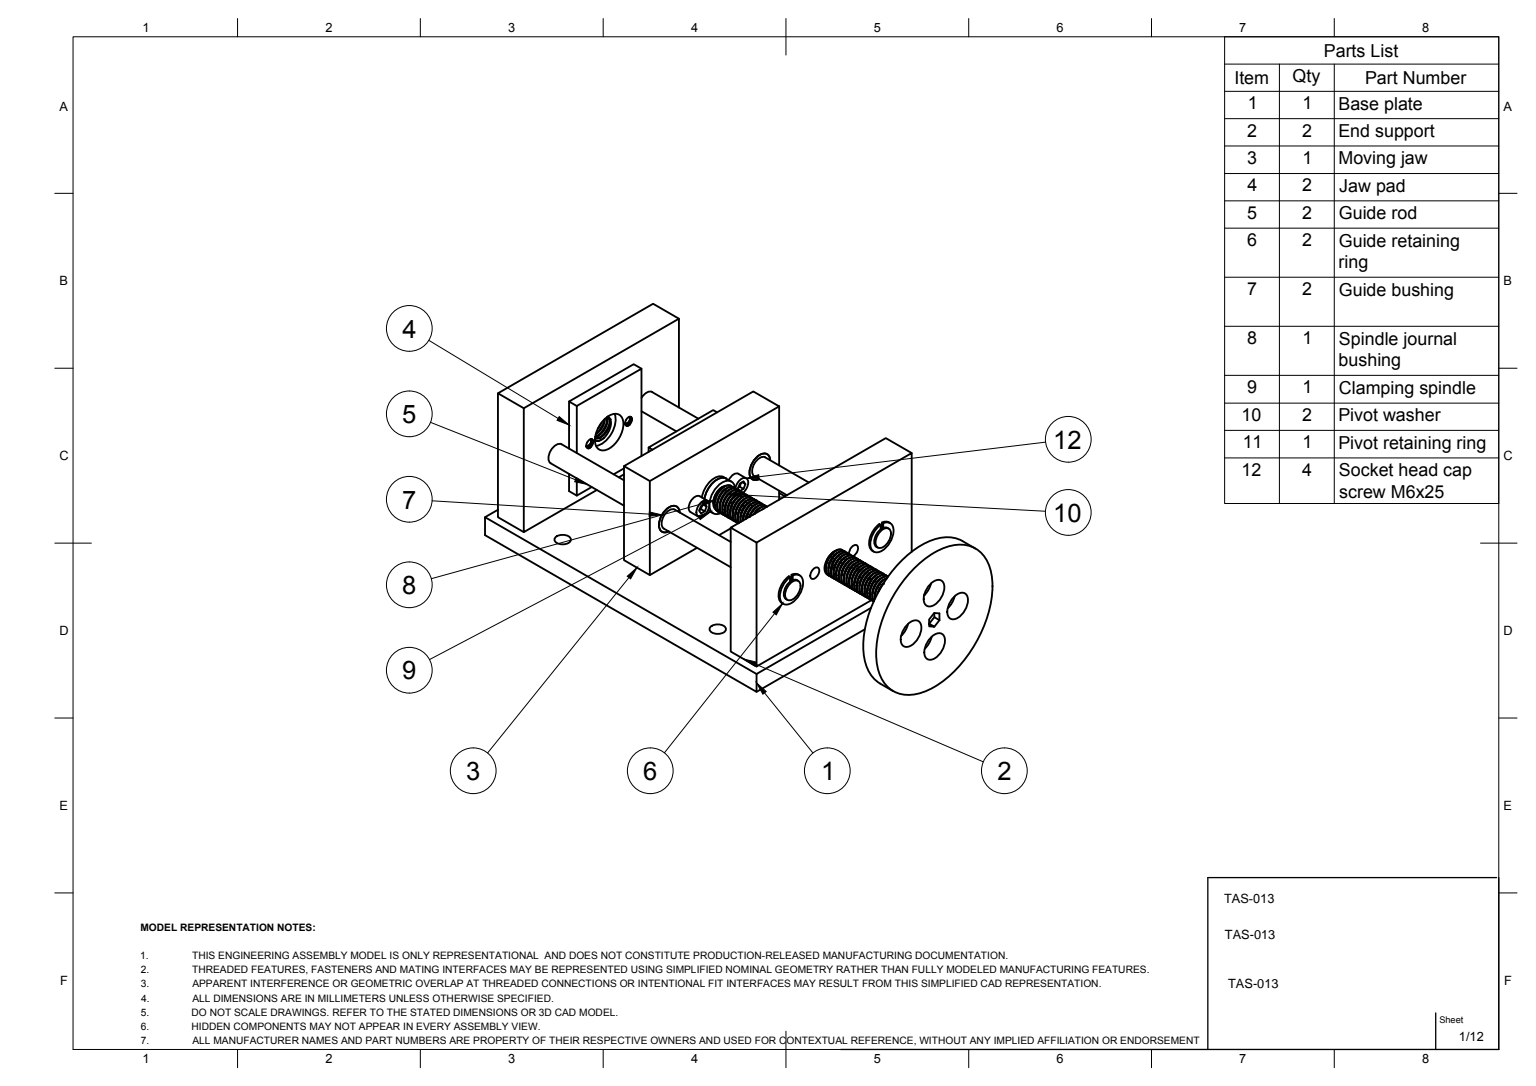
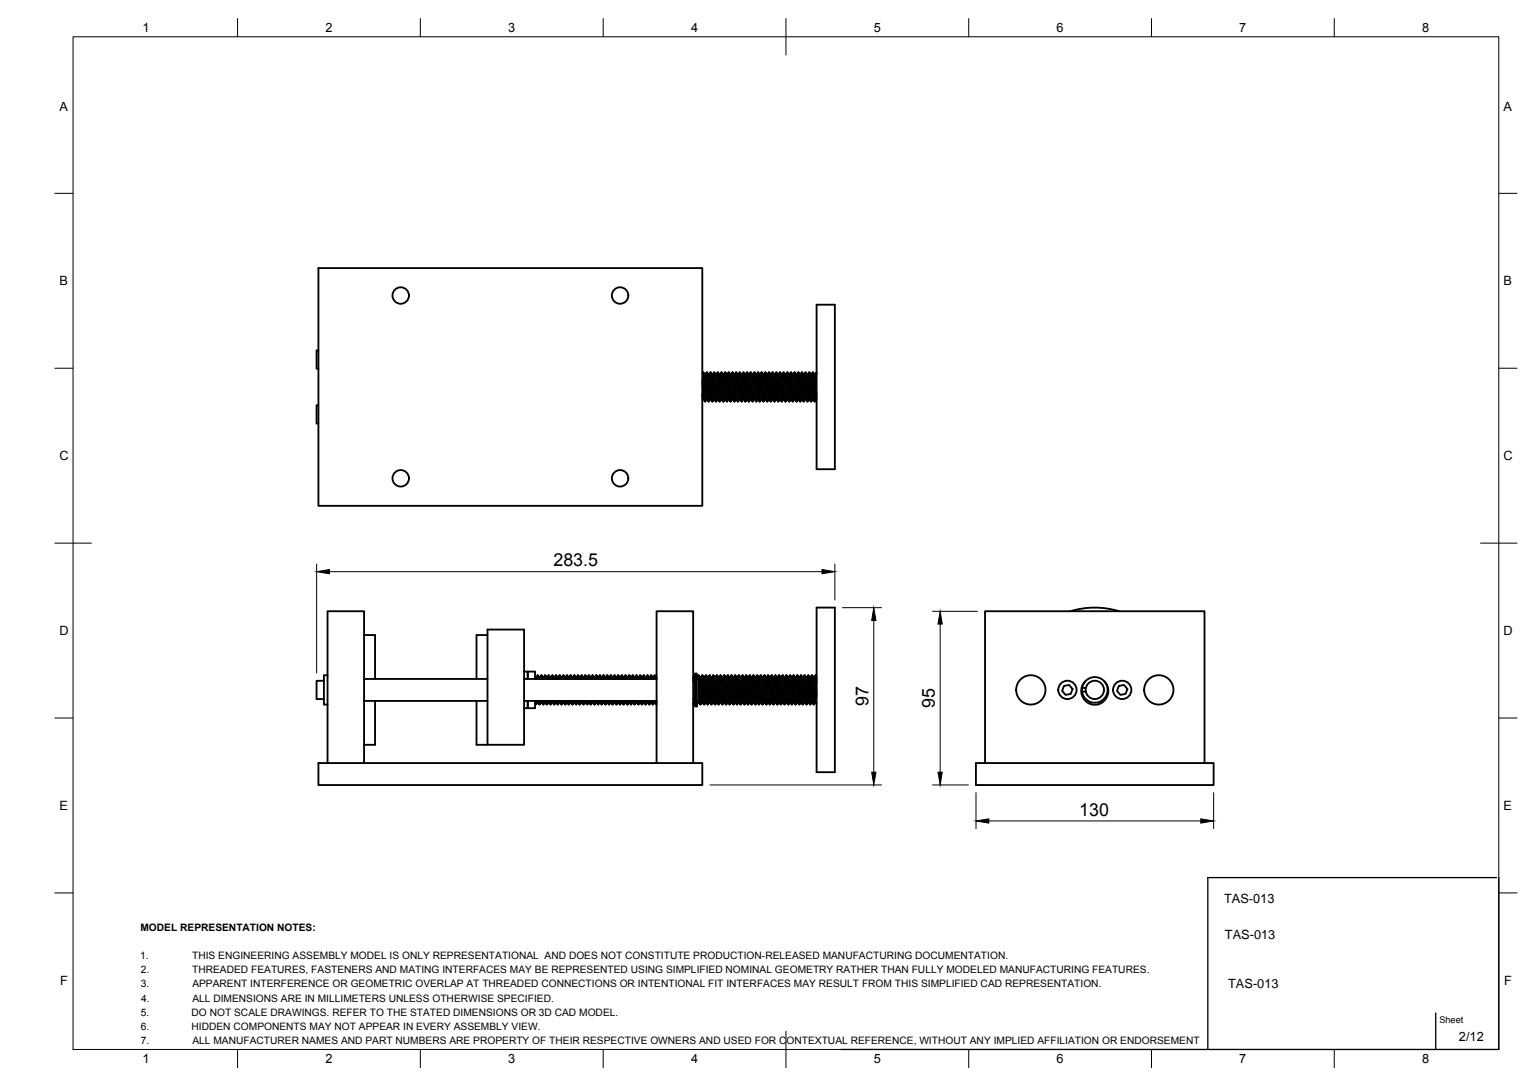
ISO-10303-21;
HEADER;
/* Generated by software containing ST-Developer
 * from STEP Tools, Inc. (www.steptools.com) 
 */

FILE_DESCRIPTION(
/* description */ (
'Independent guided parallel-jaw bracket clamp. Two12mm guide rods, re
placeable bronze sleeves, captured swiveling spindle, replaceable jaw 
pads and modeled M16x2 screw. Native slider/revolute joints linked2mm 
per revolution. Nominal opening0..122 with initial28mm. Base and two i
dentical supports welded. Standard fits, weld details and clamp load r
equire engineering selection.'),
/* implementation_level */ '2;1');

FILE_NAME(
/* name */ 'TAS-013.step',
/* time_stamp */ '2026-11-14T09:15:44-08:00',
/* author */ (''),
/* organization */ (''),
/* preprocessor_version */ 'ST-DEVELOPER v20.2',
/* originating_system */ 'Autodesk Translation Framework v15.17.0.0',
/* authorisation */ '');

FILE_SCHEMA (('AUTOMOTIVE_DESIGN { 1 0 10303 214 3 1 1 }'));
ENDSEC;

DATA;
#10=MECHANICAL_DESIGN_GEOMETRIC_PRESENTATION_REPRESENTATION('',(#915,#916,
#917,#918,#919,#920,#921,#922,#923,#924,#925,#926),#105806);
#11=ITEM_DEFINED_TRANSFORMATION($,$,#7348,#7722);
#12=ITEM_DEFINED_TRANSFORMATION($,$,#7538,#7723);
#13=ITEM_DEFINED_TRANSFORMATION($,$,#7367,#7724);
#14=ITEM_DEFINED_TRANSFORMATION($,$,#7583,#7725);
#15=ITEM_DEFINED_TRANSFORMATION($,$,#7629,#7726);
#16=ITEM_DEFINED_TRANSFORMATION($,$,#7647,#7727);
#17=ITEM_DEFINED_TRANSFORMATION($,$,#7658,#7728);
#18=ITEM_DEFINED_TRANSFORMATION($,$,#7389,#7729);
#19=ITEM_DEFINED_TRANSFORMATION($,$,#7398,#7730);
#20=ITEM_DEFINED_TRANSFORMATION($,$,#7667,#7731);
#21=ITEM_DEFINED_TRANSFORMATION($,$,#7527,#7732);
#22=ITEM_DEFINED_TRANSFORMATION($,$,#7676,#7733);
#23=ITEM_DEFINED_TRANSFORMATION($,$,#7538,#7734);
#24=ITEM_DEFINED_TRANSFORMATION($,$,#7583,#7735);
#25=ITEM_DEFINED_TRANSFORMATION($,$,#7629,#7736);
#26=ITEM_DEFINED_TRANSFORMATION($,$,#7647,#7737);
#27=ITEM_DEFINED_TRANSFORMATION($,$,#7658,#7738);
#28=ITEM_DEFINED_TRANSFORMATION($,$,#7667,#7739);
#29=ITEM_DEFINED_TRANSFORMATION($,$,#7676,#7740);
#30=ITEM_DEFINED_TRANSFORMATION($,$,#7676,#7741);
#31=ITEM_DEFINED_TRANSFORMATION($,$,#7676,#7742);
#32=(
REPRESENTATION_RELATIONSHIP($,$,#105859,#105858)
REPRESENTATION_RELATIONSHIP_WITH_TRANSFORMATION(#11)
SHAPE_REPRESENTATION_RELATIONSHIP()
);
#33=(
REPRESENTATION_RELATIONSHIP($,$,#105864,#105858)
REPRESENTATION_RELATIONSHIP_WITH_TRANSFORMATION(#12)
SHAPE_REPRESENTATION_RELATIONSHIP()
);
#34=(
REPRESENTATION_RELATIONSHIP($,$,#105860,#105858)
REPRESENTATION_RELATIONSHIP_WITH_TRANSFORMATION(#13)
SHAPE_REPRESENTATION_RELATIONSHIP()
);
#35=(
REPRESENTATION_RELATIONSHIP($,$,#105865,#105858)
REPRESENTATION_RELATIONSHIP_WITH_TRANSFORMATION(#14)
SHAPE_REPRESENTATION_RELATIONSHIP()
);
#36=(
REPRESENTATION_RELATIONSHIP($,$,#105866,#105858)
REPRESENTATION_RELATIONSHIP_WITH_TRANSFORMATION(#15)
SHAPE_REPRESENTATION_RELATIONSHIP()
);
#37=(
REPRESENTATION_RELATIONSHIP($,$,#105867,#105858)
REPRESENTATION_RELATIONSHIP_WITH_TRANSFORMATION(#16)
SHAPE_REPRESENTATION_RELATIONSHIP()
);
#38=(
REPRESENTATION_RELATIONSHIP($,$,#105868,#105858)
REPRESENTATION_RELATIONSHIP_WITH_TRANSFORMATION(#17)
SHAPE_REPRESENTATION_RELATIONSHIP()
);
#39=(
REPRESENTATION_RELATIONSHIP($,$,#105861,#105858)
REPRESENTATION_RELATIONSHIP_WITH_TRANSFORMATION(#18)
SHAPE_REPRESENTATION_RELATIONSHIP()
);
#40=(
REPRESENTATION_RELATIONSHIP($,$,#105862,#105858)
REPRESENTATION_RELATIONSHIP_WITH_TRANSFORMATION(#19)
SHAPE_REPRESENTATION_RELATIONSHIP()
);
#41=(
REPRESENTATION_RELATIONSHIP($,$,#105869,#105858)
REPRESENTATION_RELATIONSHIP_WITH_TRANSFORMATION(#20)
SHAPE_REPRESENTATION_RELATIONSHIP()
);
#42=(
REPRESENTATION_RELATIONSHIP($,$,#105863,#105858)
REPRESENTATION_RELATIONSHIP_WITH_TRANSFORMATION(#21)
SHAPE_REPRESENTATION_RELATIONSHIP()
);
#43=(
REPRESENTATION_RELATIONSHIP($,$,#105870,#105858)
REPRESENTATION_RELATIONSHIP_WITH_TRANSFORMATION(#22)
SHAPE_REPRESENTATION_RELATIONSHIP()
);
#44=(
REPRESENTATION_RELATIONSHIP($,$,#105864,#105858)
REPRESENTATION_RELATIONSHIP_WITH_TRANSFORMATION(#23)
SHAPE_REPRESENTATION_RELATIONSHIP()
);
#45=(
REPRESENTATION_RELATIONSHIP($,$,#105865,#105858)
REPRESENTATION_RELATIONSHIP_WITH_TRANSFORMATION(#24)
SHAPE_REPRESENTATION_RELATIONSHIP()
);
#46=(
REPRESENTATION_RELATIONSHIP($,$,#105866,#105858)
REPRESENTATION_RELATIONSHIP_WITH_TRANSFORMATION(#25)
SHAPE_REPRESENTATION_RELATIONSHIP()
);
#47=(
REPRESENTATION_RELATIONSHIP($,$,#105867,#105858)
REPRESENTATION_RELATIONSHIP_WITH_TRANSFORMATION(#26)
SHAPE_REPRESENTATION_RELATIONSHIP()
);
#48=(
REPRESENTATION_RELATIONSHIP($,$,#105868,#105858)
REPRESENTATION_RELATIONSHIP_WITH_TRANSFORMATION(#27)
SHAPE_REPRESENTATION_RELATIONSHIP()
);
#49=(
REPRESENTATION_RELATIONSHIP($,$,#105869,#105858)
REPRESENTATION_RELATIONSHIP_WITH_TRANSFORMATION(#28)
SHAPE_REPRESENTATION_RELATIONSHIP()
);
#50=(
REPRESENTATION_RELATIONSHIP($,$,#105870,#105858)
REPRESENTATION_RELATIONSHIP_WITH_TRANSFORMATION(#29)
SHAPE_REPRESENTATION_RELATIONSHIP()
);
#51=(
REPRESENTATION_RELATIONSHIP($,$,#105870,#105858)
REPRESENTATION_RELATIONSHIP_WITH_TRANSFORMATION(#30)
SHAPE_REPRESENTATION_RELATIONSHIP()
);
#52=(
REPRESENTATION_RELATIONSHIP($,$,#105870,#105858)
REPRESENTATION_RELATIONSHIP_WITH_TRANSFORMATION(#31)
SHAPE_REPRESENTATION_RELATIONSHIP()
);
#53=CONTEXT_DEPENDENT_SHAPE_REPRESENTATION(#32,#105837);
#54=CONTEXT_DEPENDENT_SHAPE_REPRESENTATION(#33,#105838);
#55=CONTEXT_DEPENDENT_SHAPE_REPRESENTATION(#34,#105839);
#56=CONTEXT_DEPENDENT_SHAPE_REPRESENTATION(#35,#105840);
#57=CONTEXT_DEPENDENT_SHAPE_REPRESENTATION(#36,#105841);
#58=CONTEXT_DEPENDENT_SHAPE_REPRESENTATION(#37,#105842);
#59=CONTEXT_DEPENDENT_SHAPE_REPRESENTATION(#38,#105843);
#60=CONTEXT_DEPENDENT_SHAPE_REPRESENTATION(#39,#105844);
#61=CONTEXT_DEPENDENT_SHAPE_REPRESENTATION(#40,#105845);
#62=CONTEXT_DEPENDENT_SHAPE_REPRESENTATION(#41,#105846);
#63=CONTEXT_DEPENDENT_SHAPE_REPRESENTATION(#42,#105847);
#64=CONTEXT_DEPENDENT_SHAPE_REPRESENTATION(#43,#105848);
#65=CONTEXT_DEPENDENT_SHAPE_REPRESENTATION(#44,#105849);
#66=CONTEXT_DEPENDENT_SHAPE_REPRESENTATION(#45,#105850);
#67=CONTEXT_DEPENDENT_SHAPE_REPRESENTATION(#46,#105851);
#68=CONTEXT_DEPENDENT_SHAPE_REPRESENTATION(#47,#105852);
#69=CONTEXT_DEPENDENT_SHAPE_REPRESENTATION(#48,#105853);
#70=CONTEXT_DEPENDENT_SHAPE_REPRESENTATION(#49,#105854);
#71=CONTEXT_DEPENDENT_SHAPE_REPRESENTATION(#50,#105855);
#72=CONTEXT_DEPENDENT_SHAPE_REPRESENTATION(#51,#105856);
#73=CONTEXT_DEPENDENT_SHAPE_REPRESENTATION(#52,#105857);
#74=NEXT_ASSEMBLY_USAGE_OCCURRENCE('Base plate:1','Base plate:1',
'Base plate:1',#105872,#105873,'Base plate:1');
#75=NEXT_ASSEMBLY_USAGE_OCCURRENCE('End support:1','End support:1',
'End support:1',#105872,#105878,'End support:1');
#76=NEXT_ASSEMBLY_USAGE_OCCURRENCE('Moving jaw:1','Moving jaw:1',
'Moving jaw:1',#105872,#105874,'Moving jaw:1');
#77=NEXT_ASSEMBLY_USAGE_OCCURRENCE('Jaw pad:1','Jaw pad:1','Jaw pad:1',
#105872,#105879,'Jaw pad:1');
#78=NEXT_ASSEMBLY_USAGE_OCCURRENCE('Guide rod:1','Guide rod:1',
'Guide rod:1',#105872,#105880,'Guide rod:1');
#79=NEXT_ASSEMBLY_USAGE_OCCURRENCE('Guide retaining ring:1',
'Guide retaining ring:1','Guide retaining ring:1',#105872,#105881,
'Guide retaining ring:1');
#80=NEXT_ASSEMBLY_USAGE_OCCURRENCE('Guide bushing:1','Guide bushing:1',
'Guide bushing:1',#105872,#105882,'Guide bushing:1');
#81=NEXT_ASSEMBLY_USAGE_OCCURRENCE('Spindle journal bushing:1',
'Spindle journal bushing:1','Spindle journal bushing:1',#105872,#105875,
'Spindle journal bushing:1');
#82=NEXT_ASSEMBLY_USAGE_OCCURRENCE('Clamping spindle:1',
'Clamping spindle:1','Clamping spindle:1',#105872,#105876,
'Clamping spindle:1');
#83=NEXT_ASSEMBLY_USAGE_OCCURRENCE('Pivot washer:1','Pivot washer:1',
'Pivot washer:1',#105872,#105883,'Pivot washer:1');
#84=NEXT_ASSEMBLY_USAGE_OCCURRENCE('Pivot retaining ring:1',
'Pivot retaining ring:1','Pivot retaining ring:1',#105872,#105877,
'Pivot retaining ring:1');
#85=NEXT_ASSEMBLY_USAGE_OCCURRENCE('Socket head cap screw M6x25:1',
'Socket head cap screw M6x25:1','Socket head cap screw M6x25:1',#105872,
#105884,'Socket head cap screw M6x25:1');
#86=NEXT_ASSEMBLY_USAGE_OCCURRENCE('End support:2','End support:2',
'End support:2',#105872,#105878,'End support:2');
#87=NEXT_ASSEMBLY_USAGE_OCCURRENCE('Jaw pad:2','Jaw pad:2','Jaw pad:2',
#105872,#105879,'Jaw pad:2');
#88=NEXT_ASSEMBLY_USAGE_OCCURRENCE('Guide rod:2','Guide rod:2',
'Guide rod:2',#105872,#105880,'Guide rod:2');
#89=NEXT_ASSEMBLY_USAGE_OCCURRENCE('Guide retaining ring:2',
'Guide retaining ring:2','Guide retaining ring:2',#105872,#105881,
'Guide retaining ring:2');
#90=NEXT_ASSEMBLY_USAGE_OCCURRENCE('Guide bushing:2','Guide bushing:2',
'Guide bushing:2',#105872,#105882,'Guide bushing:2');
#91=NEXT_ASSEMBLY_USAGE_OCCURRENCE('Pivot washer:2','Pivot washer:2',
'Pivot washer:2',#105872,#105883,'Pivot washer:2');
#92=NEXT_ASSEMBLY_USAGE_OCCURRENCE('Socket head cap screw M6x25:2',
'Socket head cap screw M6x25:2','Socket head cap screw M6x25:2',#105872,
#105884,'Socket head cap screw M6x25:2');
#93=NEXT_ASSEMBLY_USAGE_OCCURRENCE('Socket head cap screw M6x25:3',
'Socket head cap screw M6x25:3','Socket head cap screw M6x25:3',#105872,
#105884,'Socket head cap screw M6x25:3');
#94=NEXT_ASSEMBLY_USAGE_OCCURRENCE('Socket head cap screw M6x25:4',
'Socket head cap screw M6x25:4','Socket head cap screw M6x25:4',#105872,
#105884,'Socket head cap screw M6x25:4');
#95=B_SPLINE_SURFACE_WITH_KNOTS('',3,3,((#67139,#67140,#67141,#67142,#67143,
#67144,#67145,#67146,#67147,#67148,#67149,#67150,#67151,#67152,#67153,#67154,
#67155,#67156,#67157,#67158,#67159,#67160,#67161,#67162,#67163,#67164,#67165,
#67166,#67167,#67168,#67169,#67170,#67171,#67172,#67173,#67174,#67175,#67176,
#67177,#67178,#67179,#67180,#67181,#67182,#67183,#67184,#67185,#67186,#67187,
#67188,#67189,#67190,#67191,#67192,#67193,#67194,#67195,#67196,#67197,#67198,
#67199,#67200,#67201,#67202,#67203,#67204,#67205,#67206,#67207,#67208,#67209,
#67210,#67211,#67212,#67213,#67214,#67215,#67216,#67217,#67218,#67219,#67220,
#67221,#67222,#67223,#67224,#67225,#67226,#67227,#67228,#67229,#67230,#67231,
#67232,#67233,#67234,#67235,#67236,#67237,#67238,#67239,#67240,#67241,#67242,
#67243,#67244,#67245,#67246,#67247,#67248,#67249,#67250,#67251,#67252,#67253,
#67254,#67255,#67256,#67257,#67258,#67259,#67260,#67261,#67262,#67263,#67264,
#67265,#67266,#67267,#67268,#67269,#67270,#67271,#67272,#67273,#67274,#67275,
#67276,#67277,#67278,#67279,#67280,#67281,#67282,#67283,#67284,#67285,#67286,
#67287,#67288,#67289,#67290,#67291,#67292,#67293,#67294,#67295,#67296,#67297,
#67298,#67299,#67300,#67301,#67302,#67303,#67304,#67305,#67306,#67307,#67308,
#67309,#67310,#67311,#67312,#67313,#67314,#67315,#67316,#67317,#67318,#67319,
#67320,#67321,#67322,#67323,#67324,#67325,#67326,#67327,#67328,#67329,#67330,
#67331,#67332,#67333,#67334,#67335,#67336,#67337,#67338,#67339,#67340,#67341,
#67342,#67343,#67344,#67345,#67346,#67347,#67348,#67349,#67350,#67351,#67352,
#67353,#67354,#67355,#67356,#67357,#67358,#67359,#67360,#67361,#67362,#67363,
#67364,#67365,#67366,#67367,#67368,#67369,#67370,#67371,#67372,#67373,#67374,
#67375,#67376,#67377,#67378,#67379,#67380,#67381,#67382,#67383,#67384,#67385,
#67386,#67387,#67388,#67389,#67390,#67391,#67392,#67393,#67394,#67395,#67396,
#67397,#67398,#67399,#67400,#67401,#67402,#67403,#67404,#67405,#67406,#67407,
#67408,#67409,#67410,#67411,#67412,#67413,#67414,#67415,#67416,#67417,#67418,
#67419,#67420,#67421,#67422,#67423,#67424,#67425,#67426,#67427,#67428,#67429,
#67430,#67431,#67432,#67433,#67434,#67435,#67436,#67437,#67438,#67439,#67440,
#67441,#67442,#67443,#67444,#67445,#67446,#67447,#67448,#67449,#67450,#67451,
#67452,#67453,#67454,#67455,#67456,#67457,#67458,#67459,#67460,#67461,#67462,
#67463,#67464,#67465,#67466,#67467,#67468,#67469,#67470,#67471,#67472,#67473,
#67474,#67475,#67476,#67477,#67478,#67479,#67480,#67481,#67482,#67483,#67484,
#67485,#67486,#67487,#67488,#67489,#67490,#67491,#67492,#67493,#67494,#67495,
#67496,#67497,#67498,#67499,#67500,#67501,#67502,#67503,#67504,#67505,#67506,
#67507,#67508,#67509,#67510,#67511,#67512,#67513,#67514,#67515,#67516,#67517,
#67518,#67519,#67520,#67521,#67522,#67523,#67524,#67525,#67526,#67527,#67528,
#67529,#67530,#67531,#67532,#67533,#67534,#67535,#67536,#67537,#67538,#67539,
#67540,#67541,#67542,#67543,#67544,#67545,#67546,#67547,#67548,#67549,#67550,
#67551,#67552,#67553,#67554,#67555,#67556,#67557,#67558,#67559,#67560,#67561,
#67562,#67563,#67564,#67565,#67566,#67567,#67568,#67569,#67570,#67571,#67572,
#67573,#67574,#67575,#67576,#67577,#67578,#67579,#67580,#67581,#67582,#67583,
#67584,#67585,#67586,#67587,#67588,#67589,#67590,#67591,#67592,#67593,#67594,
#67595,#67596,#67597,#67598,#67599,#67600,#67601,#67602,#67603,#67604,#67605,
#67606,#67607,#67608,#67609,#67610,#67611,#67612,#67613,#67614,#67615,#67616,
#67617,#67618,#67619,#67620,#67621,#67622,#67623,#67624,#67625,#67626,#67627,
#67628,#67629,#67630,#67631,#67632,#67633,#67634,#67635,#67636,#67637,#67638,
#67639,#67640,#67641,#67642,#67643,#67644,#67645,#67646,#67647,#67648,#67649,
#67650,#67651,#67652,#67653,#67654,#67655,#67656,#67657,#67658,#67659,#67660,
#67661,#67662,#67663,#67664,#67665,#67666,#67667,#67668,#67669,#67670,#67671,
#67672,#67673,#67674,#67675,#67676,#67677,#67678,#67679,#67680,#67681,#67682,
#67683,#67684,#67685,#67686,#67687,#67688,#67689,#67690,#67691,#67692,#67693,
#67694,#67695,#67696),(#67697,#67698,#67699,#67700,#67701,#67702,#67703,
#67704,#67705,#67706,#67707,#67708,#67709,#67710,#67711,#67712,#67713,#67714,
#67715,#67716,#67717,#67718,#67719,#67720,#67721,#67722,#67723,#67724,#67725,
#67726,#67727,#67728,#67729,#67730,#67731,#67732,#67733,#67734,#67735,#67736,
#67737,#67738,#67739,#67740,#67741,#67742,#67743,#67744,#67745,#67746,#67747,
#67748,#67749,#67750,#67751,#67752,#67753,#67754,#67755,#67756,#67757,#67758,
#67759,#67760,#67761,#67762,#67763,#67764,#67765,#67766,#67767,#67768,#67769,
#67770,#67771,#67772,#67773,#67774,#67775,#67776,#67777,#67778,#67779,#67780,
#67781,#67782,#67783,#67784,#67785,#67786,#67787,#67788,#67789,#67790,#67791,
#67792,#67793,#67794,#67795,#67796,#67797,#67798,#67799,#67800,#67801,#67802,
#67803,#67804,#67805,#67806,#67807,#67808,#67809,#67810,#67811,#67812,#67813,
#67814,#67815,#67816,#67817,#67818,#67819,#67820,#67821,#67822,#67823,#67824,
#67825,#67826,#67827,#67828,#67829,#67830,#67831,#67832,#67833,#67834,#67835,
#67836,#67837,#67838,#67839,#67840,#67841,#67842,#67843,#67844,#67845,#67846,
#67847,#67848,#67849,#67850,#67851,#67852,#67853,#67854,#67855,#67856,#67857,
#67858,#67859,#67860,#67861,#67862,#67863,#67864,#67865,#67866,#67867,#67868,
#67869,#67870,#67871,#67872,#67873,#67874,#67875,#67876,#67877,#67878,#67879,
#67880,#67881,#67882,#67883,#67884,#67885,#67886,#67887,#67888,#67889,#67890,
#67891,#67892,#67893,#67894,#67895,#67896,#67897,#67898,#67899,#67900,#67901,
#67902,#67903,#67904,#67905,#67906,#67907,#67908,#67909,#67910,#67911,#67912,
#67913,#67914,#67915,#67916,#67917,#67918,#67919,#67920,#67921,#67922,#67923,
#67924,#67925,#67926,#67927,#67928,#67929,#67930,#67931,#67932,#67933,#67934,
#67935,#67936,#67937,#67938,#67939,#67940,#67941,#67942,#67943,#67944,#67945,
#67946,#67947,#67948,#67949,#67950,#67951,#67952,#67953,#67954,#67955,#67956,
#67957,#67958,#67959,#67960,#67961,#67962,#67963,#67964,#67965,#67966,#67967,
#67968,#67969,#67970,#67971,#67972,#67973,#67974,#67975,#67976,#67977,#67978,
#67979,#67980,#67981,#67982,#67983,#67984,#67985,#67986,#67987,#67988,#67989,
#67990,#67991,#67992,#67993,#67994,#67995,#67996,#67997,#67998,#67999,#68000,
#68001,#68002,#68003,#68004,#68005,#68006,#68007,#68008,#68009,#68010,#68011,
#68012,#68013,#68014,#68015,#68016,#68017,#68018,#68019,#68020,#68021,#68022,
#68023,#68024,#68025,#68026,#68027,#68028,#68029,#68030,#68031,#68032,#68033,
#68034,#68035,#68036,#68037,#68038,#68039,#68040,#68041,#68042,#68043,#68044,
#68045,#68046,#68047,#68048,#68049,#68050,#68051,#68052,#68053,#68054,#68055,
#68056,#68057,#68058,#68059,#68060,#68061,#68062,#68063,#68064,#68065,#68066,
#68067,#68068,#68069,#68070,#68071,#68072,#68073,#68074,#68075,#68076,#68077,
#68078,#68079,#68080,#68081,#68082,#68083,#68084,#68085,#68086,#68087,#68088,
#68089,#68090,#68091,#68092,#68093,#68094,#68095,#68096,#68097,#68098,#68099,
#68100,#68101,#68102,#68103,#68104,#68105,#68106,#68107,#68108,#68109,#68110,
#68111,#68112,#68113,#68114,#68115,#68116,#68117,#68118,#68119,#68120,#68121,
#68122,#68123,#68124,#68125,#68126,#68127,#68128,#68129,#68130,#68131,#68132,
#68133,#68134,#68135,#68136,#68137,#68138,#68139,#68140,#68141,#68142,#68143,
#68144,#68145,#68146,#68147,#68148,#68149,#68150,#68151,#68152,#68153,#68154,
#68155,#68156,#68157,#68158,#68159,#68160,#68161,#68162,#68163,#68164,#68165,
#68166,#68167,#68168,#68169,#68170,#68171,#68172,#68173,#68174,#68175,#68176,
#68177,#68178,#68179,#68180,#68181,#68182,#68183,#68184,#68185,#68186,#68187,
#68188,#68189,#68190,#68191,#68192,#68193,#68194,#68195,#68196,#68197,#68198,
#68199,#68200,#68201,#68202,#68203,#68204,#68205,#68206,#68207,#68208,#68209,
#68210,#68211,#68212,#68213,#68214,#68215,#68216,#68217,#68218,#68219,#68220,
#68221,#68222,#68223,#68224,#68225,#68226,#68227,#68228,#68229,#68230,#68231,
#68232,#68233,#68234,#68235,#68236,#68237,#68238,#68239,#68240,#68241,#68242,
#68243,#68244,#68245,#68246,#68247,#68248,#68249,#68250,#68251,#68252,#68253,
#68254),(#68255,#68256,#68257,#68258,#68259,#68260,#68261,#68262,#68263,
#68264,#68265,#68266,#68267,#68268,#68269,#68270,#68271,#68272,#68273,#68274,
#68275,#68276,#68277,#68278,#68279,#68280,#68281,#68282,#68283,#68284,#68285,
#68286,#68287,#68288,#68289,#68290,#68291,#68292,#68293,#68294,#68295,#68296,
#68297,#68298,#68299,#68300,#68301,#68302,#68303,#68304,#68305,#68306,#68307,
#68308,#68309,#68310,#68311,#68312,#68313,#68314,#68315,#68316,#68317,#68318,
#68319,#68320,#68321,#68322,#68323,#68324,#68325,#68326,#68327,#68328,#68329,
#68330,#68331,#68332,#68333,#68334,#68335,#68336,#68337,#68338,#68339,#68340,
#68341,#68342,#68343,#68344,#68345,#68346,#68347,#68348,#68349,#68350,#68351,
#68352,#68353,#68354,#68355,#68356,#68357,#68358,#68359,#68360,#68361,#68362,
#68363,#68364,#68365,#68366,#68367,#68368,#68369,#68370,#68371,#68372,#68373,
#68374,#68375,#68376,#68377,#68378,#68379,#68380,#68381,#68382,#68383,#68384,
#68385,#68386,#68387,#68388,#68389,#68390,#68391,#68392,#68393,#68394,#68395,
#68396,#68397,#68398,#68399,#68400,#68401,#68402,#68403,#68404,#68405,#68406,
#68407,#68408,#68409,#68410,#68411,#68412,#68413,#68414,#68415,#68416,#68417,
#68418,#68419,#68420,#68421,#68422,#68423,#68424,#68425,#68426,#68427,#68428,
#68429,#68430,#68431,#68432,#68433,#68434,#68435,#68436,#68437,#68438,#68439,
#68440,#68441,#68442,#68443,#68444,#68445,#68446,#68447,#68448,#68449,#68450,
#68451,#68452,#68453,#68454,#68455,#68456,#68457,#68458,#68459,#68460,#68461,
#68462,#68463,#68464,#68465,#68466,#68467,#68468,#68469,#68470,#68471,#68472,
#68473,#68474,#68475,#68476,#68477,#68478,#68479,#68480,#68481,#68482,#68483,
#68484,#68485,#68486,#68487,#68488,#68489,#68490,#68491,#68492,#68493,#68494,
#68495,#68496,#68497,#68498,#68499,#68500,#68501,#68502,#68503,#68504,#68505,
#68506,#68507,#68508,#68509,#68510,#68511,#68512,#68513,#68514,#68515,#68516,
#68517,#68518,#68519,#68520,#68521,#68522,#68523,#68524,#68525,#68526,#68527,
#68528,#68529,#68530,#68531,#68532,#68533,#68534,#68535,#68536,#68537,#68538,
#68539,#68540,#68541,#68542,#68543,#68544,#68545,#68546,#68547,#68548,#68549,
#68550,#68551,#68552,#68553,#68554,#68555,#68556,#68557,#68558,#68559,#68560,
#68561,#68562,#68563,#68564,#68565,#68566,#68567,#68568,#68569,#68570,#68571,
#68572,#68573,#68574,#68575,#68576,#68577,#68578,#68579,#68580,#68581,#68582,
#68583,#68584,#68585,#68586,#68587,#68588,#68589,#68590,#68591,#68592,#68593,
#68594,#68595,#68596,#68597,#68598,#68599,#68600,#68601,#68602,#68603,#68604,
#68605,#68606,#68607,#68608,#68609,#68610,#68611,#68612,#68613,#68614,#68615,
#68616,#68617,#68618,#68619,#68620,#68621,#68622,#68623,#68624,#68625,#68626,
#68627,#68628,#68629,#68630,#68631,#68632,#68633,#68634,#68635,#68636,#68637,
#68638,#68639,#68640,#68641,#68642,#68643,#68644,#68645,#68646,#68647,#68648,
#68649,#68650,#68651,#68652,#68653,#68654,#68655,#68656,#68657,#68658,#68659,
#68660,#68661,#68662,#68663,#68664,#68665,#68666,#68667,#68668,#68669,#68670,
#68671,#68672,#68673,#68674,#68675,#68676,#68677,#68678,#68679,#68680,#68681,
#68682,#68683,#68684,#68685,#68686,#68687,#68688,#68689,#68690,#68691,#68692,
#68693,#68694,#68695,#68696,#68697,#68698,#68699,#68700,#68701,#68702,#68703,
#68704,#68705,#68706,#68707,#68708,#68709,#68710,#68711,#68712,#68713,#68714,
#68715,#68716,#68717,#68718,#68719,#68720,#68721,#68722,#68723,#68724,#68725,
#68726,#68727,#68728,#68729,#68730,#68731,#68732,#68733,#68734,#68735,#68736,
#68737,#68738,#68739,#68740,#68741,#68742,#68743,#68744,#68745,#68746,#68747,
#68748,#68749,#68750,#68751,#68752,#68753,#68754,#68755,#68756,#68757,#68758,
#68759,#68760,#68761,#68762,#68763,#68764,#68765,#68766,#68767,#68768,#68769,
#68770,#68771,#68772,#68773,#68774,#68775,#68776,#68777,#68778,#68779,#68780,
#68781,#68782,#68783,#68784,#68785,#68786,#68787,#68788,#68789,#68790,#68791,
#68792,#68793,#68794,#68795,#68796,#68797,#68798,#68799,#68800,#68801,#68802,
#68803,#68804,#68805,#68806,#68807,#68808,#68809,#68810,#68811,#68812),
(#68813,#68814,#68815,#68816,#68817,#68818,#68819,#68820,#68821,#68822,
#68823,#68824,#68825,#68826,#68827,#68828,#68829,#68830,#68831,#68832,#68833,
#68834,#68835,#68836,#68837,#68838,#68839,#68840,#68841,#68842,#68843,#68844,
#68845,#68846,#68847,#68848,#68849,#68850,#68851,#68852,#68853,#68854,#68855,
#68856,#68857,#68858,#68859,#68860,#68861,#68862,#68863,#68864,#68865,#68866,
#68867,#68868,#68869,#68870,#68871,#68872,#68873,#68874,#68875,#68876,#68877,
#68878,#68879,#68880,#68881,#68882,#68883,#68884,#68885,#68886,#68887,#68888,
#68889,#68890,#68891,#68892,#68893,#68894,#68895,#68896,#68897,#68898,#68899,
#68900,#68901,#68902,#68903,#68904,#68905,#68906,#68907,#68908,#68909,#68910,
#68911,#68912,#68913,#68914,#68915,#68916,#68917,#68918,#68919,#68920,#68921,
#68922,#68923,#68924,#68925,#68926,#68927,#68928,#68929,#68930,#68931,#68932,
#68933,#68934,#68935,#68936,#68937,#68938,#68939,#68940,#68941,#68942,#68943,
#68944,#68945,#68946,#68947,#68948,#68949,#68950,#68951,#68952,#68953,#68954,
#68955,#68956,#68957,#68958,#68959,#68960,#68961,#68962,#68963,#68964,#68965,
#68966,#68967,#68968,#68969,#68970,#68971,#68972,#68973,#68974,#68975,#68976,
#68977,#68978,#68979,#68980,#68981,#68982,#68983,#68984,#68985,#68986,#68987,
#68988,#68989,#68990,#68991,#68992,#68993,#68994,#68995,#68996,#68997,#68998,
#68999,#69000,#69001,#69002,#69003,#69004,#69005,#69006,#69007,#69008,#69009,
#69010,#69011,#69012,#69013,#69014,#69015,#69016,#69017,#69018,#69019,#69020,
#69021,#69022,#69023,#69024,#69025,#69026,#69027,#69028,#69029,#69030,#69031,
#69032,#69033,#69034,#69035,#69036,#69037,#69038,#69039,#69040,#69041,#69042,
#69043,#69044,#69045,#69046,#69047,#69048,#69049,#69050,#69051,#69052,#69053,
#69054,#69055,#69056,#69057,#69058,#69059,#69060,#69061,#69062,#69063,#69064,
#69065,#69066,#69067,#69068,#69069,#69070,#69071,#69072,#69073,#69074,#69075,
#69076,#69077,#69078,#69079,#69080,#69081,#69082,#69083,#69084,#69085,#69086,
#69087,#69088,#69089,#69090,#69091,#69092,#69093,#69094,#69095,#69096,#69097,
#69098,#69099,#69100,#69101,#69102,#69103,#69104,#69105,#69106,#69107,#69108,
#69109,#69110,#69111,#69112,#69113,#69114,#69115,#69116,#69117,#69118,#69119,
#69120,#69121,#69122,#69123,#69124,#69125,#69126,#69127,#69128,#69129,#69130,
#69131,#69132,#69133,#69134,#69135,#69136,#69137,#69138,#69139,#69140,#69141,
#69142,#69143,#69144,#69145,#69146,#69147,#69148,#69149,#69150,#69151,#69152,
#69153,#69154,#69155,#69156,#69157,#69158,#69159,#69160,#69161,#69162,#69163,
#69164,#69165,#69166,#69167,#69168,#69169,#69170,#69171,#69172,#69173,#69174,
#69175,#69176,#69177,#69178,#69179,#69180,#69181,#69182,#69183,#69184,#69185,
#69186,#69187,#69188,#69189,#69190,#69191,#69192,#69193,#69194,#69195,#69196,
#69197,#69198,#69199,#69200,#69201,#69202,#69203,#69204,#69205,#69206,#69207,
#69208,#69209,#69210,#69211,#69212,#69213,#69214,#69215,#69216,#69217,#69218,
#69219,#69220,#69221,#69222,#69223,#69224,#69225,#69226,#69227,#69228,#69229,
#69230,#69231,#69232,#69233,#69234,#69235,#69236,#69237,#69238,#69239,#69240,
#69241,#69242,#69243,#69244,#69245,#69246,#69247,#69248,#69249,#69250,#69251,
#69252,#69253,#69254,#69255,#69256,#69257,#69258,#69259,#69260,#69261,#69262,
#69263,#69264,#69265,#69266,#69267,#69268,#69269,#69270,#69271,#69272,#69273,
#69274,#69275,#69276,#69277,#69278,#69279,#69280,#69281,#69282,#69283,#69284,
#69285,#69286,#69287,#69288,#69289,#69290,#69291,#69292,#69293,#69294,#69295,
#69296,#69297,#69298,#69299,#69300,#69301,#69302,#69303,#69304,#69305,#69306,
#69307,#69308,#69309,#69310,#69311,#69312,#69313,#69314,#69315,#69316,#69317,
#69318,#69319,#69320,#69321,#69322,#69323,#69324,#69325,#69326,#69327,#69328,
#69329,#69330,#69331,#69332,#69333,#69334,#69335,#69336,#69337,#69338,#69339,
#69340,#69341,#69342,#69343,#69344,#69345,#69346,#69347,#69348,#69349,#69350,
#69351,#69352,#69353,#69354,#69355,#69356,#69357,#69358,#69359,#69360,#69361,
#69362,#69363,#69364,#69365,#69366,#69367,#69368,#69369,#69370)),
 .UNSPECIFIED.,.F.,.F.,.F.,(4,4),(4,1,1,1,1,1,1,1,1,1,1,1,1,1,1,1,1,1,1,
1,1,1,1,1,1,1,1,1,1,1,1,1,1,1,1,1,1,1,1,1,1,1,1,1,1,1,1,1,1,1,1,1,1,1,1,
1,1,1,1,1,1,1,1,1,1,1,1,1,1,1,1,1,1,1,1,1,1,1,1,1,1,1,1,1,1,1,1,1,1,1,1,
1,1,1,1,1,1,1,1,1,1,1,1,1,1,1,1,1,1,1,1,1,1,1,1,1,1,1,1,1,1,1,1,1,1,1,1,
1,1,1,1,1,1,1,1,1,1,1,1,1,1,1,1,1,1,1,1,1,1,1,1,1,1,1,1,1,1,1,1,1,1,1,1,
1,1,1,1,1,1,1,1,1,1,1,1,1,1,1,1,1,1,1,1,1,1,1,1,1,1,1,1,1,1,1,1,1,1,1,1,
1,1,1,1,1,1,1,1,1,1,1,1,1,1,1,1,1,1,1,1,1,1,1,1,1,1,1,1,1,1,1,1,1,1,1,1,
1,1,1,1,1,1,1,1,1,1,1,1,1,1,1,1,1,1,1,1,1,1,1,1,1,1,1,1,1,1,1,1,1,1,1,1,
1,1,1,1,1,1,1,1,1,1,1,1,1,1,1,1,1,1,1,1,1,1,1,1,1,1,1,1,1,1,1,1,1,1,1,1,
1,1,1,1,1,1,1,1,1,1,1,1,1,1,1,1,1,1,1,1,1,1,1,1,1,1,1,1,1,1,1,1,1,1,1,1,
1,1,1,1,1,1,1,1,1,1,1,1,1,1,1,1,1,1,1,1,1,1,1,1,1,1,1,1,1,1,1,1,1,1,1,1,
1,1,1,1,1,1,1,1,1,1,1,1,1,1,1,1,1,1,1,1,1,1,1,1,1,1,1,1,1,1,1,1,1,1,1,1,
1,1,1,1,1,1,1,1,1,1,1,1,1,1,1,1,1,1,1,1,1,1,1,1,1,1,1,1,1,1,1,1,1,1,1,1,
1,1,1,1,1,1,1,1,1,1,1,1,1,1,1,1,1,1,1,1,1,1,1,1,1,1,1,1,1,1,1,1,1,1,1,1,
1,1,1,1,1,1,1,1,1,1,1,1,1,1,1,1,1,1,1,1,1,1,1,1,1,1,1,1,1,1,1,1,1,1,1,1,
1,1,1,1,1,1,1,1,1,1,1,1,1,1,1,1,1,1,1,1,1,1,1,1,1,1,1,1,1,1,1,1,4),(-0.00312009804042434,
0.132901482941916),(11.6144980695961,12.1142368518449,12.6134408558704,
13.6118488639213,14.6102568719722,15.6086648800232,16.6070728880741,17.605480896125,
18.1046849001504,18.6038889041759,19.6022969122268,20.6007049202777,21.5991129283287,
22.5975209363796,23.5959289444305,24.5943369524814,25.0935409565069,25.5927449605323,
26.5911529685832,27.5895609766342,28.5879689846851,29.586376992736,30.5847850007869,
31.5831930088378,32.0823970128633,32.5816010168887,33.5800090249397,34.5784170329906,
35.5768250410415,36.5752330490924,37.5736410571433,38.5720490651942,39.0712530692197,
39.5704570732452,40.5688650812961,41.567273089347,42.5656810973979,43.5640891054488,
44.5624971134997,45.5609051215507,46.0601091255761,46.5593131296016,47.5577211376525,
48.5561291457034,49.5545371537543,50.5529451618052,51.5513531698562,52.5497611779071,
53.0489651819325,53.548169185958,54.5465771940089,55.5449852020598,56.5433932101108,
57.5418012181617,58.5402092262126,59.5386172342635,60.037821238289,60.5370252423144,
61.5354332503653,62.5338412584163,63.5322492664672,64.5306572745181,65.529065282569,
66.5274732906199,67.0266772946454,67.5258812986708,68.5242893067218,69.5226973147727,
70.5211053228236,71.5195133308745,72.5179213389254,73.5163293469763,74.0155333510018,
74.5147373550273,75.5131453630782,76.5115533711291,77.50996137918,78.5083693872309,
79.5067773952818,80.5051854033328,81.0043894073582,81.5035934113837,82.5020014194346,
83.5004094274855,84.4988174355364,85.4972254435874,86.4956334516383,87.4940414596892,
87.9932454637146,88.4924494677401,89.490857475791,90.4892654838419,91.4876734918928,
92.4860814999438,93.4844895079947,94.4828975160456,94.9821015200711,95.4813055240965,
96.4797135321474,97.4781215401984,98.4765295482493,99.4749375563002,100.473345564351,
101.471753572402,101.970957576427,102.470161580453,103.468569588504,104.466977596555,
105.465385604606,106.463793612657,107.462201620708,108.460609628758,108.959813632784,
109.459017636809,110.45742564486,111.455833652911,112.454241660962,113.452649669013,
114.451057677064,115.449465685115,115.94866968914,116.447873693166,117.446281701217,
118.444689709268,119.443097717319,120.441505725369,121.43991373342,122.438321741471,
122.937525745497,123.436729749522,124.435137757573,125.433545765624,126.431953773675,
127.430361781726,128.428769789777,129.427177797828,129.926381801853,130.425585805879,
131.42399381393,132.42240182198,133.420809830031,134.419217838082,135.417625846133,
136.416033854184,136.91523785821,137.414441862235,138.412849870286,139.411257878337,
140.409665886388,141.408073894439,142.40648190249,143.404889910541,143.904093914566,
144.403297918591,145.401705926642,146.400113934693,147.398521942744,148.396929950795,
149.395337958846,150.393745966897,150.892949970922,151.392153974948,152.390561982999,
153.38896999105,154.387377999101,155.385786007152,156.384194015202,157.382602023253,
157.881806027279,158.381010031304,159.379418039355,160.377826047406,161.376234055457,
162.374642063508,163.373050071559,164.37145807961,164.870662083635,165.369866087661,
166.368274095712,167.366682103763,168.365090111813,169.363498119864,170.361906127915,
171.360314135966,171.859518139992,172.358722144017,173.357130152068,174.355538160119,
175.35394616817,176.352354176221,177.350762184272,178.349170192323,178.848374196348,
179.347578200374,180.345986208424,181.344394216475,182.342802224526,183.341210232577,
184.339618240628,185.338026248679,185.837230252705,186.33643425673,187.334842264781,
188.333250272832,189.331658280883,190.330066288934,191.328474296985,192.326882305035,
192.826086309061,193.325290313086,194.323698321137,195.322106329188,196.320514337239,
197.31892234529,198.317330353341,199.315738361392,199.814942365417,200.314146369443,
201.312554377494,202.310962385545,203.309370393596,204.307778401646,205.306186409697,
206.304594417748,206.803798421774,207.303002425799,208.30141043385,209.299818441901,
210.298226449952,211.296634458003,212.295042466054,213.293450474105,213.79265447813,
214.291858482156,215.290266490207,216.288674498257,217.287082506308,218.285490514359,
219.28389852241,220.282306530461,220.781510534487,221.280714538512,222.279122546563,
223.277530554614,224.275938562665,225.274346570716,226.272754578767,227.271162586818,
227.770366590843,228.269570594868,229.267978602919,230.26638661097,231.264794619021,
232.263202627072,233.261610635123,234.260018643174,234.759222647199,235.258426651225,
236.256834659276,237.255242667327,238.253650675378,239.252058683429,240.250466691479,
241.24887469953,241.748078703556,242.247282707581,243.245690715632,244.244098723683,
245.242506731734,246.240914739785,247.239322747836,248.237730755887,248.736934759912,
249.236138763938,250.234546771989,251.23295478004,252.23136278809,253.229770796141,
254.228178804192,255.226586812243,256.224994820294,257.223402828345,258.221810836396,
258.721014840421,259.220218844447,260.218626852498,261.217034860549,262.2154428686,
263.213850876651,264.212258884701,265.210666892752,265.709870896778,266.209074900803,
267.207482908854,268.205890916905,269.204298924956,270.202706933007,271.201114941058,
272.199522949109,272.698726953134,273.19793095716,274.196338965211,275.194746973262,
276.193154981312,277.191562989363,278.189970997414,279.188379005465,279.687583009491,
280.186787013516,281.185195021567,282.183603029618,283.182011037669,284.18041904572,
285.178827053771,286.177235061822,286.676439065847,287.175643069873,288.174051077923,
289.172459085974,290.170867094025,291.169275102076,292.167683110127,293.166091118178,
293.665295122204,294.164499126229,295.16290713428,296.161315142331,297.159723150382,
298.158131158433,299.156539166484,300.154947174534,300.65415117856,301.153355182585,
302.151763190636,303.150171198687,304.148579206738,305.146987214789,306.14539522284,
307.143803230891,307.643007234916,308.142211238942,309.140619246993,310.139027255044,
311.137435263095,312.135843271145,313.134251279196,314.132659287247,314.631863291273,
315.131067295298,316.129475303349,317.1278833114,318.126291319451,319.124699327502,
320.123107335553,321.121515343604,321.620719347629,322.119923351655,323.118331359706,
324.116739367757,325.115147375807,326.113555383858,327.111963391909,328.11037139996,
328.609575403986,329.108779408011,330.107187416062,331.105595424113,332.104003432164,
333.102411440215,334.100819448266,335.099227456317,335.598431460342,336.097635464367,
337.096043472418,338.094451480469,339.09285948852,340.091267496571,341.089675504622,
342.088083512673,342.587287516698,343.086491520724,344.084899528775,345.083307536826,
346.081715544877,347.080123552928,348.078531560978,349.076939569029,349.576143573055,
350.07534757708,351.073755585131,352.072163593182,353.070571601233,354.068979609284,
355.067387617335,356.065795625386,356.564999629411,357.064203633437,358.062611641488,
359.061019649539,360.059427657589,361.05783566564,362.056243673691,363.054651681742,
363.553855685768,364.053059689793,365.051467697844,366.049875705895,367.048283713946,
368.046691721997,369.045099730048,370.043507738099,370.542711742124,371.04191574615,
372.040323754201,373.038731762251,374.037139770302,375.035547778353,376.033955786404,
377.032363794455,377.531567798481,378.030771802506,379.029179810557,380.027587818608,
381.025995826659,382.02440383471,383.022811842761,384.021219850812,384.520423854837,
385.019627858862,386.018035866913,387.016443874964,388.014851883015,389.013259891066,
390.011667899117,391.010075907168,391.509279911193,392.008483915219,393.00689192327,
394.005299931321,395.003707939372,396.002115947423,397.000523955473,397.998931963524,
398.49813596755,398.997339971575,399.995747979626,400.994155987677,401.992563995728,
402.990972003779,403.98938001183,404.987788019881,405.486992023906,405.986196027932,
406.984604035983,407.983012044034,408.981420052084,409.979828060135,410.978236068186,
411.976644076237,412.475848080263,412.975052084288,413.973460092339,414.97186810039,
415.970276108441,416.968684116492,417.967092124543,418.965500132594,419.464704136619,
419.963908140644,420.962316148695,421.960724156746,422.959132164797,423.957540172848,
424.955948180899,425.95435618895,426.453560192975,426.952764197001,427.951172205052,
428.949580213103,429.947988221154,430.946396229205,431.944804237256,432.943212245306,
433.442416249332,433.941620253357,434.940028261408,435.938436269459,436.93684427751,
437.935252285561,438.933660293612,439.932068301663,440.431272305688,440.930476309714,
441.928884317765,442.927292325816,443.925700333867,444.924108341917,445.922516349968,
446.920924358019,447.420128362045,447.91933236607,448.917740374121,449.916148382172,
450.914556390223,451.912964398274,452.911372406325,453.909780414376,454.408984418401,
454.908188422427,455.906596430478,456.905004438528,457.903412446579,458.90182045463,
459.900228462681,460.898636470732,461.397840474758,461.897044478783,462.895452486834,
463.893860494885,464.892268502936,465.890676510987,466.889084519038,467.887492527089,
468.386696531114,468.885900535139,469.88430854319,470.882716551241,471.881124559292,
472.879532567343,473.877940575394,474.876348583445,475.37555258747,475.874756591496,
476.873164599547,477.871572607598,478.869980615649,479.8683886237,480.86679663175,
481.865204639801,482.364408643827,482.863612647852,483.862020655903,484.860428663954,
485.858836672005,486.857244680056,487.855652688107,488.854060696158,489.353264700183,
489.852468704209,490.85087671226,491.849284720311,492.847692728361,493.846100736412,
494.844508744463,495.343712748489,495.842949180242),.UNSPECIFIED.);
#96=B_SPLINE_SURFACE_WITH_KNOTS('',3,3,((#69480,#69481,#69482,#69483,#69484,
#69485,#69486,#69487,#69488,#69489,#69490,#69491,#69492,#69493,#69494,#69495,
#69496,#69497,#69498,#69499,#69500,#69501,#69502,#69503,#69504,#69505,#69506,
#69507,#69508,#69509,#69510,#69511,#69512,#69513,#69514,#69515,#69516,#69517,
#69518,#69519,#69520,#69521,#69522,#69523,#69524,#69525,#69526,#69527,#69528,
#69529,#69530,#69531,#69532,#69533,#69534,#69535,#69536,#69537,#69538,#69539,
#69540,#69541,#69542,#69543,#69544,#69545,#69546,#69547,#69548,#69549,#69550,
#69551,#69552,#69553,#69554,#69555,#69556,#69557,#69558,#69559,#69560,#69561,
#69562,#69563,#69564,#69565,#69566,#69567,#69568,#69569,#69570,#69571,#69572,
#69573,#69574,#69575,#69576,#69577,#69578,#69579,#69580,#69581,#69582,#69583,
#69584,#69585,#69586,#69587,#69588,#69589,#69590,#69591,#69592,#69593,#69594,
#69595,#69596,#69597,#69598,#69599,#69600,#69601,#69602,#69603,#69604,#69605,
#69606,#69607,#69608,#69609,#69610,#69611,#69612,#69613,#69614,#69615,#69616,
#69617,#69618,#69619,#69620,#69621,#69622,#69623,#69624,#69625,#69626,#69627,
#69628,#69629,#69630,#69631,#69632,#69633,#69634,#69635,#69636,#69637,#69638,
#69639,#69640,#69641,#69642,#69643,#69644,#69645,#69646,#69647,#69648,#69649,
#69650,#69651,#69652,#69653,#69654,#69655,#69656,#69657,#69658,#69659,#69660,
#69661,#69662,#69663,#69664,#69665,#69666,#69667,#69668,#69669,#69670,#69671,
#69672,#69673,#69674,#69675,#69676,#69677,#69678,#69679,#69680,#69681,#69682,
#69683,#69684,#69685,#69686,#69687,#69688,#69689,#69690,#69691,#69692,#69693,
#69694,#69695,#69696,#69697,#69698,#69699,#69700,#69701,#69702,#69703,#69704,
#69705,#69706,#69707,#69708,#69709,#69710,#69711,#69712,#69713,#69714,#69715,
#69716,#69717,#69718,#69719,#69720,#69721,#69722,#69723,#69724,#69725,#69726,
#69727,#69728,#69729,#69730,#69731,#69732,#69733,#69734,#69735,#69736,#69737,
#69738,#69739,#69740,#69741,#69742,#69743,#69744,#69745,#69746,#69747,#69748,
#69749,#69750,#69751,#69752,#69753,#69754,#69755,#69756,#69757,#69758,#69759,
#69760,#69761,#69762,#69763,#69764,#69765,#69766,#69767,#69768,#69769,#69770,
#69771,#69772,#69773,#69774,#69775,#69776,#69777,#69778,#69779,#69780,#69781,
#69782,#69783,#69784,#69785,#69786,#69787,#69788,#69789,#69790,#69791,#69792,
#69793,#69794,#69795,#69796,#69797,#69798,#69799,#69800,#69801,#69802,#69803,
#69804,#69805,#69806,#69807,#69808,#69809,#69810,#69811,#69812,#69813,#69814,
#69815,#69816,#69817,#69818,#69819,#69820,#69821,#69822,#69823,#69824,#69825,
#69826,#69827,#69828,#69829,#69830,#69831,#69832,#69833,#69834,#69835,#69836,
#69837,#69838,#69839,#69840,#69841,#69842,#69843,#69844,#69845,#69846,#69847,
#69848,#69849,#69850,#69851,#69852,#69853,#69854,#69855,#69856,#69857,#69858,
#69859,#69860,#69861,#69862,#69863,#69864,#69865,#69866,#69867,#69868,#69869,
#69870,#69871,#69872,#69873,#69874,#69875,#69876,#69877,#69878,#69879,#69880,
#69881,#69882,#69883,#69884,#69885,#69886,#69887,#69888,#69889,#69890,#69891,
#69892,#69893,#69894,#69895,#69896,#69897,#69898,#69899,#69900,#69901,#69902,
#69903,#69904,#69905,#69906,#69907,#69908,#69909,#69910,#69911,#69912,#69913,
#69914,#69915,#69916,#69917,#69918,#69919,#69920,#69921,#69922,#69923,#69924,
#69925,#69926,#69927,#69928,#69929,#69930,#69931,#69932,#69933,#69934,#69935,
#69936,#69937,#69938,#69939,#69940,#69941,#69942,#69943,#69944,#69945,#69946,
#69947,#69948,#69949,#69950,#69951,#69952,#69953,#69954,#69955,#69956,#69957,
#69958,#69959,#69960,#69961,#69962,#69963,#69964,#69965,#69966,#69967,#69968,
#69969,#69970,#69971,#69972,#69973,#69974,#69975,#69976,#69977,#69978,#69979,
#69980,#69981,#69982,#69983,#69984,#69985,#69986,#69987,#69988,#69989,#69990,
#69991,#69992,#69993,#69994,#69995,#69996,#69997,#69998,#69999,#70000,#70001,
#70002,#70003,#70004,#70005,#70006,#70007,#70008,#70009,#70010,#70011,#70012,
#70013,#70014,#70015,#70016,#70017,#70018,#70019,#70020,#70021,#70022,#70023,
#70024,#70025,#70026,#70027,#70028,#70029,#70030,#70031,#70032,#70033,#70034,
#70035,#70036,#70037,#70038),(#70039,#70040,#70041,#70042,#70043,#70044,
#70045,#70046,#70047,#70048,#70049,#70050,#70051,#70052,#70053,#70054,#70055,
#70056,#70057,#70058,#70059,#70060,#70061,#70062,#70063,#70064,#70065,#70066,
#70067,#70068,#70069,#70070,#70071,#70072,#70073,#70074,#70075,#70076,#70077,
#70078,#70079,#70080,#70081,#70082,#70083,#70084,#70085,#70086,#70087,#70088,
#70089,#70090,#70091,#70092,#70093,#70094,#70095,#70096,#70097,#70098,#70099,
#70100,#70101,#70102,#70103,#70104,#70105,#70106,#70107,#70108,#70109,#70110,
#70111,#70112,#70113,#70114,#70115,#70116,#70117,#70118,#70119,#70120,#70121,
#70122,#70123,#70124,#70125,#70126,#70127,#70128,#70129,#70130,#70131,#70132,
#70133,#70134,#70135,#70136,#70137,#70138,#70139,#70140,#70141,#70142,#70143,
#70144,#70145,#70146,#70147,#70148,#70149,#70150,#70151,#70152,#70153,#70154,
#70155,#70156,#70157,#70158,#70159,#70160,#70161,#70162,#70163,#70164,#70165,
#70166,#70167,#70168,#70169,#70170,#70171,#70172,#70173,#70174,#70175,#70176,
#70177,#70178,#70179,#70180,#70181,#70182,#70183,#70184,#70185,#70186,#70187,
#70188,#70189,#70190,#70191,#70192,#70193,#70194,#70195,#70196,#70197,#70198,
#70199,#70200,#70201,#70202,#70203,#70204,#70205,#70206,#70207,#70208,#70209,
#70210,#70211,#70212,#70213,#70214,#70215,#70216,#70217,#70218,#70219,#70220,
#70221,#70222,#70223,#70224,#70225,#70226,#70227,#70228,#70229,#70230,#70231,
#70232,#70233,#70234,#70235,#70236,#70237,#70238,#70239,#70240,#70241,#70242,
#70243,#70244,#70245,#70246,#70247,#70248,#70249,#70250,#70251,#70252,#70253,
#70254,#70255,#70256,#70257,#70258,#70259,#70260,#70261,#70262,#70263,#70264,
#70265,#70266,#70267,#70268,#70269,#70270,#70271,#70272,#70273,#70274,#70275,
#70276,#70277,#70278,#70279,#70280,#70281,#70282,#70283,#70284,#70285,#70286,
#70287,#70288,#70289,#70290,#70291,#70292,#70293,#70294,#70295,#70296,#70297,
#70298,#70299,#70300,#70301,#70302,#70303,#70304,#70305,#70306,#70307,#70308,
#70309,#70310,#70311,#70312,#70313,#70314,#70315,#70316,#70317,#70318,#70319,
#70320,#70321,#70322,#70323,#70324,#70325,#70326,#70327,#70328,#70329,#70330,
#70331,#70332,#70333,#70334,#70335,#70336,#70337,#70338,#70339,#70340,#70341,
#70342,#70343,#70344,#70345,#70346,#70347,#70348,#70349,#70350,#70351,#70352,
#70353,#70354,#70355,#70356,#70357,#70358,#70359,#70360,#70361,#70362,#70363,
#70364,#70365,#70366,#70367,#70368,#70369,#70370,#70371,#70372,#70373,#70374,
#70375,#70376,#70377,#70378,#70379,#70380,#70381,#70382,#70383,#70384,#70385,
#70386,#70387,#70388,#70389,#70390,#70391,#70392,#70393,#70394,#70395,#70396,
#70397,#70398,#70399,#70400,#70401,#70402,#70403,#70404,#70405,#70406,#70407,
#70408,#70409,#70410,#70411,#70412,#70413,#70414,#70415,#70416,#70417,#70418,
#70419,#70420,#70421,#70422,#70423,#70424,#70425,#70426,#70427,#70428,#70429,
#70430,#70431,#70432,#70433,#70434,#70435,#70436,#70437,#70438,#70439,#70440,
#70441,#70442,#70443,#70444,#70445,#70446,#70447,#70448,#70449,#70450,#70451,
#70452,#70453,#70454,#70455,#70456,#70457,#70458,#70459,#70460,#70461,#70462,
#70463,#70464,#70465,#70466,#70467,#70468,#70469,#70470,#70471,#70472,#70473,
#70474,#70475,#70476,#70477,#70478,#70479,#70480,#70481,#70482,#70483,#70484,
#70485,#70486,#70487,#70488,#70489,#70490,#70491,#70492,#70493,#70494,#70495,
#70496,#70497,#70498,#70499,#70500,#70501,#70502,#70503,#70504,#70505,#70506,
#70507,#70508,#70509,#70510,#70511,#70512,#70513,#70514,#70515,#70516,#70517,
#70518,#70519,#70520,#70521,#70522,#70523,#70524,#70525,#70526,#70527,#70528,
#70529,#70530,#70531,#70532,#70533,#70534,#70535,#70536,#70537,#70538,#70539,
#70540,#70541,#70542,#70543,#70544,#70545,#70546,#70547,#70548,#70549,#70550,
#70551,#70552,#70553,#70554,#70555,#70556,#70557,#70558,#70559,#70560,#70561,
#70562,#70563,#70564,#70565,#70566,#70567,#70568,#70569,#70570,#70571,#70572,
#70573,#70574,#70575,#70576,#70577,#70578,#70579,#70580,#70581,#70582,#70583,
#70584,#70585,#70586,#70587,#70588,#70589,#70590,#70591,#70592,#70593,#70594,
#70595,#70596,#70597),(#70598,#70599,#70600,#70601,#70602,#70603,#70604,
#70605,#70606,#70607,#70608,#70609,#70610,#70611,#70612,#70613,#70614,#70615,
#70616,#70617,#70618,#70619,#70620,#70621,#70622,#70623,#70624,#70625,#70626,
#70627,#70628,#70629,#70630,#70631,#70632,#70633,#70634,#70635,#70636,#70637,
#70638,#70639,#70640,#70641,#70642,#70643,#70644,#70645,#70646,#70647,#70648,
#70649,#70650,#70651,#70652,#70653,#70654,#70655,#70656,#70657,#70658,#70659,
#70660,#70661,#70662,#70663,#70664,#70665,#70666,#70667,#70668,#70669,#70670,
#70671,#70672,#70673,#70674,#70675,#70676,#70677,#70678,#70679,#70680,#70681,
#70682,#70683,#70684,#70685,#70686,#70687,#70688,#70689,#70690,#70691,#70692,
#70693,#70694,#70695,#70696,#70697,#70698,#70699,#70700,#70701,#70702,#70703,
#70704,#70705,#70706,#70707,#70708,#70709,#70710,#70711,#70712,#70713,#70714,
#70715,#70716,#70717,#70718,#70719,#70720,#70721,#70722,#70723,#70724,#70725,
#70726,#70727,#70728,#70729,#70730,#70731,#70732,#70733,#70734,#70735,#70736,
#70737,#70738,#70739,#70740,#70741,#70742,#70743,#70744,#70745,#70746,#70747,
#70748,#70749,#70750,#70751,#70752,#70753,#70754,#70755,#70756,#70757,#70758,
#70759,#70760,#70761,#70762,#70763,#70764,#70765,#70766,#70767,#70768,#70769,
#70770,#70771,#70772,#70773,#70774,#70775,#70776,#70777,#70778,#70779,#70780,
#70781,#70782,#70783,#70784,#70785,#70786,#70787,#70788,#70789,#70790,#70791,
#70792,#70793,#70794,#70795,#70796,#70797,#70798,#70799,#70800,#70801,#70802,
#70803,#70804,#70805,#70806,#70807,#70808,#70809,#70810,#70811,#70812,#70813,
#70814,#70815,#70816,#70817,#70818,#70819,#70820,#70821,#70822,#70823,#70824,
#70825,#70826,#70827,#70828,#70829,#70830,#70831,#70832,#70833,#70834,#70835,
#70836,#70837,#70838,#70839,#70840,#70841,#70842,#70843,#70844,#70845,#70846,
#70847,#70848,#70849,#70850,#70851,#70852,#70853,#70854,#70855,#70856,#70857,
#70858,#70859,#70860,#70861,#70862,#70863,#70864,#70865,#70866,#70867,#70868,
#70869,#70870,#70871,#70872,#70873,#70874,#70875,#70876,#70877,#70878,#70879,
#70880,#70881,#70882,#70883,#70884,#70885,#70886,#70887,#70888,#70889,#70890,
#70891,#70892,#70893,#70894,#70895,#70896,#70897,#70898,#70899,#70900,#70901,
#70902,#70903,#70904,#70905,#70906,#70907,#70908,#70909,#70910,#70911,#70912,
#70913,#70914,#70915,#70916,#70917,#70918,#70919,#70920,#70921,#70922,#70923,
#70924,#70925,#70926,#70927,#70928,#70929,#70930,#70931,#70932,#70933,#70934,
#70935,#70936,#70937,#70938,#70939,#70940,#70941,#70942,#70943,#70944,#70945,
#70946,#70947,#70948,#70949,#70950,#70951,#70952,#70953,#70954,#70955,#70956,
#70957,#70958,#70959,#70960,#70961,#70962,#70963,#70964,#70965,#70966,#70967,
#70968,#70969,#70970,#70971,#70972,#70973,#70974,#70975,#70976,#70977,#70978,
#70979,#70980,#70981,#70982,#70983,#70984,#70985,#70986,#70987,#70988,#70989,
#70990,#70991,#70992,#70993,#70994,#70995,#70996,#70997,#70998,#70999,#71000,
#71001,#71002,#71003,#71004,#71005,#71006,#71007,#71008,#71009,#71010,#71011,
#71012,#71013,#71014,#71015,#71016,#71017,#71018,#71019,#71020,#71021,#71022,
#71023,#71024,#71025,#71026,#71027,#71028,#71029,#71030,#71031,#71032,#71033,
#71034,#71035,#71036,#71037,#71038,#71039,#71040,#71041,#71042,#71043,#71044,
#71045,#71046,#71047,#71048,#71049,#71050,#71051,#71052,#71053,#71054,#71055,
#71056,#71057,#71058,#71059,#71060,#71061,#71062,#71063,#71064,#71065,#71066,
#71067,#71068,#71069,#71070,#71071,#71072,#71073,#71074,#71075,#71076,#71077,
#71078,#71079,#71080,#71081,#71082,#71083,#71084,#71085,#71086,#71087,#71088,
#71089,#71090,#71091,#71092,#71093,#71094,#71095,#71096,#71097,#71098,#71099,
#71100,#71101,#71102,#71103,#71104,#71105,#71106,#71107,#71108,#71109,#71110,
#71111,#71112,#71113,#71114,#71115,#71116,#71117,#71118,#71119,#71120,#71121,
#71122,#71123,#71124,#71125,#71126,#71127,#71128,#71129,#71130,#71131,#71132,
#71133,#71134,#71135,#71136,#71137,#71138,#71139,#71140,#71141,#71142,#71143,
#71144,#71145,#71146,#71147,#71148,#71149,#71150,#71151,#71152,#71153,#71154,
#71155,#71156),(#71157,#71158,#71159,#71160,#71161,#71162,#71163,#71164,
#71165,#71166,#71167,#71168,#71169,#71170,#71171,#71172,#71173,#71174,#71175,
#71176,#71177,#71178,#71179,#71180,#71181,#71182,#71183,#71184,#71185,#71186,
#71187,#71188,#71189,#71190,#71191,#71192,#71193,#71194,#71195,#71196,#71197,
#71198,#71199,#71200,#71201,#71202,#71203,#71204,#71205,#71206,#71207,#71208,
#71209,#71210,#71211,#71212,#71213,#71214,#71215,#71216,#71217,#71218,#71219,
#71220,#71221,#71222,#71223,#71224,#71225,#71226,#71227,#71228,#71229,#71230,
#71231,#71232,#71233,#71234,#71235,#71236,#71237,#71238,#71239,#71240,#71241,
#71242,#71243,#71244,#71245,#71246,#71247,#71248,#71249,#71250,#71251,#71252,
#71253,#71254,#71255,#71256,#71257,#71258,#71259,#71260,#71261,#71262,#71263,
#71264,#71265,#71266,#71267,#71268,#71269,#71270,#71271,#71272,#71273,#71274,
#71275,#71276,#71277,#71278,#71279,#71280,#71281,#71282,#71283,#71284,#71285,
#71286,#71287,#71288,#71289,#71290,#71291,#71292,#71293,#71294,#71295,#71296,
#71297,#71298,#71299,#71300,#71301,#71302,#71303,#71304,#71305,#71306,#71307,
#71308,#71309,#71310,#71311,#71312,#71313,#71314,#71315,#71316,#71317,#71318,
#71319,#71320,#71321,#71322,#71323,#71324,#71325,#71326,#71327,#71328,#71329,
#71330,#71331,#71332,#71333,#71334,#71335,#71336,#71337,#71338,#71339,#71340,
#71341,#71342,#71343,#71344,#71345,#71346,#71347,#71348,#71349,#71350,#71351,
#71352,#71353,#71354,#71355,#71356,#71357,#71358,#71359,#71360,#71361,#71362,
#71363,#71364,#71365,#71366,#71367,#71368,#71369,#71370,#71371,#71372,#71373,
#71374,#71375,#71376,#71377,#71378,#71379,#71380,#71381,#71382,#71383,#71384,
#71385,#71386,#71387,#71388,#71389,#71390,#71391,#71392,#71393,#71394,#71395,
#71396,#71397,#71398,#71399,#71400,#71401,#71402,#71403,#71404,#71405,#71406,
#71407,#71408,#71409,#71410,#71411,#71412,#71413,#71414,#71415,#71416,#71417,
#71418,#71419,#71420,#71421,#71422,#71423,#71424,#71425,#71426,#71427,#71428,
#71429,#71430,#71431,#71432,#71433,#71434,#71435,#71436,#71437,#71438,#71439,
#71440,#71441,#71442,#71443,#71444,#71445,#71446,#71447,#71448,#71449,#71450,
#71451,#71452,#71453,#71454,#71455,#71456,#71457,#71458,#71459,#71460,#71461,
#71462,#71463,#71464,#71465,#71466,#71467,#71468,#71469,#71470,#71471,#71472,
#71473,#71474,#71475,#71476,#71477,#71478,#71479,#71480,#71481,#71482,#71483,
#71484,#71485,#71486,#71487,#71488,#71489,#71490,#71491,#71492,#71493,#71494,
#71495,#71496,#71497,#71498,#71499,#71500,#71501,#71502,#71503,#71504,#71505,
#71506,#71507,#71508,#71509,#71510,#71511,#71512,#71513,#71514,#71515,#71516,
#71517,#71518,#71519,#71520,#71521,#71522,#71523,#71524,#71525,#71526,#71527,
#71528,#71529,#71530,#71531,#71532,#71533,#71534,#71535,#71536,#71537,#71538,
#71539,#71540,#71541,#71542,#71543,#71544,#71545,#71546,#71547,#71548,#71549,
#71550,#71551,#71552,#71553,#71554,#71555,#71556,#71557,#71558,#71559,#71560,
#71561,#71562,#71563,#71564,#71565,#71566,#71567,#71568,#71569,#71570,#71571,
#71572,#71573,#71574,#71575,#71576,#71577,#71578,#71579,#71580,#71581,#71582,
#71583,#71584,#71585,#71586,#71587,#71588,#71589,#71590,#71591,#71592,#71593,
#71594,#71595,#71596,#71597,#71598,#71599,#71600,#71601,#71602,#71603,#71604,
#71605,#71606,#71607,#71608,#71609,#71610,#71611,#71612,#71613,#71614,#71615,
#71616,#71617,#71618,#71619,#71620,#71621,#71622,#71623,#71624,#71625,#71626,
#71627,#71628,#71629,#71630,#71631,#71632,#71633,#71634,#71635,#71636,#71637,
#71638,#71639,#71640,#71641,#71642,#71643,#71644,#71645,#71646,#71647,#71648,
#71649,#71650,#71651,#71652,#71653,#71654,#71655,#71656,#71657,#71658,#71659,
#71660,#71661,#71662,#71663,#71664,#71665,#71666,#71667,#71668,#71669,#71670,
#71671,#71672,#71673,#71674,#71675,#71676,#71677,#71678,#71679,#71680,#71681,
#71682,#71683,#71684,#71685,#71686,#71687,#71688,#71689,#71690,#71691,#71692,
#71693,#71694,#71695,#71696,#71697,#71698,#71699,#71700,#71701,#71702,#71703,
#71704,#71705,#71706,#71707,#71708,#71709,#71710,#71711,#71712,#71713,#71714,
#71715)),.UNSPECIFIED.,.F.,.F.,.F.,(4,4),(4,1,1,1,1,1,1,1,1,1,1,1,1,1,1,
1,1,1,1,1,1,1,1,1,1,1,1,1,1,1,1,1,1,1,1,1,1,1,1,1,1,1,1,1,1,1,1,1,1,1,1,
1,1,1,1,1,1,1,1,1,1,1,1,1,1,1,1,1,1,1,1,1,1,1,1,1,1,1,1,1,1,1,1,1,1,1,1,
1,1,1,1,1,1,1,1,1,1,1,1,1,1,1,1,1,1,1,1,1,1,1,1,1,1,1,1,1,1,1,1,1,1,1,1,
1,1,1,1,1,1,1,1,1,1,1,1,1,1,1,1,1,1,1,1,1,1,1,1,1,1,1,1,1,1,1,1,1,1,1,1,
1,1,1,1,1,1,1,1,1,1,1,1,1,1,1,1,1,1,1,1,1,1,1,1,1,1,1,1,1,1,1,1,1,1,1,1,
1,1,1,1,1,1,1,1,1,1,1,1,1,1,1,1,1,1,1,1,1,1,1,1,1,1,1,1,1,1,1,1,1,1,1,1,
1,1,1,1,1,1,1,1,1,1,1,1,1,1,1,1,1,1,1,1,1,1,1,1,1,1,1,1,1,1,1,1,1,1,1,1,
1,1,1,1,1,1,1,1,1,1,1,1,1,1,1,1,1,1,1,1,1,1,1,1,1,1,1,1,1,1,1,1,1,1,1,1,
1,1,1,1,1,1,1,1,1,1,1,1,1,1,1,1,1,1,1,1,1,1,1,1,1,1,1,1,1,1,1,1,1,1,1,1,
1,1,1,1,1,1,1,1,1,1,1,1,1,1,1,1,1,1,1,1,1,1,1,1,1,1,1,1,1,1,1,1,1,1,1,1,
1,1,1,1,1,1,1,1,1,1,1,1,1,1,1,1,1,1,1,1,1,1,1,1,1,1,1,1,1,1,1,1,1,1,1,1,
1,1,1,1,1,1,1,1,1,1,1,1,1,1,1,1,1,1,1,1,1,1,1,1,1,1,1,1,1,1,1,1,1,1,1,1,
1,1,1,1,1,1,1,1,1,1,1,1,1,1,1,1,1,1,1,1,1,1,1,1,1,1,1,1,1,1,1,1,1,1,1,1,
1,1,1,1,1,1,1,1,1,1,1,1,1,1,1,1,1,1,1,1,1,1,1,1,1,1,1,1,1,1,1,1,1,1,1,1,
1,1,1,1,1,1,1,1,1,1,1,1,1,1,1,1,1,1,1,1,1,1,1,1,1,1,1,1,1,1,1,1,1,1,1,1,
1,4),(-0.00081013426626431,0.132758442671244),(8.30110427451238,8.80100606031193,
9.30088286599662,10.300636477366,11.3003900887353,12.3001437001047,13.2998973114741,
14.2996509228435,14.7995277285281,15.2994045342128,16.2991581455822,17.2989117569516,
18.2986653683209,19.2984189796903,20.2981725910597,21.297926202429,21.7978030081137,
22.2976798137984,23.2974334251678,24.2971870365371,25.2969406479065,26.2966942592759,
27.2964478706452,28.2962014820146,28.7960782876993,29.295955093384,30.2957087047533,
31.2954623161227,32.2952159274921,33.2949695388614,34.2947231502308,35.2944767616002,
35.7943535672848,36.2942303729695,37.2939839843389,38.2937375957083,39.2934912070776,
40.293244818447,41.2929984298164,42.2927520411857,42.7926288468704,43.2925056525551,
44.2922592639245,45.2920128752938,46.2917664866632,47.2915200980326,48.2912737094019,
49.2910273207713,49.790904126456,50.2907809321407,51.29053454351,52.2902881548794,
53.2900417662488,54.2897953776181,55.2895489889875,56.2893026003569,56.7891794060416,
57.2890562117262,58.2888098230956,59.288563434465,60.2883170458343,61.2880706572037,
62.2878242685731,63.2875778799424,63.7874546856271,64.2873314913118,65.2870851026812,
66.2868387140505,67.2865923254199,68.2863459367893,69.2860995481586,70.285853159528,
70.7857299652127,71.2856067708974,72.2853603822667,73.2851139936361,74.2848676050055,
75.2846212163748,76.2843748277442,77.2841284391136,77.7840052447983,78.2838820504829,
79.2836356618523,80.2833892732217,81.283142884591,82.2828964959604,83.2826501073298,
84.2824037186991,84.7822805243838,85.2821573300685,86.2819109414379,87.2816645528073,
88.2814181641766,89.281171775546,90.2809253869154,91.2806789982847,91.7805558039694,
92.2804326096541,93.2801862210235,94.2799398323928,95.2796934437622,96.2794470551316,
97.2792006665009,98.2789542778703,98.778831083555,99.2787078892397,100.278461500609,
101.278215111978,102.277968723348,103.277722334717,104.277475946086,105.277229557456,
105.777106363141,106.276983168825,107.276736780195,108.276490391564,109.276244002933,
110.275997614303,111.275751225672,112.275504837041,112.775381642726,113.275258448411,
114.27501205978,115.27476567115,116.274519282519,117.274272893888,118.274026505258,
119.273780116627,119.773656922312,120.273533727996,121.273287339366,122.273040950735,
123.272794562104,124.272548173474,125.272301784843,126.272055396213,126.771932201897,
127.271809007582,128.271562618951,129.271316230321,130.27106984169,131.270823453059,
132.270577064429,133.270330675798,133.770207481483,134.270084287167,135.269837898537,
136.269591509906,137.269345121276,138.269098732645,139.268852344014,140.268605955384,
140.768482761068,141.268359566753,142.268113178122,143.267866789492,144.267620400861,
145.267374012231,146.2671276236,147.266881234969,147.766758040654,148.266634846339,
149.266388457708,150.266142069077,151.265895680447,152.265649291816,153.265402903185,
154.265156514555,154.76503332024,155.264910125924,156.264663737294,157.264417348663,
158.264170960032,159.263924571402,160.263678182771,161.26343179414,161.763308599825,
162.26318540551,163.262939016879,164.262692628249,165.262446239618,166.262199850987,
167.261953462357,168.261707073726,168.761583879411,169.261460685095,170.261214296465,
171.260967907834,172.260721519203,173.260475130573,174.260228741942,175.259982353312,
175.759859158996,176.259735964681,177.25948957605,178.25924318742,179.258996798789,
180.258750410158,181.258504021528,182.258257632897,182.758134438582,183.258011244266,
184.257764855636,185.257518467005,186.257272078375,187.257025689744,188.256779301113,
189.256532912483,189.756409718167,190.256286523852,191.256040135221,192.255793746591,
193.25554735796,194.25530096933,195.255054580699,196.254808192068,196.754684997753,
197.254561803438,198.254315414807,199.254069026176,200.253822637546,201.253576248915,
202.253329860284,203.253083471654,203.752960277339,204.252837083023,205.252590694393,
206.252344305762,207.252097917131,208.251851528501,209.25160513987,210.251358751239,
210.751235556924,211.251112362609,212.250865973978,213.250619585347,214.250373196717,
215.250126808086,216.249880419456,217.249634030825,217.74951083651,218.249387642194,
219.249141253564,220.248894864933,221.248648476302,222.248402087672,223.248155699041,
224.247909310411,224.747786116095,225.24766292178,226.247416533149,227.247170144519,
228.246923755888,229.246677367257,230.246430978627,231.246184589996,231.746061395681,
232.245938201365,233.245691812735,234.245445424104,235.245199035474,236.244952646843,
237.244706258212,238.244459869582,238.744336675266,239.244213480951,240.24396709232,
241.24372070369,242.243474315059,243.243227926429,244.242981537798,245.242735149167,
245.742611954852,246.242488760537,247.242242371906,248.241995983275,249.241749594645,
250.241503206014,251.241256817383,252.241010428753,253.240764040122,254.240517651492,
255.240271262861,256.24002487423,256.739901679915,257.2397784856,258.239532096969,
259.239285708338,260.239039319708,261.238792931077,262.238546542446,263.238300153816,
263.7381769595,264.238053765185,265.237807376555,266.237560987924,267.237314599293,
268.237068210663,269.236821822032,270.236575433401,270.736452239086,271.236329044771,
272.23608265614,273.23583626751,274.235589878879,275.235343490248,276.235097101618,
277.234850712987,277.734727518672,278.234604324356,279.234357935726,280.234111547095,
281.233865158464,282.233618769834,283.233372381203,284.233125992573,284.733002798257,
285.232879603942,286.232633215311,287.232386826681,288.23214043805,289.231894049419,
290.231647660789,291.231401272158,291.731278077843,292.231154883527,293.230908494897,
294.230662106266,295.230415717636,296.230169329005,297.229922940374,298.229676551744,
298.729553357428,299.229430163113,300.229183774482,301.228937385852,302.228690997221,
303.228444608591,304.22819821996,305.227951831329,305.727828637014,306.227705442699,
307.227459054068,308.227212665437,309.226966276807,310.226719888176,311.226473499545,
312.226227110915,312.7261039166,313.225980722284,314.225734333654,315.225487945023,
316.225241556392,317.224995167762,318.224748779131,319.2245023905,319.724379196185,
320.22425600187,321.224009613239,322.223763224608,323.223516835978,324.223270447347,
325.223024058717,326.222777670086,326.722654475771,327.222531281455,328.222284892825,
329.222038504194,330.221792115563,331.221545726933,332.221299338302,333.221052949672,
333.720929755356,334.220806561041,335.22056017241,336.22031378378,337.220067395149,
338.219821006518,339.219574617888,340.219328229257,340.719205034942,341.219081840626,
342.218835451996,343.218589063365,344.218342674735,345.218096286104,346.217849897473,
347.217603508843,347.717480314527,348.217357120212,349.217110731581,350.216864342951,
351.21661795432,352.216371565689,353.216125177059,354.215878788428,354.715755594113,
355.215632399798,356.215386011167,357.215139622536,358.214893233906,359.214646845275,
360.214400456644,361.214154068014,361.714030873699,362.213907679383,363.213661290753,
364.213414902122,365.213168513491,366.212922124861,367.21267573623,368.212429347599,
368.712306153284,369.212182958969,370.211936570338,371.211690181707,372.211443793077,
373.211197404446,374.210951015816,375.210704627185,375.71058143287,376.210458238554,
377.210211849924,378.209965461293,379.209719072662,380.209472684032,381.209226295401,
382.208979906771,382.708856712455,383.20873351814,384.208487129509,385.208240740879,
386.207994352248,387.207747963617,388.207501574987,389.207255186356,389.707131992041,
390.207008797725,391.206762409095,392.206516020464,393.206269631834,394.206023243203,
395.205776854572,396.205530465942,396.705407271626,397.205284077311,398.20503768868,
399.20479130005,400.204544911419,401.204298522789,402.204052134158,403.203805745527,
403.703682551212,404.203559356897,405.203312968266,406.203066579635,407.202820191005,
408.202573802374,409.202327413743,410.202081025113,410.701957830797,411.201834636482,
412.201588247852,413.201341859221,414.20109547059,415.20084908196,416.200602693329,
417.200356304698,417.700233110383,418.200109916068,419.199863527437,420.199617138806,
421.199370750176,422.199124361545,423.198877972915,424.198631584284,424.698508389969,
425.198385195653,426.198138807023,427.197892418392,428.197646029761,429.197399641131,
430.1971532525,431.19690686387,431.696783669554,432.196660475239,433.196414086608,
434.196167697978,435.195921309347,436.195674920716,437.195428532086,438.195182143455,
438.69505894914,439.194935754824,440.194689366194,441.194442977563,442.194196588933,
443.193950200302,444.193703811671,445.193457423041,445.693334228725,446.19321103441,
447.192964645779,448.192718257149,449.192471868518,450.192225479887,451.191979091257,
452.191732702626,452.691609508311,453.191486313996,454.191239925365,455.190993536734,
456.190747148104,457.190500759473,458.190254370842,459.190007982212,459.689884787896,
460.189761593581,461.189515204951,462.18926881632,463.189022427689,464.188776039059,
465.188529650428,466.188283261797,466.688160067482,467.188036873167,468.187790484536,
469.187544095905,470.187297707275,471.187051318644,472.186804930014,473.186558541383,
473.686435347068,474.186312152752,475.186065764122,476.185819375491,477.18557298686,
478.18532659823,479.185080209599,480.184833820968,480.684710626653,481.184587432338,
482.184341043707,483.184094655077,484.183848266446,485.183601877815,486.183355489185,
487.183109100554,487.682985906239,488.182862711923,489.182616323293,490.182369934662,
491.182123546032,492.181877157401,493.18163076877,493.681507574455,494.18151432674),
 .UNSPECIFIED.);
#97=B_SPLINE_SURFACE_WITH_KNOTS('',3,3,((#78284,#78285,#78286,#78287,#78288,
#78289,#78290,#78291,#78292,#78293,#78294,#78295,#78296,#78297,#78298,#78299,
#78300,#78301,#78302,#78303,#78304,#78305,#78306,#78307,#78308,#78309,#78310,
#78311,#78312,#78313,#78314,#78315,#78316,#78317,#78318,#78319,#78320,#78321,
#78322,#78323,#78324,#78325,#78326,#78327,#78328,#78329,#78330,#78331,#78332,
#78333,#78334,#78335,#78336,#78337,#78338,#78339,#78340,#78341,#78342,#78343,
#78344,#78345,#78346,#78347,#78348,#78349,#78350,#78351,#78352,#78353,#78354,
#78355,#78356,#78357,#78358,#78359,#78360,#78361,#78362,#78363,#78364,#78365,
#78366,#78367,#78368,#78369,#78370,#78371,#78372,#78373,#78374,#78375,#78376,
#78377,#78378,#78379,#78380,#78381,#78382,#78383,#78384,#78385,#78386,#78387,
#78388,#78389,#78390,#78391,#78392,#78393,#78394,#78395,#78396,#78397,#78398,
#78399,#78400,#78401,#78402,#78403,#78404,#78405,#78406,#78407,#78408,#78409,
#78410,#78411,#78412,#78413,#78414,#78415,#78416),(#78417,#78418,#78419,
#78420,#78421,#78422,#78423,#78424,#78425,#78426,#78427,#78428,#78429,#78430,
#78431,#78432,#78433,#78434,#78435,#78436,#78437,#78438,#78439,#78440,#78441,
#78442,#78443,#78444,#78445,#78446,#78447,#78448,#78449,#78450,#78451,#78452,
#78453,#78454,#78455,#78456,#78457,#78458,#78459,#78460,#78461,#78462,#78463,
#78464,#78465,#78466,#78467,#78468,#78469,#78470,#78471,#78472,#78473,#78474,
#78475,#78476,#78477,#78478,#78479,#78480,#78481,#78482,#78483,#78484,#78485,
#78486,#78487,#78488,#78489,#78490,#78491,#78492,#78493,#78494,#78495,#78496,
#78497,#78498,#78499,#78500,#78501,#78502,#78503,#78504,#78505,#78506,#78507,
#78508,#78509,#78510,#78511,#78512,#78513,#78514,#78515,#78516,#78517,#78518,
#78519,#78520,#78521,#78522,#78523,#78524,#78525,#78526,#78527,#78528,#78529,
#78530,#78531,#78532,#78533,#78534,#78535,#78536,#78537,#78538,#78539,#78540,
#78541,#78542,#78543,#78544,#78545,#78546,#78547,#78548,#78549),(#78550,
#78551,#78552,#78553,#78554,#78555,#78556,#78557,#78558,#78559,#78560,#78561,
#78562,#78563,#78564,#78565,#78566,#78567,#78568,#78569,#78570,#78571,#78572,
#78573,#78574,#78575,#78576,#78577,#78578,#78579,#78580,#78581,#78582,#78583,
#78584,#78585,#78586,#78587,#78588,#78589,#78590,#78591,#78592,#78593,#78594,
#78595,#78596,#78597,#78598,#78599,#78600,#78601,#78602,#78603,#78604,#78605,
#78606,#78607,#78608,#78609,#78610,#78611,#78612,#78613,#78614,#78615,#78616,
#78617,#78618,#78619,#78620,#78621,#78622,#78623,#78624,#78625,#78626,#78627,
#78628,#78629,#78630,#78631,#78632,#78633,#78634,#78635,#78636,#78637,#78638,
#78639,#78640,#78641,#78642,#78643,#78644,#78645,#78646,#78647,#78648,#78649,
#78650,#78651,#78652,#78653,#78654,#78655,#78656,#78657,#78658,#78659,#78660,
#78661,#78662,#78663,#78664,#78665,#78666,#78667,#78668,#78669,#78670,#78671,
#78672,#78673,#78674,#78675,#78676,#78677,#78678,#78679,#78680,#78681,#78682),
(#78683,#78684,#78685,#78686,#78687,#78688,#78689,#78690,#78691,#78692,
#78693,#78694,#78695,#78696,#78697,#78698,#78699,#78700,#78701,#78702,#78703,
#78704,#78705,#78706,#78707,#78708,#78709,#78710,#78711,#78712,#78713,#78714,
#78715,#78716,#78717,#78718,#78719,#78720,#78721,#78722,#78723,#78724,#78725,
#78726,#78727,#78728,#78729,#78730,#78731,#78732,#78733,#78734,#78735,#78736,
#78737,#78738,#78739,#78740,#78741,#78742,#78743,#78744,#78745,#78746,#78747,
#78748,#78749,#78750,#78751,#78752,#78753,#78754,#78755,#78756,#78757,#78758,
#78759,#78760,#78761,#78762,#78763,#78764,#78765,#78766,#78767,#78768,#78769,
#78770,#78771,#78772,#78773,#78774,#78775,#78776,#78777,#78778,#78779,#78780,
#78781,#78782,#78783,#78784,#78785,#78786,#78787,#78788,#78789,#78790,#78791,
#78792,#78793,#78794,#78795,#78796,#78797,#78798,#78799,#78800,#78801,#78802,
#78803,#78804,#78805,#78806,#78807,#78808,#78809,#78810,#78811,#78812,#78813,
#78814,#78815)),.UNSPECIFIED.,.F.,.F.,.F.,(4,4),(4,1,1,1,1,1,1,1,1,1,1,
1,1,1,1,1,1,1,1,1,1,1,1,1,1,1,1,1,1,1,1,1,1,1,1,1,1,1,1,1,1,1,1,1,1,1,1,
1,1,1,1,1,1,1,1,1,1,1,1,1,1,1,1,1,1,1,1,1,1,1,1,1,1,1,1,1,1,1,1,1,1,1,1,
1,1,1,1,1,1,1,1,1,1,1,1,1,1,1,1,1,1,1,1,1,1,1,1,1,1,1,1,1,1,1,1,1,1,1,1,
1,1,1,1,1,1,1,1,1,1,1,4),(-8.529467209505E-5,0.128694174119411),(11.8548225190662,
12.3537726257656,12.8526374377929,13.3515022498203,13.8503670618476,14.3492318738749,
14.8480966859023,15.3469614979296,15.8458263099569,16.3446911219842,16.8435559340116,
17.3424207460389,17.8412855580662,18.3401503700936,18.8390151821209,19.3378799941482,
19.8367448061755,20.3356096182029,20.8344744302302,21.3333392422575,21.8322040542849,
22.3310688663122,22.8299336783395,23.3287984903668,23.8276633023942,24.3265281144215,
24.8253929264488,25.3242577384762,25.8231225505035,26.3219873625308,26.8208521745581,
27.3197169865855,27.8185817986128,28.3174466106401,28.8163114226675,29.3151762346948,
29.8140410467221,30.3129058587495,30.8117706707768,31.3106354828041,31.8095002948314,
32.3083651068588,32.8072299188861,33.3060947309134,33.8049595429408,34.3038243549681,
34.8026891669954,35.3015539790227,35.8004187910501,36.2992836030774,36.7981484151047,
37.2970132271321,37.7958780391594,38.2947428511867,38.793607663214,39.2924724752414,
39.7913372872687,40.290202099296,40.7890669113234,41.2879317233507,41.786796535378,
42.2856613474054,42.7845261594327,43.28339097146,43.7822557834873,44.2811205955147,
44.779985407542,45.2788502195693,45.7777150315967,46.276579843624,46.7754446556513,
47.2743094676786,47.773174279706,48.2720390917333,48.7709039037606,49.269768715788,
49.7686335278153,50.2674983398426,50.76636315187,51.2652279638973,51.7640927759246,
52.2629575879519,52.7618223999793,53.2606872120066,53.7595520240339,54.2584168360613,
54.7572816480886,55.2561464601159,55.7550112721432,56.2538760841706,56.7527408961979,
57.2516057082252,57.7504705202526,58.2493353322799,58.7482001443072,59.2470649563345,
59.7459297683619,60.2447945803892,60.7436593924165,61.2425242044439,61.7413890164712,
62.2402538284985,62.7391186405258,63.2379834525532,63.7368482645805,64.2357130766078,
64.7345778886352,65.2334427006625,65.7323075126898,66.2311723247172,66.7300371367445,
67.2289019487718,67.7277667607991,68.2266315728265,68.7254963848538,69.2243611968811,
69.7232260089085,70.2220908209358,70.7209556329631,71.2198204449904,71.7186852570178,
72.2175500690451,72.7164148810724,73.2152796930998,73.7141445051271,74.2130093171544,
74.7118741291818,75.2107389412091,75.7096037532364,76.2084685652637,76.7073333772911),
 .UNSPECIFIED.);
#98=B_SPLINE_SURFACE_WITH_KNOTS('',3,3,((#79039,#79040,#79041,#79042,#79043,
#79044,#79045,#79046,#79047,#79048,#79049,#79050,#79051,#79052,#79053,#79054,
#79055,#79056,#79057,#79058,#79059,#79060,#79061,#79062,#79063,#79064,#79065,
#79066,#79067,#79068,#79069,#79070,#79071,#79072,#79073,#79074,#79075,#79076,
#79077,#79078,#79079,#79080,#79081,#79082,#79083,#79084,#79085,#79086,#79087,
#79088,#79089,#79090,#79091,#79092,#79093,#79094,#79095,#79096,#79097,#79098,
#79099,#79100,#79101,#79102,#79103,#79104,#79105,#79106,#79107,#79108,#79109,
#79110,#79111,#79112,#79113,#79114,#79115,#79116,#79117,#79118,#79119,#79120,
#79121,#79122,#79123,#79124,#79125,#79126,#79127,#79128,#79129,#79130,#79131,
#79132,#79133,#79134,#79135,#79136,#79137,#79138,#79139,#79140,#79141,#79142,
#79143,#79144,#79145,#79146,#79147,#79148,#79149,#79150,#79151,#79152,#79153,
#79154,#79155,#79156,#79157,#79158,#79159,#79160,#79161,#79162,#79163,#79164,
#79165,#79166,#79167,#79168,#79169,#79170,#79171),(#79172,#79173,#79174,
#79175,#79176,#79177,#79178,#79179,#79180,#79181,#79182,#79183,#79184,#79185,
#79186,#79187,#79188,#79189,#79190,#79191,#79192,#79193,#79194,#79195,#79196,
#79197,#79198,#79199,#79200,#79201,#79202,#79203,#79204,#79205,#79206,#79207,
#79208,#79209,#79210,#79211,#79212,#79213,#79214,#79215,#79216,#79217,#79218,
#79219,#79220,#79221,#79222,#79223,#79224,#79225,#79226,#79227,#79228,#79229,
#79230,#79231,#79232,#79233,#79234,#79235,#79236,#79237,#79238,#79239,#79240,
#79241,#79242,#79243,#79244,#79245,#79246,#79247,#79248,#79249,#79250,#79251,
#79252,#79253,#79254,#79255,#79256,#79257,#79258,#79259,#79260,#79261,#79262,
#79263,#79264,#79265,#79266,#79267,#79268,#79269,#79270,#79271,#79272,#79273,
#79274,#79275,#79276,#79277,#79278,#79279,#79280,#79281,#79282,#79283,#79284,
#79285,#79286,#79287,#79288,#79289,#79290,#79291,#79292,#79293,#79294,#79295,
#79296,#79297,#79298,#79299,#79300,#79301,#79302,#79303,#79304),(#79305,
#79306,#79307,#79308,#79309,#79310,#79311,#79312,#79313,#79314,#79315,#79316,
#79317,#79318,#79319,#79320,#79321,#79322,#79323,#79324,#79325,#79326,#79327,
#79328,#79329,#79330,#79331,#79332,#79333,#79334,#79335,#79336,#79337,#79338,
#79339,#79340,#79341,#79342,#79343,#79344,#79345,#79346,#79347,#79348,#79349,
#79350,#79351,#79352,#79353,#79354,#79355,#79356,#79357,#79358,#79359,#79360,
#79361,#79362,#79363,#79364,#79365,#79366,#79367,#79368,#79369,#79370,#79371,
#79372,#79373,#79374,#79375,#79376,#79377,#79378,#79379,#79380,#79381,#79382,
#79383,#79384,#79385,#79386,#79387,#79388,#79389,#79390,#79391,#79392,#79393,
#79394,#79395,#79396,#79397,#79398,#79399,#79400,#79401,#79402,#79403,#79404,
#79405,#79406,#79407,#79408,#79409,#79410,#79411,#79412,#79413,#79414,#79415,
#79416,#79417,#79418,#79419,#79420,#79421,#79422,#79423,#79424,#79425,#79426,
#79427,#79428,#79429,#79430,#79431,#79432,#79433,#79434,#79435,#79436,#79437),
(#79438,#79439,#79440,#79441,#79442,#79443,#79444,#79445,#79446,#79447,
#79448,#79449,#79450,#79451,#79452,#79453,#79454,#79455,#79456,#79457,#79458,
#79459,#79460,#79461,#79462,#79463,#79464,#79465,#79466,#79467,#79468,#79469,
#79470,#79471,#79472,#79473,#79474,#79475,#79476,#79477,#79478,#79479,#79480,
#79481,#79482,#79483,#79484,#79485,#79486,#79487,#79488,#79489,#79490,#79491,
#79492,#79493,#79494,#79495,#79496,#79497,#79498,#79499,#79500,#79501,#79502,
#79503,#79504,#79505,#79506,#79507,#79508,#79509,#79510,#79511,#79512,#79513,
#79514,#79515,#79516,#79517,#79518,#79519,#79520,#79521,#79522,#79523,#79524,
#79525,#79526,#79527,#79528,#79529,#79530,#79531,#79532,#79533,#79534,#79535,
#79536,#79537,#79538,#79539,#79540,#79541,#79542,#79543,#79544,#79545,#79546,
#79547,#79548,#79549,#79550,#79551,#79552,#79553,#79554,#79555,#79556,#79557,
#79558,#79559,#79560,#79561,#79562,#79563,#79564,#79565,#79566,#79567,#79568,
#79569,#79570)),.UNSPECIFIED.,.F.,.F.,.F.,(4,4),(4,1,1,1,1,1,1,1,1,1,1,
1,1,1,1,1,1,1,1,1,1,1,1,1,1,1,1,1,1,1,1,1,1,1,1,1,1,1,1,1,1,1,1,1,1,1,1,
1,1,1,1,1,1,1,1,1,1,1,1,1,1,1,1,1,1,1,1,1,1,1,1,1,1,1,1,1,1,1,1,1,1,1,1,
1,1,1,1,1,1,1,1,1,1,1,1,1,1,1,1,1,1,1,1,1,1,1,1,1,1,1,1,1,1,1,1,1,1,1,1,
1,1,1,1,1,1,1,1,1,1,1,4),(-6.05230187934505E-5,0.12871890615391),(14.3988535768129,
14.8977183888402,15.3965832008676,15.8954480128949,16.3943128249222,16.8931776369496,
17.3920424489769,17.8909072610042,18.3897720730315,18.8886368850589,19.3875016970862,
19.8863665091135,20.3852313211409,20.8840961331682,21.3829609451955,21.8818257572228,
22.3806905692502,22.8795553812775,23.3784201933048,23.8772850053322,24.3761498173595,
24.8750146293868,25.3738794414141,25.8727442534415,26.3716090654688,26.8704738774961,
27.3693386895235,27.8682035015508,28.3670683135781,28.8659331256054,29.3647979376328,
29.8636627496601,30.3625275616874,30.8613923737148,31.3602571857421,31.8591219977694,
32.3579868097967,32.8568516218241,33.3557164338514,33.8545812458787,34.3534460579061,
34.8523108699334,35.3511756819607,35.8500404939881,36.3489053060154,36.8477701180427,
37.34663493007,37.8454997420974,38.3443645541247,38.843229366152,39.3420941781794,
39.8409589902067,40.339823802234,40.8386886142613,41.3375534262887,41.836418238316,
42.3352830503433,42.8341478623707,43.333012674398,43.8318774864253,44.3307422984526,
44.82960711048,45.3284719225073,45.8273367345346,46.326201546562,46.8250663585893,
47.3239311706166,47.8227959826439,48.3216607946713,48.8205256066986,49.3193904187259,
49.8182552307533,50.3171200427806,50.8159848548079,51.3148496668353,51.8137144788626,
52.3125792908899,52.8114441029172,53.3103089149446,53.8091737269719,54.3080385389992,
54.8069033510266,55.3057681630539,55.8046329750812,56.3034977871085,56.8023625991359,
57.3012274111632,57.8000922231905,58.2989570352179,58.7978218472452,59.2966866592725,
59.7955514712998,60.2944162833272,60.7932810953545,61.2921459073818,61.7910107194092,
62.2898755314365,62.7887403434638,63.2876051554911,63.7864699675185,64.2853347795458,
64.7841995915731,65.2830644036005,65.7819292156278,66.2807940276551,66.7796588396825,
67.2785236517098,67.7773884637371,68.2762532757644,68.7751180877918,69.2739828998191,
69.7728477118464,70.2717125238738,70.7705773359011,71.2694421479284,71.7683069599557,
72.2671717719831,72.7660365840104,73.2649013960377,73.7637662080651,74.2626310200924,
74.7614958321197,75.260360644147,75.7592254561744,76.2580902682017,76.756955080229,
77.2558198922564,77.7546847042837,78.253549516311,78.7524143283383,79.2513644065442),
 .UNSPECIFIED.);
#99=B_SPLINE_SURFACE_WITH_KNOTS('',3,3,((#87313,#87314,#87315,#87316,#87317,
#87318,#87319,#87320,#87321,#87322,#87323,#87324,#87325,#87326,#87327,#87328,
#87329,#87330,#87331,#87332,#87333,#87334,#87335,#87336,#87337,#87338,#87339,
#87340,#87341,#87342,#87343,#87344,#87345,#87346,#87347,#87348,#87349,#87350,
#87351,#87352,#87353,#87354,#87355),(#87356,#87357,#87358,#87359,#87360,
#87361,#87362,#87363,#87364,#87365,#87366,#87367,#87368,#87369,#87370,#87371,
#87372,#87373,#87374,#87375,#87376,#87377,#87378,#87379,#87380,#87381,#87382,
#87383,#87384,#87385,#87386,#87387,#87388,#87389,#87390,#87391,#87392,#87393,
#87394,#87395,#87396,#87397,#87398),(#87399,#87400,#87401,#87402,#87403,
#87404,#87405,#87406,#87407,#87408,#87409,#87410,#87411,#87412,#87413,#87414,
#87415,#87416,#87417,#87418,#87419,#87420,#87421,#87422,#87423,#87424,#87425,
#87426,#87427,#87428,#87429,#87430,#87431,#87432,#87433,#87434,#87435,#87436,
#87437,#87438,#87439,#87440,#87441),(#87442,#87443,#87444,#87445,#87446,
#87447,#87448,#87449,#87450,#87451,#87452,#87453,#87454,#87455,#87456,#87457,
#87458,#87459,#87460,#87461,#87462,#87463,#87464,#87465,#87466,#87467,#87468,
#87469,#87470,#87471,#87472,#87473,#87474,#87475,#87476,#87477,#87478,#87479,
#87480,#87481,#87482,#87483,#87484)),.UNSPECIFIED.,.F.,.F.,.F.,(4,4),(4,
1,1,1,1,1,1,1,1,1,1,1,1,1,1,1,1,1,1,1,1,1,1,1,1,1,1,1,1,1,1,1,1,1,1,1,1,
1,1,1,4),(-0.00051259176634298,0.0646339630657592),(11.8584762705415,12.8518902807105,
13.8447916991131,14.8376931175158,15.8305945359184,16.8234959543211,17.8163973727237,
18.8092987911264,19.802200209529,20.7951016279317,21.7880030463343,22.780904464737,
23.7738058831396,24.7667073015423,25.7596087199449,26.7525101383476,27.7454115567502,
28.7383129751529,29.7312143935555,30.7241158119582,31.7170172303608,32.7099186487635,
33.7028200671661,34.6957214855688,35.6886229039714,36.6815243223741,37.6744257407767,
38.6673271591794,39.660228577582,40.6531299959847,41.6460314143873,42.63893283279,
43.6318342511926,44.6247356695953,45.6176370879979,46.6105385064006,47.6034399248032,
48.5963413432059,49.5892427616085,50.5821441800112,51.5750455984138),
 .UNSPECIFIED.);
#100=B_SPLINE_SURFACE_WITH_KNOTS('',3,3,((#87669,#87670,#87671,#87672,#87673,
#87674,#87675,#87676,#87677,#87678,#87679,#87680,#87681,#87682,#87683,#87684,
#87685,#87686,#87687,#87688,#87689,#87690,#87691,#87692,#87693,#87694,#87695,
#87696,#87697,#87698,#87699,#87700,#87701,#87702,#87703,#87704,#87705,#87706,
#87707,#87708,#87709,#87710,#87711),(#87712,#87713,#87714,#87715,#87716,
#87717,#87718,#87719,#87720,#87721,#87722,#87723,#87724,#87725,#87726,#87727,
#87728,#87729,#87730,#87731,#87732,#87733,#87734,#87735,#87736,#87737,#87738,
#87739,#87740,#87741,#87742,#87743,#87744,#87745,#87746,#87747,#87748,#87749,
#87750,#87751,#87752,#87753,#87754),(#87755,#87756,#87757,#87758,#87759,
#87760,#87761,#87762,#87763,#87764,#87765,#87766,#87767,#87768,#87769,#87770,
#87771,#87772,#87773,#87774,#87775,#87776,#87777,#87778,#87779,#87780,#87781,
#87782,#87783,#87784,#87785,#87786,#87787,#87788,#87789,#87790,#87791,#87792,
#87793,#87794,#87795,#87796,#87797),(#87798,#87799,#87800,#87801,#87802,
#87803,#87804,#87805,#87806,#87807,#87808,#87809,#87810,#87811,#87812,#87813,
#87814,#87815,#87816,#87817,#87818,#87819,#87820,#87821,#87822,#87823,#87824,
#87825,#87826,#87827,#87828,#87829,#87830,#87831,#87832,#87833,#87834,#87835,
#87836,#87837,#87838,#87839,#87840)),.UNSPECIFIED.,.F.,.F.,.F.,(4,4),(4,
1,1,1,1,1,1,1,1,1,1,1,1,1,1,1,1,1,1,1,1,1,1,1,1,1,1,1,1,1,1,1,1,1,1,1,1,
1,1,1,4),(-0.000452026491598011,0.0646067404509306),(14.3984001269719,15.3913015453745,
16.3842029637772,17.3771043821798,18.3700058005825,19.3629072189851,20.3558086373878,
21.3487100557904,22.3416114741931,23.3345128925957,24.3274143109984,25.320315729401,
26.3132171478037,27.3061185662063,28.299019984609,29.2919214030116,30.2848228214142,
31.2777242398169,32.2706256582195,33.2635270766222,34.2564284950248,35.2493299134275,
36.2422313318301,37.2351327502328,38.2280341686354,39.2209355870381,40.2138370054407,
41.2067384238434,42.199639842246,43.1925412606487,44.1854426790513,45.178344097454,
46.1712455158566,47.1641469342593,48.1570483526619,49.1499497710646,50.1428511894672,
51.1357526078699,52.1286540262725,53.1215554446752,54.1144568630778),
 .UNSPECIFIED.);
#101=B_SPLINE_SURFACE_WITH_KNOTS('',3,3,((#88213,#88214,#88215,#88216,#88217,
#88218,#88219,#88220,#88221,#88222,#88223,#88224,#88225,#88226,#88227,#88228,
#88229,#88230,#88231,#88232,#88233,#88234,#88235,#88236,#88237,#88238,#88239,
#88240,#88241,#88242,#88243,#88244,#88245,#88246,#88247,#88248,#88249,#88250,
#88251,#88252,#88253,#88254,#88255),(#88256,#88257,#88258,#88259,#88260,
#88261,#88262,#88263,#88264,#88265,#88266,#88267,#88268,#88269,#88270,#88271,
#88272,#88273,#88274,#88275,#88276,#88277,#88278,#88279,#88280,#88281,#88282,
#88283,#88284,#88285,#88286,#88287,#88288,#88289,#88290,#88291,#88292,#88293,
#88294,#88295,#88296,#88297,#88298),(#88299,#88300,#88301,#88302,#88303,
#88304,#88305,#88306,#88307,#88308,#88309,#88310,#88311,#88312,#88313,#88314,
#88315,#88316,#88317,#88318,#88319,#88320,#88321,#88322,#88323,#88324,#88325,
#88326,#88327,#88328,#88329,#88330,#88331,#88332,#88333,#88334,#88335,#88336,
#88337,#88338,#88339,#88340,#88341),(#88342,#88343,#88344,#88345,#88346,
#88347,#88348,#88349,#88350,#88351,#88352,#88353,#88354,#88355,#88356,#88357,
#88358,#88359,#88360,#88361,#88362,#88363,#88364,#88365,#88366,#88367,#88368,
#88369,#88370,#88371,#88372,#88373,#88374,#88375,#88376,#88377,#88378,#88379,
#88380,#88381,#88382,#88383,#88384)),.UNSPECIFIED.,.F.,.F.,.F.,(4,4),(4,
1,1,1,1,1,1,1,1,1,1,1,1,1,1,1,1,1,1,1,1,1,1,1,1,1,1,1,1,1,1,1,1,1,1,1,1,
1,1,1,4),(-0.000512482261750268,0.0646339207422172),(11.858476380046,12.8518902807105,
13.8447916991131,14.8376931175158,15.8305945359184,16.8234959543211,17.8163973727237,
18.8092987911264,19.802200209529,20.7951016279317,21.7880030463343,22.780904464737,
23.7738058831396,24.7667073015423,25.7596087199449,26.7525101383476,27.7454115567502,
28.7383129751529,29.7312143935555,30.7241158119582,31.7170172303608,32.7099186487635,
33.7028200671661,34.6957214855688,35.6886229039714,36.6815243223741,37.6744257407767,
38.6673271591794,39.660228577582,40.6531299959847,41.6460314143873,42.63893283279,
43.6318342511926,44.6247356695953,45.6176370879979,46.6105385064006,47.6034399248032,
48.5963413432059,49.5892427616085,50.5821441800112,51.5750455984138),
 .UNSPECIFIED.);
#102=B_SPLINE_SURFACE_WITH_KNOTS('',3,3,((#88481,#88482,#88483,#88484,#88485,
#88486,#88487,#88488,#88489,#88490,#88491,#88492,#88493,#88494,#88495,#88496,
#88497,#88498,#88499,#88500,#88501,#88502,#88503,#88504,#88505,#88506,#88507,
#88508,#88509,#88510,#88511,#88512,#88513,#88514,#88515,#88516,#88517,#88518,
#88519,#88520,#88521,#88522,#88523),(#88524,#88525,#88526,#88527,#88528,
#88529,#88530,#88531,#88532,#88533,#88534,#88535,#88536,#88537,#88538,#88539,
#88540,#88541,#88542,#88543,#88544,#88545,#88546,#88547,#88548,#88549,#88550,
#88551,#88552,#88553,#88554,#88555,#88556,#88557,#88558,#88559,#88560,#88561,
#88562,#88563,#88564,#88565,#88566),(#88567,#88568,#88569,#88570,#88571,
#88572,#88573,#88574,#88575,#88576,#88577,#88578,#88579,#88580,#88581,#88582,
#88583,#88584,#88585,#88586,#88587,#88588,#88589,#88590,#88591,#88592,#88593,
#88594,#88595,#88596,#88597,#88598,#88599,#88600,#88601,#88602,#88603,#88604,
#88605,#88606,#88607,#88608,#88609),(#88610,#88611,#88612,#88613,#88614,
#88615,#88616,#88617,#88618,#88619,#88620,#88621,#88622,#88623,#88624,#88625,
#88626,#88627,#88628,#88629,#88630,#88631,#88632,#88633,#88634,#88635,#88636,
#88637,#88638,#88639,#88640,#88641,#88642,#88643,#88644,#88645,#88646,#88647,
#88648,#88649,#88650,#88651,#88652)),.UNSPECIFIED.,.F.,.F.,.F.,(4,4),(4,
1,1,1,1,1,1,1,1,1,1,1,1,1,1,1,1,1,1,1,1,1,1,1,1,1,1,1,1,1,1,1,1,1,1,1,1,
1,1,1,4),(-0.000452057026596796,0.0646067341429239),(14.3984001269719,15.3913015453745,
16.3842029637772,17.3771043821798,18.3700058005825,19.3629072189851,20.3558086373878,
21.3487100557904,22.3416114741931,23.3345128925957,24.3274143109984,25.320315729401,
26.3132171478037,27.3061185662063,28.299019984609,29.2919214030116,30.2848228214143,
31.2777242398169,32.2706256582196,33.2635270766222,34.2564284950248,35.2493299134275,
36.2422313318302,37.2351327502328,38.2280341686354,39.2209355870381,40.2138370054408,
41.2067384238434,42.199639842246,43.1925412606487,44.1854426790513,45.178344097454,
46.1712455158566,47.1641469342593,48.1570483526619,49.1499497710646,50.1428511894672,
51.1357526078699,52.1286540262725,53.1215554446752,54.1144568630778),
 .UNSPECIFIED.);
#103=B_SPLINE_SURFACE_WITH_KNOTS('',3,3,((#104256,#104257,#104258,#104259,
#104260,#104261,#104262,#104263,#104264,#104265,#104266,#104267,#104268,
#104269,#104270,#104271,#104272,#104273,#104274,#104275,#104276,#104277,
#104278,#104279,#104280,#104281,#104282,#104283,#104284,#104285,#104286,
#104287,#104288,#104289,#104290,#104291,#104292,#104293,#104294,#104295,
#104296,#104297,#104298,#104299,#104300,#104301,#104302,#104303,#104304,
#104305,#104306,#104307,#104308,#104309,#104310,#104311,#104312,#104313,
#104314,#104315,#104316,#104317,#104318,#104319,#104320,#104321,#104322,
#104323,#104324,#104325,#104326,#104327,#104328,#104329,#104330,#104331,
#104332,#104333,#104334,#104335,#104336,#104337,#104338,#104339,#104340,
#104341,#104342,#104343,#104344,#104345,#104346,#104347,#104348,#104349,
#104350,#104351,#104352,#104353,#104354,#104355,#104356,#104357,#104358,
#104359,#104360,#104361,#104362,#104363,#104364,#104365,#104366,#104367,
#104368,#104369,#104370,#104371,#104372,#104373,#104374,#104375,#104376,
#104377,#104378,#104379,#104380,#104381,#104382,#104383,#104384,#104385,
#104386,#104387,#104388,#104389,#104390,#104391,#104392,#104393,#104394,
#104395,#104396,#104397,#104398,#104399,#104400,#104401,#104402,#104403,
#104404,#104405,#104406,#104407,#104408,#104409,#104410,#104411,#104412,
#104413),(#104414,#104415,#104416,#104417,#104418,#104419,#104420,#104421,
#104422,#104423,#104424,#104425,#104426,#104427,#104428,#104429,#104430,
#104431,#104432,#104433,#104434,#104435,#104436,#104437,#104438,#104439,
#104440,#104441,#104442,#104443,#104444,#104445,#104446,#104447,#104448,
#104449,#104450,#104451,#104452,#104453,#104454,#104455,#104456,#104457,
#104458,#104459,#104460,#104461,#104462,#104463,#104464,#104465,#104466,
#104467,#104468,#104469,#104470,#104471,#104472,#104473,#104474,#104475,
#104476,#104477,#104478,#104479,#104480,#104481,#104482,#104483,#104484,
#104485,#104486,#104487,#104488,#104489,#104490,#104491,#104492,#104493,
#104494,#104495,#104496,#104497,#104498,#104499,#104500,#104501,#104502,
#104503,#104504,#104505,#104506,#104507,#104508,#104509,#104510,#104511,
#104512,#104513,#104514,#104515,#104516,#104517,#104518,#104519,#104520,
#104521,#104522,#104523,#104524,#104525,#104526,#104527,#104528,#104529,
#104530,#104531,#104532,#104533,#104534,#104535,#104536,#104537,#104538,
#104539,#104540,#104541,#104542,#104543,#104544,#104545,#104546,#104547,
#104548,#104549,#104550,#104551,#104552,#104553,#104554,#104555,#104556,
#104557,#104558,#104559,#104560,#104561,#104562,#104563,#104564,#104565,
#104566,#104567,#104568,#104569,#104570,#104571),(#104572,#104573,#104574,
#104575,#104576,#104577,#104578,#104579,#104580,#104581,#104582,#104583,
#104584,#104585,#104586,#104587,#104588,#104589,#104590,#104591,#104592,
#104593,#104594,#104595,#104596,#104597,#104598,#104599,#104600,#104601,
#104602,#104603,#104604,#104605,#104606,#104607,#104608,#104609,#104610,
#104611,#104612,#104613,#104614,#104615,#104616,#104617,#104618,#104619,
#104620,#104621,#104622,#104623,#104624,#104625,#104626,#104627,#104628,
#104629,#104630,#104631,#104632,#104633,#104634,#104635,#104636,#104637,
#104638,#104639,#104640,#104641,#104642,#104643,#104644,#104645,#104646,
#104647,#104648,#104649,#104650,#104651,#104652,#104653,#104654,#104655,
#104656,#104657,#104658,#104659,#104660,#104661,#104662,#104663,#104664,
#104665,#104666,#104667,#104668,#104669,#104670,#104671,#104672,#104673,
#104674,#104675,#104676,#104677,#104678,#104679,#104680,#104681,#104682,
#104683,#104684,#104685,#104686,#104687,#104688,#104689,#104690,#104691,
#104692,#104693,#104694,#104695,#104696,#104697,#104698,#104699,#104700,
#104701,#104702,#104703,#104704,#104705,#104706,#104707,#104708,#104709,
#104710,#104711,#104712,#104713,#104714,#104715,#104716,#104717,#104718,
#104719,#104720,#104721,#104722,#104723,#104724,#104725,#104726,#104727,
#104728,#104729),(#104730,#104731,#104732,#104733,#104734,#104735,#104736,
#104737,#104738,#104739,#104740,#104741,#104742,#104743,#104744,#104745,
#104746,#104747,#104748,#104749,#104750,#104751,#104752,#104753,#104754,
#104755,#104756,#104757,#104758,#104759,#104760,#104761,#104762,#104763,
#104764,#104765,#104766,#104767,#104768,#104769,#104770,#104771,#104772,
#104773,#104774,#104775,#104776,#104777,#104778,#104779,#104780,#104781,
#104782,#104783,#104784,#104785,#104786,#104787,#104788,#104789,#104790,
#104791,#104792,#104793,#104794,#104795,#104796,#104797,#104798,#104799,
#104800,#104801,#104802,#104803,#104804,#104805,#104806,#104807,#104808,
#104809,#104810,#104811,#104812,#104813,#104814,#104815,#104816,#104817,
#104818,#104819,#104820,#104821,#104822,#104823,#104824,#104825,#104826,
#104827,#104828,#104829,#104830,#104831,#104832,#104833,#104834,#104835,
#104836,#104837,#104838,#104839,#104840,#104841,#104842,#104843,#104844,
#104845,#104846,#104847,#104848,#104849,#104850,#104851,#104852,#104853,
#104854,#104855,#104856,#104857,#104858,#104859,#104860,#104861,#104862,
#104863,#104864,#104865,#104866,#104867,#104868,#104869,#104870,#104871,
#104872,#104873,#104874,#104875,#104876,#104877,#104878,#104879,#104880,
#104881,#104882,#104883,#104884,#104885,#104886,#104887)),.UNSPECIFIED.,
 .F.,.F.,.F.,(4,4),(4,1,1,1,1,1,1,1,1,1,1,1,1,1,1,1,1,1,1,1,1,1,1,1,1,1,
1,1,1,1,1,1,1,1,1,1,1,1,1,1,1,1,1,1,1,1,1,1,1,1,1,1,1,1,1,1,1,1,1,1,1,1,
1,1,1,1,1,1,1,1,1,1,1,1,1,1,1,1,1,1,1,1,1,1,1,1,1,1,1,1,1,1,1,1,1,1,1,1,
1,1,1,1,1,1,1,1,1,1,1,1,1,1,1,1,1,1,1,1,1,1,1,1,1,1,1,1,1,1,1,1,1,1,1,1,
1,1,1,1,1,1,1,1,1,1,1,1,1,1,1,1,1,1,1,1,1,4),(-0.000442659764714567,0.0663381390438544),
(11.6145431713147,12.61338032228,13.6117277967416,14.6100752712031,15.6084227456647,
16.6067702201263,17.6051176945879,18.6034651690495,19.6018126435111,20.6001601179726,
21.5985075924342,22.5968550668958,23.5952025413574,24.593550015819,25.5918974902806,
26.5902449647422,27.5885924392037,28.5869399136653,29.5852873881269,30.5836348625885,
31.5819823370501,32.5803298115117,33.5786772859733,34.5770247604348,35.5753722348964,
36.573719709358,37.5720671838196,38.5704146582812,39.5687621327428,40.5671096072044,
41.5654570816659,42.5638045561275,43.5621520305891,44.5604995050507,45.5588469795123,
46.5571944539739,47.5555419284354,48.553889402897,49.5522368773586,50.5505843518202,
51.5489318262818,52.5472793007434,53.545626775205,54.5439742496665,55.5423217241281,
56.5406691985897,57.5390166730513,58.5373641475129,59.5357116219745,60.5340590964361,
61.5324065708976,62.5307540453592,63.5291015198208,64.5274489942824,65.525796468744,
66.5241439432056,67.5224914176672,68.5208388921287,69.5191863665903,70.5175338410519,
71.5158813155135,72.5142287899751,73.5125762644367,74.5109237388983,75.5092712133598,
76.5076186878214,77.505966162283,78.5043136367446,79.5026611112062,80.5010085856678,
81.4993560601293,82.4977035345909,83.4960510090525,84.4943984835141,85.4927459579757,
86.4910934324373,87.4894409068989,88.4877883813604,89.486135855822,90.4844833302836,
91.4828308047452,92.4811782792068,93.4795257536684,94.47787322813,95.4762207025915,
96.4745681770531,97.4729156515147,98.4712631259763,99.4696106004379,100.467958074899,
101.466305549361,102.464653023823,103.463000498284,104.461347972746,105.459695447207,
106.458042921669,107.456390396131,108.454737870592,109.453085345054,110.451432819515,
111.449780293977,112.448127768438,113.4464752429,114.444822717362,115.443170191823,
116.441517666285,117.439865140746,118.438212615208,119.43656008967,120.434907564131,
121.433255038593,122.431602513054,123.429949987516,124.428297461978,125.426644936439,
126.424992410901,127.423339885362,128.421687359824,129.420034834285,130.418382308747,
131.416729783209,132.41507725767,133.413424732132,134.411772206593,135.410119681055,
136.408467155517,137.406814629978,138.40516210444,139.403509578901,140.401857053363,
141.400204527824,142.398552002286,143.396899476748,144.395246951209,145.393594425671,
146.391941900132,147.390289374594,148.388636849056,149.386984323517,150.385331797979,
151.38367927244,152.382026746902,153.380374221363,154.378721695825,155.377069170287,
156.375416644748,157.37376411921,158.372111593671,159.370459068133,160.368806542595,
161.367154017056,162.365501491518,163.363848965979,164.362196440441,165.360543914903,
166.359382730207),.UNSPECIFIED.);
#104=B_SPLINE_SURFACE_WITH_KNOTS('',3,3,((#104979,#104980,#104981,#104982,
#104983,#104984,#104985,#104986,#104987,#104988,#104989,#104990,#104991,
#104992,#104993,#104994,#104995,#104996,#104997,#104998,#104999,#105000,
#105001,#105002,#105003,#105004,#105005,#105006,#105007,#105008,#105009,
#105010,#105011,#105012,#105013,#105014,#105015,#105016,#105017,#105018,
#105019,#105020,#105021,#105022,#105023,#105024,#105025,#105026,#105027,
#105028,#105029,#105030,#105031,#105032,#105033,#105034,#105035,#105036,
#105037,#105038,#105039,#105040,#105041,#105042,#105043,#105044,#105045,
#105046,#105047,#105048,#105049,#105050,#105051,#105052,#105053,#105054,
#105055,#105056,#105057,#105058,#105059,#105060,#105061,#105062,#105063,
#105064,#105065,#105066,#105067,#105068,#105069,#105070,#105071,#105072,
#105073,#105074,#105075,#105076,#105077,#105078,#105079,#105080,#105081,
#105082,#105083,#105084,#105085,#105086,#105087,#105088,#105089,#105090,
#105091,#105092,#105093,#105094,#105095,#105096,#105097,#105098,#105099,
#105100,#105101,#105102,#105103,#105104,#105105,#105106,#105107,#105108,
#105109,#105110,#105111,#105112,#105113,#105114,#105115,#105116,#105117,
#105118,#105119,#105120,#105121,#105122,#105123,#105124,#105125,#105126,
#105127,#105128,#105129,#105130,#105131,#105132,#105133,#105134,#105135,
#105136,#105137,#105138),(#105139,#105140,#105141,#105142,#105143,#105144,
#105145,#105146,#105147,#105148,#105149,#105150,#105151,#105152,#105153,
#105154,#105155,#105156,#105157,#105158,#105159,#105160,#105161,#105162,
#105163,#105164,#105165,#105166,#105167,#105168,#105169,#105170,#105171,
#105172,#105173,#105174,#105175,#105176,#105177,#105178,#105179,#105180,
#105181,#105182,#105183,#105184,#105185,#105186,#105187,#105188,#105189,
#105190,#105191,#105192,#105193,#105194,#105195,#105196,#105197,#105198,
#105199,#105200,#105201,#105202,#105203,#105204,#105205,#105206,#105207,
#105208,#105209,#105210,#105211,#105212,#105213,#105214,#105215,#105216,
#105217,#105218,#105219,#105220,#105221,#105222,#105223,#105224,#105225,
#105226,#105227,#105228,#105229,#105230,#105231,#105232,#105233,#105234,
#105235,#105236,#105237,#105238,#105239,#105240,#105241,#105242,#105243,
#105244,#105245,#105246,#105247,#105248,#105249,#105250,#105251,#105252,
#105253,#105254,#105255,#105256,#105257,#105258,#105259,#105260,#105261,
#105262,#105263,#105264,#105265,#105266,#105267,#105268,#105269,#105270,
#105271,#105272,#105273,#105274,#105275,#105276,#105277,#105278,#105279,
#105280,#105281,#105282,#105283,#105284,#105285,#105286,#105287,#105288,
#105289,#105290,#105291,#105292,#105293,#105294,#105295,#105296,#105297,
#105298),(#105299,#105300,#105301,#105302,#105303,#105304,#105305,#105306,
#105307,#105308,#105309,#105310,#105311,#105312,#105313,#105314,#105315,
#105316,#105317,#105318,#105319,#105320,#105321,#105322,#105323,#105324,
#105325,#105326,#105327,#105328,#105329,#105330,#105331,#105332,#105333,
#105334,#105335,#105336,#105337,#105338,#105339,#105340,#105341,#105342,
#105343,#105344,#105345,#105346,#105347,#105348,#105349,#105350,#105351,
#105352,#105353,#105354,#105355,#105356,#105357,#105358,#105359,#105360,
#105361,#105362,#105363,#105364,#105365,#105366,#105367,#105368,#105369,
#105370,#105371,#105372,#105373,#105374,#105375,#105376,#105377,#105378,
#105379,#105380,#105381,#105382,#105383,#105384,#105385,#105386,#105387,
#105388,#105389,#105390,#105391,#105392,#105393,#105394,#105395,#105396,
#105397,#105398,#105399,#105400,#105401,#105402,#105403,#105404,#105405,
#105406,#105407,#105408,#105409,#105410,#105411,#105412,#105413,#105414,
#105415,#105416,#105417,#105418,#105419,#105420,#105421,#105422,#105423,
#105424,#105425,#105426,#105427,#105428,#105429,#105430,#105431,#105432,
#105433,#105434,#105435,#105436,#105437,#105438,#105439,#105440,#105441,
#105442,#105443,#105444,#105445,#105446,#105447,#105448,#105449,#105450,
#105451,#105452,#105453,#105454,#105455,#105456,#105457,#105458),(#105459,
#105460,#105461,#105462,#105463,#105464,#105465,#105466,#105467,#105468,
#105469,#105470,#105471,#105472,#105473,#105474,#105475,#105476,#105477,
#105478,#105479,#105480,#105481,#105482,#105483,#105484,#105485,#105486,
#105487,#105488,#105489,#105490,#105491,#105492,#105493,#105494,#105495,
#105496,#105497,#105498,#105499,#105500,#105501,#105502,#105503,#105504,
#105505,#105506,#105507,#105508,#105509,#105510,#105511,#105512,#105513,
#105514,#105515,#105516,#105517,#105518,#105519,#105520,#105521,#105522,
#105523,#105524,#105525,#105526,#105527,#105528,#105529,#105530,#105531,
#105532,#105533,#105534,#105535,#105536,#105537,#105538,#105539,#105540,
#105541,#105542,#105543,#105544,#105545,#105546,#105547,#105548,#105549,
#105550,#105551,#105552,#105553,#105554,#105555,#105556,#105557,#105558,
#105559,#105560,#105561,#105562,#105563,#105564,#105565,#105566,#105567,
#105568,#105569,#105570,#105571,#105572,#105573,#105574,#105575,#105576,
#105577,#105578,#105579,#105580,#105581,#105582,#105583,#105584,#105585,
#105586,#105587,#105588,#105589,#105590,#105591,#105592,#105593,#105594,
#105595,#105596,#105597,#105598,#105599,#105600,#105601,#105602,#105603,
#105604,#105605,#105606,#105607,#105608,#105609,#105610,#105611,#105612,
#105613,#105614,#105615,#105616,#105617,#105618)),.UNSPECIFIED.,.F.,.F.,
 .F.,(4,4),(4,1,1,1,1,1,1,1,1,1,1,1,1,1,1,1,1,1,1,1,1,1,1,1,1,1,1,1,1,1,
1,1,1,1,1,1,1,1,1,1,1,1,1,1,1,1,1,1,1,1,1,1,1,1,1,1,1,1,1,1,1,1,1,1,1,1,
1,1,1,1,1,1,1,1,1,1,1,1,1,1,1,1,1,1,1,1,1,1,1,1,1,1,1,1,1,1,1,1,1,1,1,1,
1,1,1,1,1,1,1,1,1,1,1,1,1,1,1,1,1,1,1,1,1,1,1,1,1,1,1,1,1,1,1,1,1,1,1,1,
1,1,1,1,1,1,1,1,1,1,1,1,1,1,1,1,1,1,1,4),(-0.000490634837690153,0.0662903764834337),
(8.30725806501226,9.30628326397092,10.3050889755407,11.3038946871105,12.3027003986803,
13.30150611025,14.3003118218198,15.2991175333896,16.2979232449594,17.2967289565291,
18.2955346680989,19.2943403796687,20.2931460912385,21.2919518028082,22.290757514378,
23.2895632259478,24.2883689375176,25.2871746490874,26.2859803606571,27.2847860722269,
28.2835917837967,29.2823974953665,30.2812032069362,31.280008918506,32.2788146300758,
33.2776203416456,34.2764260532153,35.2752317647851,36.2740374763549,37.2728431879247,
38.2716488994945,39.2704546110642,40.269260322634,41.2680660342038,42.2668717457736,
43.2656774573433,44.2644831689131,45.2632888804829,46.2620945920527,47.2609003036224,
48.2597060151922,49.258511726762,50.2573174383318,51.2561231499016,52.2549288614713,
53.2537345730411,54.2525402846109,55.2513459961807,56.2501517077504,57.2489574193202,
58.24776313089,59.2465688424598,60.2453745540296,61.2441802655993,62.2429859771691,
63.2417916887389,64.2405974003087,65.2394031118784,66.2382088234482,67.237014535018,
68.2358202465878,69.2346259581576,70.2334316697273,71.2322373812971,72.2310430928669,
73.2298488044367,74.2286545160064,75.2274602275762,76.226265939146,77.2250716507158,
78.2238773622855,79.2226830738553,80.2214887854251,81.2202944969949,82.2191002085647,
83.2179059201344,84.2167116317042,85.215517343274,86.2143230548438,87.2131287664135,
88.2119344779833,89.2107401895531,90.2095459011229,91.2083516126927,92.2071573242624,
93.2059630358322,94.204768747402,95.2035744589718,96.2023801705415,97.2011858821113,
98.1999915936811,99.1987973052509,100.197603016821,101.19640872839,102.19521443996,
103.19402015153,104.1928258631,105.19163157467,106.190437286239,107.189242997809,
108.188048709379,109.186854420949,110.185660132518,111.184465844088,112.183271555658,
113.182077267228,114.180882978798,115.179688690367,116.178494401937,117.177300113507,
118.176105825077,119.174911536646,120.173717248216,121.172522959786,122.171328671356,
123.170134382926,124.168940094495,125.167745806065,126.166551517635,127.165357229205,
128.164162940774,129.162968652344,130.161774363914,131.160580075484,132.159385787054,
133.158191498623,134.156997210193,135.155802921763,136.154608633333,137.153414344902,
138.152220056472,139.151025768042,140.149831479612,141.148637191182,142.147442902751,
143.146248614321,144.145054325891,145.143860037461,146.14266574903,147.1414714606,
148.14027717217,149.13908288374,150.13788859531,151.136694306879,152.135500018449,
153.134305730019,154.133111441589,155.131917153158,156.130722864728,157.129528576298,
158.128334287868,159.127139999438,160.125945711007,161.124751422577,162.123557134147,
163.122362845717,164.121168557286,165.120464903694),.UNSPECIFIED.);
#105=CONICAL_SURFACE('',#7514,7.5,0.785398163397451);
#106=CONICAL_SURFACE('',#7707,2.5,0.785398163397448);
#107=ELLIPSE('',#7497,6.37218304159764,5.71843041940893);
#108=ELLIPSE('',#7498,6.23535398393752,5.62417080294212);
#109=B_SPLINE_CURVE_WITH_KNOTS('',3,(#8945,#8946,#8947,#8948,#8949,#8950,
#8951,#8952,#8953,#8954,#8955,#8956,#8957,#8958,#8959,#8960,#8961,#8962,
#8963,#8964,#8965,#8966,#8967,#8968,#8969,#8970,#8971,#8972,#8973,#8974,
#8975,#8976,#8977,#8978,#8979,#8980,#8981,#8982,#8983,#8984,#8985,#8986,
#8987,#8988,#8989,#8990,#8991,#8992,#8993,#8994,#8995,#8996,#8997,#8998,
#8999,#9000,#9001,#9002,#9003,#9004,#9005,#9006,#9007,#9008,#9009,#9010,
#9011,#9012,#9013,#9014,#9015,#9016,#9017,#9018,#9019,#9020,#9021,#9022,
#9023,#9024,#9025,#9026,#9027,#9028,#9029,#9030,#9031,#9032,#9033,#9034,
#9035,#9036,#9037,#9038,#9039,#9040,#9041,#9042,#9043,#9044,#9045,#9046,
#9047,#9048,#9049,#9050,#9051,#9052,#9053,#9054,#9055,#9056,#9057,#9058,
#9059,#9060,#9061,#9062,#9063,#9064,#9065,#9066,#9067,#9068,#9069,#9070,
#9071,#9072,#9073,#9074,#9075,#9076,#9077),.UNSPECIFIED.,.F.,.F.,(4,3,3,
3,3,3,3,3,3,3,3,3,3,3,3,3,3,3,3,3,3,3,3,3,3,3,3,3,3,3,3,3,3,3,3,3,3,3,3,
3,3,3,3,3,4),(10.3769047257236,10.4527816077004,10.5285705693428,10.6042884681534,
10.6799520845211,10.7575068350479,10.8331228590851,10.9087383619952,10.9843684364558,
11.0633738495257,11.1391179258011,11.2149124638109,11.2908054681926,11.3003900887353,
11.3780272612758,11.4555770973186,11.5330551296334,11.610476839924,11.6878576694966,
11.7652227836524,11.8425815660687,11.9199479598844,11.9973359098454,12.0748026220138,
12.152309867659,12.2299284461808,12.3001437001047,12.3771329899878,12.4540352583854,
12.5308666134793,12.6076431087672,12.6843807554362,12.761320324941,12.8380442272445,
12.9147794477103,12.9915404486635,13.0686296643661,13.1455244992986,13.2227109053863,
13.2998973114741,13.3773518589841,13.4546868229213,13.531953152234,13.6091519910909,
13.661913603788),.UNSPECIFIED.);
#110=B_SPLINE_CURVE_WITH_KNOTS('',3,(#9080,#9081,#9082,#9083,#9084,#9085,
#9086,#9087,#9088,#9089,#9090,#9091,#9092,#9093,#9094,#9095,#9096,#9097,
#9098,#9099,#9100,#9101,#9102,#9103,#9104,#9105,#9106,#9107,#9108,#9109,
#9110,#9111,#9112,#9113,#9114,#9115,#9116,#9117,#9118,#9119,#9120,#9121,
#9122,#9123,#9124,#9125,#9126,#9127,#9128,#9129,#9130,#9131,#9132,#9133,
#9134,#9135,#9136,#9137,#9138,#9139,#9140,#9141,#9142,#9143,#9144,#9145,
#9146,#9147,#9148,#9149,#9150,#9151,#9152,#9153,#9154,#9155),
 .UNSPECIFIED.,.F.,.F.,(4,3,3,3,3,3,3,3,3,3,3,3,3,3,3,3,3,3,3,3,3,3,3,3,
3,4),(11.6150328478195,11.6974944507364,11.7799553878079,11.8624156864323,
11.9448753740057,12.0273344779219,12.1097930255731,12.1922510443491,12.2747085616382,
12.3613793526067,12.4438461362102,12.5263112474637,12.6087747960201,12.6912368915109,
12.7736976435469,12.8561571617202,12.9386155556056,13.0210729347622,13.1035393166313,
13.1860025148144,13.2684629678307,13.3509211140436,13.4333867103942,13.515846583346,
13.598310680714,13.661441217134),.UNSPECIFIED.);
#111=B_SPLINE_CURVE_WITH_KNOTS('',3,(#9161,#9162,#9163,#9164,#9165,#9166,
#9167,#9168,#9169,#9170,#9171,#9172,#9173,#9174,#9175,#9176,#9177,#9178,
#9179,#9180,#9181,#9182,#9183,#9184,#9185,#9186,#9187,#9188,#9189,#9190,
#9191,#9192,#9193,#9194,#9195,#9196,#9197,#9198,#9199,#9200,#9201,#9202,
#9203,#9204,#9205,#9206,#9207,#9208,#9209,#9210,#9211,#9212,#9213,#9214,
#9215,#9216,#9217,#9218,#9219,#9220,#9221,#9222,#9223,#9224,#9225,#9226,
#9227,#9228,#9229,#9230,#9231,#9232,#9233,#9234,#9235,#9236,#9237,#9238,
#9239,#9240,#9241,#9242,#9243,#9244,#9245,#9246,#9247,#9248,#9249,#9250,
#9251,#9252,#9253,#9254,#9255,#9256,#9257,#9258,#9259,#9260,#9261,#9262,
#9263,#9264,#9265,#9266,#9267,#9268,#9269,#9270,#9271,#9272,#9273,#9274,
#9275,#9276,#9277,#9278,#9279,#9280,#9281,#9282,#9283,#9284,#9285,#9286,
#9287,#9288,#9289,#9290,#9291,#9292,#9293,#9294,#9295,#9296,#9297,#9298,
#9299,#9300,#9301,#9302,#9303,#9304,#9305,#9306,#9307,#9308,#9309,#9310,
#9311,#9312,#9313,#9314,#9315,#9316,#9317),.UNSPECIFIED.,.F.,.F.,(4,3,3,
3,3,3,3,3,3,3,3,3,3,3,3,3,3,3,3,3,3,3,3,3,3,3,3,3,3,3,3,3,3,3,3,3,3,3,3,
3,3,3,3,3,3,3,3,3,3,3,3,3,4),(15.7079632679501,15.7904254739863,15.8728873317261,
15.9553488480197,16.0378100297171,16.1202708836684,16.2027314167227,16.2851916357294,
16.3676515475373,16.450111158995,16.5325704769509,16.6150295082534,16.69748825975,
16.7799467382885,16.8624049507163,16.9448629038807,17.0273206046285,17.1097780598065,
17.1922352762608,17.2782475027625,17.361571847186,17.4440384526314,17.5265042138728,
17.6089691583254,17.6914333134013,17.7738967065101,17.8563593650587,17.9388213164515,
18.0212825880902,18.1037432073744,18.1862032017012,18.2686625984657,18.3511214250608,
18.4335797088775,18.516037477305,18.5984947577303,18.6826279931418,18.7650939912334,
18.8475583675889,18.9300212318511,19.0124826936418,19.0949428625629,19.1774018481984,
19.2598597601156,19.3454556056404,19.4279203422406,19.5103821142425,19.5928413600846,
19.6752985180616,19.7577610363429,19.8402187071978,19.9226774971486,19.9446265243138),
 .UNSPECIFIED.);
#112=B_SPLINE_CURVE_WITH_KNOTS('',3,(#9318,#9319,#9320,#9321,#9322,#9323,
#9324,#9325,#9326,#9327,#9328,#9329,#9330,#9331,#9332,#9333,#9334,#9335,
#9336,#9337,#9338,#9339,#9340,#9341,#9342,#9343,#9344,#9345,#9346,#9347,
#9348,#9349,#9350,#9351,#9352,#9353,#9354,#9355,#9356,#9357,#9358,#9359,
#9360,#9361,#9362,#9363,#9364,#9365,#9366,#9367,#9368,#9369,#9370,#9371,
#9372,#9373,#9374,#9375,#9376,#9377,#9378,#9379,#9380,#9381,#9382,#9383,
#9384,#9385,#9386,#9387,#9388,#9389,#9390,#9391,#9392,#9393,#9394,#9395,
#9396,#9397,#9398,#9399,#9400,#9401,#9402),.UNSPECIFIED.,.F.,.F.,(4,3,3,
3,3,3,3,3,3,3,3,3,3,3,3,3,3,3,3,3,3,3,3,3,3,3,3,3,4),(13.661913603788,13.74163076867,
13.8187547130951,13.8958776827639,13.9730138226308,14.0501772823724,14.1274181186823,
14.2047051682193,14.2820865197271,14.2996509228435,14.3812500628693,14.4627432830108,
14.5469393943902,14.6282018702999,14.7093852717979,14.79047384344,14.7995277285281,
14.8805147931035,14.9615778600741,15.0460345286088,15.1273201750453,15.2086838620509,
15.2901690288209,15.2994045342128,15.3835468826529,15.4674320024452,15.5511589990445,
15.634627823912,15.7079632679501),.UNSPECIFIED.);
#113=B_SPLINE_CURVE_WITH_KNOTS('',3,(#9404,#9405,#9406,#9407,#9408,#9409,
#9410,#9411,#9412,#9413,#9414,#9415,#9416,#9417,#9418,#9419,#9420,#9421,
#9422,#9423,#9424,#9425,#9426,#9427,#9428,#9429,#9430,#9431,#9432,#9433,
#9434,#9435,#9436,#9437,#9438,#9439,#9440,#9441,#9442,#9443,#9444,#9445,
#9446,#9447,#9448,#9449,#9450,#9451,#9452,#9453,#9454,#9455,#9456,#9457,
#9458,#9459,#9460,#9461,#9462,#9463,#9464,#9465,#9466,#9467,#9468,#9469,
#9470,#9471,#9472,#9473,#9474,#9475,#9476,#9477,#9478,#9479),
 .UNSPECIFIED.,.F.,.F.,(4,3,3,3,3,3,3,3,3,3,3,3,3,3,3,3,3,3,3,3,3,3,3,3,
3,4),(13.661441217134,13.7439028162622,13.8263637496976,13.9088240448388,
13.9912837290816,14.0737428298202,14.1562013744464,14.2386593903501,14.3211169049196,
14.4077589589255,14.4902257335027,14.5726908363028,14.6551543769792,14.7376164651628,
14.8200772104646,14.9025367224764,14.9849951107731,15.0674524849134,15.1499188490036,
15.2323820317,15.314842471521,15.3973006068293,15.4797661687128,15.5622260163633,
15.6446900491511,15.7073897690138),.UNSPECIFIED.);
#114=B_SPLINE_CURVE_WITH_KNOTS('',3,(#9480,#9481,#9482,#9483,#9484,#9485,
#9486,#9487,#9488,#9489,#9490,#9491,#9492,#9493,#9494,#9495,#9496,#9497,
#9498,#9499,#9500,#9501,#9502,#9503,#9504,#9505,#9506,#9507,#9508,#9509,
#9510,#9511,#9512,#9513,#9514,#9515,#9516,#9517,#9518,#9519,#9520,#9521,
#9522,#9523,#9524,#9525,#9526,#9527,#9528,#9529,#9530,#9531,#9532,#9533,
#9534,#9535,#9536,#9537,#9538,#9539,#9540,#9541,#9542,#9543,#9544,#9545,
#9546,#9547,#9548,#9549,#9550,#9551,#9552,#9553,#9554,#9555,#9556,#9557,
#9558,#9559,#9560,#9561,#9562,#9563,#9564,#9565,#9566,#9567,#9568,#9569,
#9570,#9571,#9572,#9573,#9574,#9575,#9576,#9577,#9578,#9579,#9580,#9581,
#9582,#9583,#9584,#9585,#9586,#9587,#9588,#9589,#9590,#9591,#9592,#9593,
#9594,#9595,#9596,#9597,#9598,#9599,#9600,#9601,#9602,#9603,#9604,#9605,
#9606,#9607,#9608,#9609,#9610,#9611,#9612,#9613,#9614,#9615,#9616,#9617,
#9618,#9619,#9620,#9621,#9622,#9623,#9624,#9625,#9626,#9627,#9628,#9629,
#9630,#9631,#9632,#9633,#9634,#9635,#9636,#9637,#9638,#9639,#9640,#9641,
#9642,#9643,#9644,#9645,#9646,#9647,#9648,#9649,#9650,#9651),
 .UNSPECIFIED.,.F.,.F.,(4,3,3,3,3,3,3,3,3,3,3,3,3,3,3,3,3,3,3,3,3,3,3,3,
3,3,3,3,3,3,3,3,3,3,3,3,3,3,3,3,3,3,3,3,3,3,3,3,3,3,3,3,3,3,3,3,3,4),(15.7079632952952,
15.7840025321932,15.8599648001924,15.9358667980574,16.011725164846,16.0875668207261,
16.1634020177953,16.2392457593701,16.3151130540793,16.3910644371312,16.4670598741112,
16.5431728456518,16.6070728880741,16.6845222139964,16.7618780204501,16.8391560772364,
16.9163720976792,16.9935417500323,17.0706879712162,17.1478232165181,17.2249616213568,
17.3021173203171,17.3793459856373,17.4566118378682,17.5339848547524,17.605480896125,
17.6870848273324,17.7685832167635,17.8526086376102,17.9338773603292,18.0192811302398,
18.1003738605163,18.1046849001504,18.1856750726475,18.2667409241249,18.3510279191377,
18.432315204022,18.5136802303654,18.5951660787181,18.6038889041759,18.6814065367343,
18.7588426168442,18.8362127393099,18.9135324517233,18.9908172650905,19.0680957040123,
19.1453735563204,19.2226648395218,19.2999835760365,19.3773904489576,19.4548430590586,
19.5324155966512,19.6022969122268,19.6791914072041,19.7559671805278,19.8326746431303,
19.9093157129169,19.9452932995404),.UNSPECIFIED.);
#115=B_SPLINE_CURVE_WITH_KNOTS('',3,(#9657,#9658,#9659,#9660,#9661,#9662,
#9663,#9664,#9665,#9666,#9667,#9668,#9669,#9670,#9671,#9672,#9673,#9674,
#9675,#9676,#9677,#9678,#9679,#9680,#9681,#9682,#9683,#9684,#9685,#9686,
#9687,#9688,#9689,#9690,#9691,#9692,#9693,#9694,#9695,#9696,#9697,#9698,
#9699,#9700,#9701,#9702,#9703,#9704,#9705,#9706,#9707,#9708,#9709,#9710,
#9711,#9712,#9713,#9714,#9715,#9716,#9717,#9718,#9719,#9720,#9721,#9722,
#9723,#9724,#9725,#9726,#9727,#9728,#9729,#9730,#9731,#9732,#9733,#9734,
#9735,#9736,#9737,#9738,#9739,#9740,#9741,#9742,#9743,#9744,#9745,#9746,
#9747,#9748,#9749,#9750,#9751,#9752,#9753,#9754,#9755,#9756,#9757,#9758,
#9759,#9760,#9761,#9762,#9763,#9764,#9765,#9766,#9767,#9768,#9769,#9770,
#9771,#9772,#9773,#9774,#9775,#9776,#9777,#9778,#9779,#9780,#9781,#9782,
#9783,#9784,#9785,#9786,#9787,#9788,#9789,#9790,#9791,#9792,#9793,#9794,
#9795,#9796,#9797,#9798,#9799,#9800,#9801,#9802,#9803,#9804,#9805,#9806,
#9807,#9808,#9809,#9810,#9811,#9812,#9813,#9814,#9815,#9816,#9817,#9818,
#9819,#9820,#9821,#9822),.UNSPECIFIED.,.F.,.F.,(4,3,3,3,3,3,3,3,3,3,3,3,
3,3,3,3,3,3,3,3,3,3,3,3,3,3,3,3,3,3,3,3,3,3,3,3,3,3,3,3,3,3,3,3,3,3,3,3,
3,3,3,3,3,3,3,4),(21.9911485751297,22.0810996357526,22.1714401170014,22.262210689136,
22.2976798137984,22.3751954065669,22.4526295180584,22.5299977443591,22.6073156343901,
22.6845987005346,22.7618755834062,22.8391519603175,22.9164418501864,22.9937592768941,
23.0711652742691,23.1486170734114,23.2261896715283,23.2974334251678,23.374282115361,
23.4510370293504,23.5277144368787,23.6043305452548,23.6809015129049,23.7579372033589,
23.8344796918291,23.9110280983708,23.9875969999661,24.0649945091089,24.1416856601052,
24.2194363483211,24.2971870365371,24.3747045940136,24.4521348195148,24.5294933687083,
24.6067958458031,24.6840578144639,24.7613050472459,24.838546565628,24.9157964232056,
24.9930686756278,25.0704216413305,25.1478160415037,25.2253243771904,25.2969406479065,
25.374461596459,25.4518944782164,25.5292549516708,25.6065586232433,25.6841896108983,
25.7614330861104,25.8386698613634,25.9159139891612,25.9938371229918,26.0711686401118,
26.1493875822976,26.2276065244835),.UNSPECIFIED.);
#116=B_SPLINE_CURVE_WITH_KNOTS('',3,(#9823,#9824,#9825,#9826,#9827,#9828,
#9829,#9830,#9831,#9832,#9833,#9834,#9835,#9836,#9837,#9838,#9839,#9840,
#9841,#9842,#9843,#9844,#9845,#9846,#9847,#9848,#9849,#9850,#9851,#9852,
#9853,#9854,#9855,#9856,#9857,#9858,#9859,#9860,#9861,#9862,#9863,#9864,
#9865,#9866,#9867,#9868,#9869,#9870,#9871,#9872,#9873,#9874,#9875,#9876,
#9877,#9878,#9879,#9880,#9881,#9882,#9883,#9884,#9885,#9886,#9887,#9888,
#9889,#9890,#9891,#9892,#9893,#9894,#9895,#9896,#9897,#9898),
 .UNSPECIFIED.,.F.,.F.,(4,3,3,3,3,3,3,3,3,3,3,3,3,3,3,3,3,3,3,3,3,3,3,3,
3,4),(19.9446265243138,20.0270881281676,20.1095490661382,20.1920093656239,
20.2744690540208,20.3569281587228,20.439386707122,20.5218447266083,20.6043022445699,
20.6909801402299,20.7734469260655,20.8559120394093,20.9383755899145,21.0208376872122,
21.1032984409136,21.1857579606107,21.2682163558785,21.3506737362757,21.4331401225421,
21.5156033245558,21.5980637808363,21.6805219297472,21.7629875346264,21.8454474138409,
21.9279115272047,21.9911485751297),.UNSPECIFIED.);
#117=B_SPLINE_CURVE_WITH_KNOTS('',3,(#9900,#9901,#9902,#9903,#9904,#9905,
#9906,#9907,#9908,#9909,#9910,#9911,#9912,#9913,#9914,#9915,#9916,#9917,
#9918,#9919,#9920,#9921,#9922,#9923,#9924,#9925,#9926,#9927,#9928,#9929,
#9930,#9931,#9932,#9933,#9934,#9935,#9936,#9937,#9938,#9939,#9940,#9941,
#9942,#9943,#9944,#9945,#9946,#9947,#9948,#9949,#9950,#9951,#9952,#9953,
#9954,#9955,#9956,#9957,#9958,#9959,#9960,#9961,#9962,#9963,#9964,#9965,
#9966,#9967,#9968,#9969,#9970,#9971,#9972,#9973,#9974,#9975,#9976,#9977,
#9978,#9979,#9980,#9981),.UNSPECIFIED.,.F.,.F.,(4,3,3,3,3,3,3,3,3,3,3,3,
3,3,3,3,3,3,3,3,3,3,3,3,3,3,3,4),(19.9452932995404,20.0218764286094,20.098449829705,
20.1750215389486,20.2516061131552,20.3282181146041,20.4049138676908,20.4816564455584,
20.5585073870191,20.6007049202777,20.6782317587392,20.7556714715145,20.8330397034221,
20.9103520480074,20.9876240584291,21.0648814996859,21.1421333592579,21.2193936816471,
21.2966765134702,21.3740398998633,21.4514448142151,21.5289629928235,21.5991129283287,
21.6853515317677,21.7712477478555,21.8569207098858,21.9422242479864,21.9911485750449),
 .UNSPECIFIED.);
#118=B_SPLINE_CURVE_WITH_KNOTS('',3,(#9982,#9983,#9984,#9985,#9986,#9987,
#9988,#9989,#9990,#9991,#9992,#9993,#9994,#9995,#9996,#9997,#9998,#9999,
#10000,#10001,#10002,#10003,#10004,#10005,#10006,#10007,#10008,#10009,#10010,
#10011,#10012,#10013,#10014,#10015,#10016,#10017,#10018,#10019,#10020,#10021,
#10022,#10023,#10024,#10025,#10026,#10027,#10028,#10029,#10030,#10031,#10032,
#10033,#10034,#10035,#10036,#10037,#10038,#10039,#10040,#10041,#10042,#10043,
#10044,#10045,#10046,#10047,#10048,#10049,#10050,#10051,#10052,#10053,#10054,
#10055,#10056,#10057,#10058,#10059,#10060,#10061,#10062,#10063,#10064,#10065,
#10066,#10067,#10068,#10069,#10070,#10071,#10072,#10073,#10074,#10075,#10076,
#10077,#10078,#10079,#10080,#10081,#10082,#10083,#10084,#10085,#10086,#10087,
#10088,#10089,#10090,#10091,#10092,#10093,#10094,#10095,#10096,#10097,#10098,
#10099,#10100,#10101,#10102,#10103,#10104,#10105,#10106,#10107,#10108,#10109,
#10110,#10111,#10112,#10113,#10114,#10115,#10116,#10117,#10118,#10119,#10120,
#10121,#10122,#10123,#10124,#10125,#10126,#10127,#10128,#10129,#10130,#10131,
#10132,#10133,#10134,#10135,#10136,#10137,#10138,#10139,#10140,#10141,#10142,
#10143,#10144,#10145,#10146,#10147,#10148,#10149,#10150,#10151,#10152,#10153),
 .UNSPECIFIED.,.F.,.F.,(4,3,3,3,3,3,3,3,3,3,3,3,3,3,3,3,3,3,3,3,3,3,3,3,
3,3,3,3,3,3,3,3,3,3,3,3,3,3,3,3,3,3,3,3,3,3,3,3,3,3,3,3,3,3,3,3,3,4),(21.9911485751295,
22.0695184733941,22.1479066212012,22.2263255018552,22.3047876151167,22.3833550279714,
22.46197914016,22.5407293214231,22.5975209363796,22.6743586591899,22.7511073831277,
22.8277833450473,22.90440272373,22.9809816530099,23.0578500644375,23.1344119450102,
23.2109840282971,23.2875808824072,23.364667897913,23.441396891209,23.5186629178197,
23.5959289444305,23.6735231120596,23.7510248731705,23.8284498505637,23.9058136120981,
23.98313168169,24.0604268738106,24.1377114056863,24.2149992848633,24.2923045181101,
24.3696820492007,24.4470966131919,24.5246167262537,24.5943369524814,24.6758223858517,
24.7572035843824,24.8412879274136,24.922444368254,25.0035242804619,25.0845134135558,
25.0935409565069,25.1745548343586,25.2556443278473,25.3399194860185,25.4212298041297,
25.5026175723088,25.5841255927926,25.5927449605323,25.672078121751,25.7495172508508,
25.8268944839681,25.9042238961777,25.9850204847038,26.0623029562465,26.1395795805683,
26.2168751299167,26.2274102502822),.UNSPECIFIED.);
#119=B_SPLINE_CURVE_WITH_KNOTS('',3,(#10159,#10160,#10161,#10162,#10163,
#10164,#10165,#10166,#10167,#10168,#10169,#10170,#10171,#10172,#10173,#10174,
#10175,#10176,#10177,#10178,#10179,#10180,#10181,#10182,#10183,#10184,#10185,
#10186,#10187,#10188,#10189,#10190,#10191,#10192,#10193,#10194,#10195,#10196,
#10197,#10198,#10199,#10200,#10201,#10202,#10203,#10204,#10205,#10206,#10207,
#10208,#10209,#10210,#10211,#10212,#10213,#10214,#10215,#10216,#10217,#10218,
#10219,#10220,#10221,#10222,#10223,#10224,#10225,#10226,#10227,#10228,#10229,
#10230,#10231,#10232,#10233,#10234,#10235,#10236,#10237,#10238,#10239,#10240,
#10241,#10242,#10243,#10244,#10245,#10246,#10247,#10248,#10249,#10250,#10251,
#10252,#10253,#10254,#10255,#10256,#10257,#10258,#10259,#10260,#10261,#10262,
#10263,#10264,#10265,#10266,#10267,#10268,#10269,#10270,#10271,#10272,#10273,
#10274,#10275,#10276,#10277,#10278,#10279,#10280,#10281,#10282,#10283,#10284,
#10285,#10286,#10287,#10288,#10289,#10290,#10291,#10292,#10293,#10294,#10295,
#10296,#10297,#10298,#10299,#10300,#10301,#10302,#10303,#10304,#10305,#10306,
#10307,#10308,#10309,#10310,#10311,#10312,#10313,#10314,#10315,#10316,#10317,
#10318,#10319,#10320,#10321,#10322,#10323,#10324,#10325,#10326,#10327,#10328,
#10329,#10330),.UNSPECIFIED.,.F.,.F.,(4,3,3,3,3,3,3,3,3,3,3,3,3,3,3,3,3,
3,3,3,3,3,3,3,3,3,3,3,3,3,3,3,3,3,3,3,3,3,3,3,3,3,3,3,3,3,3,3,3,3,3,3,3,
3,3,3,3,4),(28.2743338823092,28.2962014820146,28.3776854389874,28.4590647871843,
28.543318162313,28.6244716418665,28.7055483043996,28.7865337170947,28.7960782876993,
28.8770866933325,28.9581709601934,29.0426169934911,29.1239230857728,29.2053068862678,
29.286811558155,29.295955093384,29.3734708701903,29.4509051691213,29.5282735860479,
29.6055916696782,29.6828749321845,29.7601520149366,29.8374285938519,29.9147186876652,
29.9920363200754,30.0694425247984,30.146894532504,30.2244673392231,30.2957087047533,
30.3725573280629,30.4493121745814,30.5259895141068,30.6026055540021,30.6791764527465,
30.7562121856686,30.8327546044912,30.9093029411695,30.9858717727319,31.0632694085796,
31.1399604896431,31.2177114028829,31.2954623161227,31.3729798679754,31.4504100876332,
31.5277686307702,31.6050711016021,31.6823330637999,31.7595802898336,31.8368218012941,
31.9140716517821,31.9913438969519,32.0686968551811,32.1460912477492,32.2235995756764,
32.2952159274921,32.3727404680712,32.4501637622965,32.5116015420207),
 .UNSPECIFIED.);
#120=B_SPLINE_CURVE_WITH_KNOTS('',3,(#10331,#10332,#10333,#10334,#10335,
#10336,#10337,#10338,#10339,#10340,#10341,#10342,#10343,#10344,#10345,#10346,
#10347,#10348,#10349,#10350,#10351,#10352,#10353,#10354,#10355,#10356,#10357,
#10358,#10359,#10360,#10361,#10362,#10363,#10364,#10365,#10366,#10367,#10368,
#10369,#10370,#10371,#10372,#10373,#10374,#10375,#10376,#10377,#10378,#10379,
#10380,#10381,#10382,#10383,#10384,#10385,#10386,#10387,#10388,#10389,#10390,
#10391,#10392,#10393,#10394,#10395,#10396,#10397,#10398,#10399,#10400,#10401,
#10402,#10403,#10404,#10405,#10406,#10407,#10408,#10409,#10410,#10411,#10412),
 .UNSPECIFIED.,.F.,.F.,(4,3,3,3,3,3,3,3,3,3,3,3,3,3,3,3,3,3,3,3,3,3,3,3,
3,3,3,4),(26.2276065244835,26.2966942592759,26.3735154661939,26.4502474382501,
26.5269064263103,26.6035086227474,26.6800701746596,26.7571173866578,26.8336615714257,
26.9102158616206,26.9867948367697,27.0642080952385,27.1409195856865,27.2186837281658,
27.2964478706452,27.3737810706327,27.4510218443257,27.5281860713245,27.605289574782,
27.6823481331002,27.7593848991671,27.836412147927,27.9134441159848,27.9904950400087,
28.0676179573777,28.1447798002582,28.2220420502019,28.2743338821727),
 .UNSPECIFIED.);
#121=B_SPLINE_CURVE_WITH_KNOTS('',3,(#10414,#10415,#10416,#10417,#10418,
#10419,#10420,#10421,#10422,#10423,#10424,#10425,#10426,#10427,#10428,#10429,
#10430,#10431,#10432,#10433,#10434,#10435,#10436,#10437,#10438,#10439,#10440,
#10441,#10442,#10443,#10444,#10445,#10446,#10447,#10448,#10449,#10450,#10451,
#10452,#10453,#10454,#10455,#10456,#10457,#10458,#10459,#10460,#10461,#10462,
#10463,#10464,#10465,#10466,#10467,#10468,#10469,#10470,#10471,#10472,#10473,
#10474,#10475,#10476,#10477,#10478,#10479,#10480,#10481,#10482,#10483,#10484,
#10485,#10486,#10487,#10488,#10489,#10490,#10491,#10492,#10493,#10494,#10495),
 .UNSPECIFIED.,.F.,.F.,(4,3,3,3,3,3,3,3,3,3,3,3,3,3,3,3,3,3,3,3,3,3,3,3,
3,3,3,4),(26.2274102502822,26.3047485634863,26.3821761878827,26.4596522575986,
26.5372438213464,26.5911529685832,26.6680164211604,26.7447863214985,26.8214789265624,
26.8981104312959,26.9746969820839,27.0515549814027,27.1281133751358,27.2046777808017,
27.2812627650986,27.3583373179825,27.435044209929,27.5123025932816,27.5895609766342,
27.6669870549331,27.7442937112837,27.821530825017,27.8987126059822,27.975853229399,
28.0529751002743,28.130084055375,28.2072164237887,28.2743338823091),
 .UNSPECIFIED.);
#122=B_SPLINE_CURVE_WITH_KNOTS('',3,(#10496,#10497,#10498,#10499,#10500,
#10501,#10502,#10503,#10504,#10505,#10506,#10507,#10508,#10509,#10510,#10511,
#10512,#10513,#10514,#10515,#10516,#10517,#10518,#10519,#10520,#10521,#10522,
#10523,#10524,#10525,#10526,#10527,#10528,#10529,#10530,#10531,#10532,#10533,
#10534,#10535,#10536,#10537,#10538,#10539,#10540,#10541,#10542,#10543,#10544,
#10545,#10546,#10547,#10548,#10549,#10550,#10551,#10552,#10553,#10554,#10555,
#10556,#10557,#10558,#10559,#10560,#10561,#10562,#10563,#10564,#10565,#10566,
#10567,#10568,#10569,#10570,#10571,#10572,#10573,#10574,#10575,#10576,#10577,
#10578,#10579,#10580,#10581,#10582,#10583,#10584,#10585,#10586,#10587,#10588,
#10589,#10590,#10591,#10592,#10593,#10594,#10595,#10596,#10597,#10598,#10599,
#10600,#10601,#10602,#10603,#10604,#10605,#10606,#10607,#10608,#10609,#10610,
#10611,#10612,#10613,#10614,#10615,#10616,#10617,#10618,#10619,#10620,#10621,
#10622,#10623,#10624,#10625,#10626,#10627,#10628,#10629,#10630,#10631,#10632,
#10633,#10634,#10635,#10636,#10637,#10638,#10639,#10640,#10641,#10642,#10643,
#10644,#10645,#10646,#10647,#10648,#10649,#10650,#10651,#10652,#10653,#10654,
#10655,#10656,#10657,#10658,#10659,#10660,#10661,#10662,#10663,#10664),
 .UNSPECIFIED.,.F.,.F.,(4,3,3,3,3,3,3,3,3,3,3,3,3,3,3,3,3,3,3,3,3,3,3,3,
3,3,3,3,3,3,3,3,3,3,3,3,3,3,3,3,3,3,3,3,3,3,3,3,3,3,3,3,3,3,3,3,4),(28.2743338823925,
28.3653751030432,28.4569879802351,28.5492606248583,28.5879689846851,28.6654990819551,
28.7429420901964,28.8203136506885,28.8976293534778,28.9749047482534,29.0521656022372,
29.1294208913882,29.2066846571501,29.283970943089,29.3613377821852,29.4387461535387,
29.5162677639265,29.586376992736,29.6632130347834,29.7399600605163,29.8166343081586,
29.8932519578245,29.9698291446533,30.04669862667,30.1232587394907,30.1998290469636,
30.2764241183324,30.353514338946,30.4302415458469,30.5075132733169,30.5847850007869,
30.6623796722761,30.7398819404659,30.8173074276379,30.8946717011361,30.9719902843659,
31.0492859909964,31.126571037823,31.2038594319365,31.2811651796506,31.3585432218276,
31.4359582957656,31.5134789122165,31.5831930088378,31.6646793075531,31.7460613742313,
31.8301452838893,31.9113025873758,31.9923833559512,32.0733733331285,32.0823970128633,
32.1633981440914,32.2444746546452,32.3256813350582,32.4069598838733,32.4883571744755,
32.5108171892216),.UNSPECIFIED.);
#123=B_SPLINE_CURVE_WITH_KNOTS('',3,(#10670,#10671,#10672,#10673,#10674,
#10675,#10676,#10677,#10678,#10679,#10680,#10681,#10682,#10683,#10684,#10685,
#10686,#10687,#10688,#10689,#10690,#10691,#10692,#10693,#10694,#10695,#10696,
#10697,#10698,#10699,#10700,#10701,#10702,#10703,#10704,#10705,#10706,#10707,
#10708,#10709,#10710,#10711,#10712,#10713,#10714,#10715,#10716,#10717,#10718,
#10719,#10720,#10721,#10722,#10723,#10724,#10725,#10726,#10727,#10728,#10729,
#10730,#10731,#10732,#10733,#10734,#10735,#10736,#10737,#10738,#10739,#10740,
#10741,#10742,#10743,#10744,#10745,#10746,#10747,#10748,#10749,#10750,#10751,
#10752,#10753,#10754,#10755,#10756,#10757,#10758,#10759,#10760,#10761,#10762,
#10763,#10764,#10765,#10766,#10767,#10768,#10769,#10770,#10771,#10772,#10773,
#10774,#10775,#10776,#10777,#10778,#10779,#10780,#10781,#10782,#10783,#10784,
#10785,#10786,#10787,#10788,#10789,#10790,#10791,#10792,#10793,#10794,#10795,
#10796,#10797,#10798,#10799,#10800,#10801,#10802,#10803,#10804,#10805,#10806,
#10807,#10808,#10809,#10810,#10811,#10812,#10813,#10814,#10815,#10816,#10817,
#10818,#10819,#10820,#10821,#10822,#10823,#10824,#10825,#10826),
 .UNSPECIFIED.,.F.,.F.,(4,3,3,3,3,3,3,3,3,3,3,3,3,3,3,3,3,3,3,3,3,3,3,3,
3,3,3,3,3,3,3,3,3,3,3,3,3,3,3,3,3,3,3,3,3,3,3,3,3,3,3,3,4),(34.5575191894888,
34.639981395525,34.7224432532648,34.8049047695584,34.887365951256,34.9698268052072,
35.0522873382615,35.1347475572681,35.217207469076,35.2996670805337,35.3821263984897,
35.4645854297921,35.5470441812887,35.6295026598273,35.7119608722552,35.7944188254196,
35.8768765261672,35.959333981345,36.0417911977997,36.1278034243013,36.2111277687248,
36.2935943741702,36.3760601354117,36.4585250798642,36.5409892349401,36.623452628049,
36.7059152865976,36.7883772379904,36.870838509629,36.9532991289132,37.03575912324,
37.1182185200045,37.2006773465996,37.2831356304163,37.3655933988438,37.4480506792692,
37.5321839146807,37.6146499127723,37.6971142891278,37.77957715339,37.8620386151806,
37.9444987841018,38.0269577697373,38.1094156816546,38.1950115271793,38.2774762637794,
38.3599380357814,38.4423972816235,38.5248544396006,38.6073169578818,38.6897746287368,
38.7722334186875,38.7941824458525),.UNSPECIFIED.);
#124=B_SPLINE_CURVE_WITH_KNOTS('',3,(#10827,#10828,#10829,#10830,#10831,
#10832,#10833,#10834,#10835,#10836,#10837,#10838,#10839,#10840,#10841,#10842,
#10843,#10844,#10845,#10846,#10847,#10848,#10849,#10850,#10851,#10852,#10853,
#10854,#10855,#10856,#10857,#10858,#10859,#10860,#10861,#10862,#10863,#10864,
#10865,#10866,#10867,#10868,#10869,#10870,#10871,#10872,#10873,#10874,#10875,
#10876,#10877,#10878,#10879,#10880,#10881,#10882,#10883,#10884,#10885,#10886,
#10887,#10888,#10889,#10890,#10891,#10892,#10893,#10894,#10895,#10896,#10897,
#10898,#10899,#10900,#10901,#10902,#10903,#10904,#10905),.UNSPECIFIED.,
 .F.,.F.,(4,3,3,3,3,3,3,3,3,3,3,3,3,3,3,3,3,3,3,3,3,3,3,3,3,3,4),(32.5116015420207,
32.5889141847545,32.666183147843,32.7447814467203,32.8220229675921,32.8992702080937,
32.9765372229118,33.0561453018992,33.1335323916167,33.214250965239,33.2949695388614,
33.3717907360345,33.4485226982671,33.5251816764331,33.6017838629126,33.6783454048116,
33.755392622989,33.8319367976511,33.908491077714,33.9850700427109,34.0624833195909,
34.1391947999148,34.2169589750728,34.2947231502308,34.398883755279,34.5003194542774,
34.5575191894888),.UNSPECIFIED.);
#125=B_SPLINE_CURVE_WITH_KNOTS('',3,(#10907,#10908,#10909,#10910,#10911,
#10912,#10913,#10914,#10915,#10916,#10917,#10918,#10919,#10920,#10921,#10922,
#10923,#10924,#10925,#10926,#10927,#10928,#10929,#10930,#10931,#10932,#10933,
#10934,#10935,#10936,#10937,#10938,#10939,#10940,#10941,#10942,#10943,#10944,
#10945,#10946,#10947,#10948,#10949,#10950,#10951,#10952,#10953,#10954,#10955,
#10956,#10957,#10958,#10959,#10960,#10961,#10962,#10963,#10964,#10965,#10966,
#10967,#10968,#10969,#10970,#10971,#10972,#10973,#10974,#10975,#10976,#10977,
#10978,#10979,#10980,#10981,#10982,#10983,#10984,#10985,#10986,#10987,#10988),
 .UNSPECIFIED.,.F.,.F.,(4,3,3,3,3,3,3,3,3,3,3,3,3,3,3,3,3,3,3,3,3,3,3,3,
3,3,3,4),(32.5108171892216,32.5816010168887,32.6591291686339,32.7365760421083,
32.8139572193074,32.8912882352399,32.9685845885241,33.0458748872923,33.1231647934493,
33.2004683138543,33.2777994603781,33.3552189485883,33.4326843053928,33.5102696900783,
33.5800090249397,33.656604099681,33.7331059794936,33.8095311195445,33.8858959089002,
33.9622166853699,34.0385190780695,34.1148140336137,34.1911162890776,34.2674405842712,
34.3438449513389,34.4202916671493,34.4968502747876,34.5575191893733),
 .UNSPECIFIED.);
#126=B_SPLINE_CURVE_WITH_KNOTS('',3,(#10989,#10990,#10991,#10992,#10993,
#10994,#10995,#10996,#10997,#10998,#10999,#11000,#11001,#11002,#11003,#11004,
#11005,#11006,#11007,#11008,#11009,#11010,#11011,#11012,#11013,#11014,#11015,
#11016,#11017,#11018,#11019,#11020,#11021,#11022,#11023,#11024,#11025,#11026,
#11027,#11028,#11029,#11030,#11031,#11032,#11033,#11034,#11035,#11036,#11037,
#11038,#11039,#11040,#11041,#11042,#11043,#11044,#11045,#11046,#11047,#11048,
#11049,#11050,#11051,#11052,#11053,#11054,#11055,#11056,#11057,#11058,#11059,
#11060,#11061,#11062,#11063,#11064,#11065,#11066,#11067,#11068,#11069,#11070,
#11071,#11072,#11073,#11074,#11075,#11076,#11077,#11078,#11079,#11080,#11081,
#11082,#11083,#11084,#11085,#11086,#11087,#11088,#11089,#11090,#11091,#11092,
#11093,#11094,#11095,#11096,#11097,#11098,#11099,#11100,#11101,#11102,#11103,
#11104,#11105,#11106,#11107,#11108,#11109,#11110,#11111,#11112,#11113,#11114,
#11115,#11116,#11117,#11118,#11119,#11120,#11121,#11122,#11123,#11124,#11125,
#11126,#11127,#11128,#11129,#11130,#11131,#11132,#11133,#11134,#11135,#11136,
#11137,#11138,#11139,#11140,#11141,#11142,#11143,#11144,#11145,#11146,#11147,
#11148,#11149,#11150,#11151,#11152,#11153,#11154,#11155,#11156,#11157),
 .UNSPECIFIED.,.F.,.F.,(4,3,3,3,3,3,3,3,3,3,3,3,3,3,3,3,3,3,3,3,3,3,3,3,
3,3,3,3,3,3,3,3,3,3,3,3,3,3,3,3,3,3,3,3,3,3,3,3,3,3,3,3,3,3,3,3,4),(34.5575191894887,
34.5784170329906,34.6559472296781,34.7333903245148,34.810761958805,34.8880777226114,
34.9653531656302,35.0426140482937,35.1198693541842,35.1971331247264,35.2744194034607,
35.3517862165038,35.4291945514629,35.5067161082775,35.5768250410415,35.6543551589462,
35.7317981881018,35.8091697697655,35.886485493962,35.9637609103589,36.0410217862186,
36.1182770973981,36.1955408853225,36.2728271935386,36.3501940549771,36.4276024487411,
36.5051240814463,36.5752330490924,36.6520690812362,36.7288160969845,36.8054903345689,
36.8821079741115,36.9586851507596,37.0355546390576,37.112114741601,37.188685038769,
37.2652800998119,37.3423703391448,37.4190975357463,37.4963692964448,37.5736410571433,
37.6512357266259,37.7287379927851,37.806163477905,37.8835277493315,37.9608463304722,
38.0381420349939,38.1154270797002,38.1927154716837,38.2700212172599,38.3473992572976,
38.4248143290925,38.5023349434136,38.5720490651942,38.6535432663946,38.7349057059727,
38.7946740022541),.UNSPECIFIED.);
#127=B_SPLINE_CURVE_WITH_KNOTS('',3,(#11163,#11164,#11165,#11166,#11167,
#11168,#11169,#11170,#11171,#11172,#11173,#11174,#11175,#11176,#11177,#11178,
#11179,#11180,#11181,#11182,#11183,#11184,#11185,#11186,#11187,#11188,#11189,
#11190,#11191,#11192,#11193,#11194,#11195,#11196,#11197,#11198,#11199,#11200,
#11201,#11202,#11203,#11204,#11205,#11206,#11207,#11208,#11209,#11210,#11211,
#11212,#11213,#11214,#11215,#11216,#11217,#11218,#11219,#11220,#11221,#11222,
#11223,#11224,#11225,#11226,#11227,#11228,#11229,#11230,#11231,#11232,#11233,
#11234,#11235,#11236,#11237,#11238,#11239,#11240,#11241,#11242,#11243,#11244,
#11245,#11246,#11247,#11248,#11249,#11250,#11251,#11252,#11253,#11254,#11255,
#11256,#11257,#11258,#11259,#11260,#11261,#11262,#11263,#11264,#11265,#11266,
#11267,#11268,#11269,#11270,#11271,#11272,#11273,#11274,#11275,#11276,#11277,
#11278,#11279,#11280,#11281,#11282,#11283,#11284,#11285,#11286,#11287,#11288,
#11289,#11290,#11291,#11292,#11293,#11294,#11295,#11296,#11297,#11298,#11299,
#11300,#11301,#11302,#11303,#11304,#11305,#11306,#11307,#11308,#11309,#11310,
#11311,#11312,#11313,#11314,#11315,#11316,#11317,#11318,#11319,#11320,#11321,
#11322,#11323,#11324,#11325,#11326,#11327,#11328,#11329,#11330,#11331,#11332,
#11333,#11334),.UNSPECIFIED.,.F.,.F.,(4,3,3,3,3,3,3,3,3,3,3,3,3,3,3,3,3,
3,3,3,3,3,3,3,3,3,3,3,3,3,3,3,3,3,3,3,3,3,3,3,3,3,3,3,3,3,3,3,3,3,3,3,3,
3,3,3,3,4),(40.8407044966684,40.9226860206192,41.0048355818795,41.0872473425637,
41.169800636749,41.2525762919204,41.2929984298164,41.3705810534312,41.4480710356402,
41.5254840128659,41.6028355663674,41.680141233279,41.7574238263243,41.8346956132684,
41.9119706131257,41.9892628440641,42.0666275164294,42.1440291248622,42.2215369394709,
42.2927520411857,42.3742360141403,42.4556153782796,42.5398687454273,42.6210222405984,
42.7020989185568,42.7830843463464,42.7926288468704,42.8736372427747,42.9547214996063,
43.0391675378435,43.1204736195508,43.2018574093194,43.2833620703483,43.2925056525551,
43.3700214308182,43.4474557312288,43.5248241496561,43.6021422348063,43.6794254988508,
43.7567025831623,43.8339791636502,43.9112692590475,43.9885868930519,44.0659930993764,
44.1434451086899,44.2210179170119,44.2922592639245,44.3691208876133,44.4458862286764,
44.5247399268615,44.6013498667174,44.6779187437654,44.7544611603038,44.8309916999188,
44.9075431458621,44.9841078702885,45.0607207321892,45.0767158141578),
 .UNSPECIFIED.);
#128=B_SPLINE_CURVE_WITH_KNOTS('',3,(#11335,#11336,#11337,#11338,#11339,
#11340,#11341,#11342,#11343,#11344,#11345,#11346,#11347,#11348,#11349,#11350,
#11351,#11352,#11353,#11354,#11355,#11356,#11357,#11358,#11359,#11360,#11361,
#11362,#11363,#11364,#11365,#11366,#11367,#11368,#11369,#11370,#11371,#11372,
#11373,#11374,#11375,#11376,#11377,#11378,#11379,#11380,#11381,#11382,#11383,
#11384,#11385,#11386,#11387,#11388,#11389,#11390,#11391,#11392,#11393,#11394,
#11395,#11396,#11397,#11398,#11399,#11400,#11401,#11402,#11403,#11404,#11405,
#11406,#11407,#11408,#11409,#11410),.UNSPECIFIED.,.F.,.F.,(4,3,3,3,3,3,
3,3,3,3,3,3,3,3,3,3,3,3,3,3,3,3,3,3,3,4),(38.7941824458525,38.8766440497063,
38.9591049876769,39.0415652871625,39.1240249755595,39.2064840802615,39.2889426286607,
39.371400648147,39.4538581661086,39.5405360617686,39.6230028476043,39.7054679609481,
39.7879315114532,39.870393608751,39.9528543624523,40.0353138821495,40.1177722774172,
40.2002296578144,40.2826960440808,40.3651592460946,40.4476197023751,40.5300778512858,
40.6125434561651,40.6950033353796,40.7774674487435,40.8407044966684),
 .UNSPECIFIED.);
#129=B_SPLINE_CURVE_WITH_KNOTS('',3,(#11412,#11413,#11414,#11415,#11416,
#11417,#11418,#11419,#11420,#11421,#11422,#11423,#11424,#11425,#11426,#11427,
#11428,#11429,#11430,#11431,#11432,#11433,#11434,#11435,#11436,#11437,#11438,
#11439,#11440,#11441,#11442,#11443,#11444,#11445,#11446,#11447,#11448,#11449,
#11450,#11451,#11452,#11453,#11454,#11455,#11456,#11457,#11458,#11459,#11460,
#11461,#11462,#11463,#11464,#11465,#11466,#11467,#11468,#11469,#11470,#11471,
#11472,#11473,#11474,#11475,#11476,#11477,#11478,#11479,#11480,#11481,#11482,
#11483,#11484,#11485,#11486,#11487,#11488,#11489,#11490,#11491,#11492,#11493),
 .UNSPECIFIED.,.F.,.F.,(4,3,3,3,3,3,3,3,3,3,3,3,3,3,3,3,3,3,3,3,3,3,3,3,
3,3,3,4),(38.7946740022541,38.8758554047595,38.9569584929794,39.037964427007,
39.0712530692197,39.1522661755758,39.2333548699162,39.3176304207485,39.3989398872088,
39.4803267884912,39.5618339273282,39.5704570732452,39.6479852264478,39.7254321014026,
39.8028132801034,39.8801442975572,39.9574406523807,40.03473095271,40.1120208604414,
40.1893243824326,40.2666555305528,40.3440750203668,40.4215403787817,40.4991257650728,
40.5688650812961,40.6659056003397,40.7613323688028,40.8407044966683),
 .UNSPECIFIED.);
#130=B_SPLINE_CURVE_WITH_KNOTS('',3,(#11494,#11495,#11496,#11497,#11498,
#11499,#11500,#11501,#11502,#11503,#11504,#11505,#11506,#11507,#11508,#11509,
#11510,#11511,#11512,#11513,#11514,#11515,#11516,#11517,#11518,#11519,#11520,
#11521,#11522,#11523,#11524,#11525,#11526,#11527,#11528,#11529,#11530,#11531,
#11532,#11533,#11534,#11535,#11536,#11537,#11538,#11539,#11540,#11541,#11542,
#11543,#11544,#11545,#11546,#11547,#11548,#11549,#11550,#11551,#11552,#11553,
#11554,#11555,#11556,#11557,#11558,#11559,#11560,#11561,#11562,#11563,#11564,
#11565,#11566,#11567,#11568,#11569,#11570,#11571,#11572,#11573,#11574,#11575,
#11576,#11577,#11578,#11579,#11580,#11581,#11582,#11583,#11584,#11585,#11586,
#11587,#11588,#11589,#11590,#11591,#11592,#11593,#11594,#11595,#11596,#11597,
#11598,#11599,#11600,#11601,#11602,#11603,#11604,#11605,#11606,#11607,#11608,
#11609,#11610,#11611,#11612,#11613,#11614,#11615,#11616,#11617,#11618,#11619,
#11620,#11621,#11622,#11623,#11624,#11625,#11626,#11627,#11628,#11629,#11630,
#11631,#11632,#11633,#11634,#11635,#11636,#11637,#11638,#11639,#11640,#11641,
#11642,#11643,#11644,#11645,#11646,#11647,#11648,#11649,#11650),
 .UNSPECIFIED.,.F.,.F.,(4,3,3,3,3,3,3,3,3,3,3,3,3,3,3,3,3,3,3,3,3,3,3,3,
3,3,3,3,3,3,3,3,3,3,3,3,3,3,3,3,3,3,3,3,3,3,3,3,3,3,3,3,4),(40.8407044966683,
40.9231667027045,41.0056285604443,41.088090076738,41.1705512584355,41.2530121123868,
41.3354726454411,41.4179328644477,41.5003927762555,41.5828523877132,41.6653117056691,
41.7477707369714,41.830229488468,41.9126879670064,41.9951461794344,42.0776041325986,
42.1600618333463,42.242519288524,42.3249765049787,42.4109887314803,42.4943130759038,
42.5767796813492,42.6592454425907,42.7417103870432,42.8241745421191,42.906637935228,
42.9891005937767,43.0715625451694,43.1540238168081,43.2364844360922,43.318944430419,
43.4014038271835,43.4838626537786,43.5663209375953,43.6487787060228,43.7312359864481,
43.8153692218596,43.8978352199512,43.9802995963067,44.062762460569,44.1452239223596,
44.2276840912808,44.3101430769163,44.3926009888336,44.4781968343584,44.5606615709585,
44.6431233429604,44.7255825888025,44.8080397467795,44.8905022650607,44.9729599359157,
45.0554187258664,45.0773677530319),.UNSPECIFIED.);
#131=B_SPLINE_CURVE_WITH_KNOTS('',3,(#11656,#11657,#11658,#11659,#11660,
#11661,#11662,#11663,#11664,#11665,#11666,#11667,#11668,#11669,#11670,#11671,
#11672,#11673,#11674,#11675,#11676,#11677,#11678,#11679,#11680,#11681,#11682,
#11683,#11684,#11685,#11686,#11687,#11688,#11689,#11690,#11691,#11692,#11693,
#11694,#11695,#11696,#11697,#11698,#11699,#11700,#11701,#11702,#11703,#11704,
#11705,#11706,#11707,#11708,#11709,#11710,#11711,#11712,#11713,#11714,#11715,
#11716,#11717,#11718,#11719,#11720,#11721,#11722,#11723,#11724,#11725,#11726,
#11727,#11728,#11729,#11730,#11731,#11732,#11733,#11734,#11735,#11736,#11737,
#11738,#11739,#11740,#11741,#11742,#11743,#11744,#11745,#11746,#11747,#11748,
#11749,#11750,#11751,#11752,#11753,#11754,#11755,#11756,#11757,#11758,#11759,
#11760,#11761,#11762,#11763,#11764,#11765,#11766,#11767,#11768,#11769,#11770,
#11771,#11772,#11773,#11774,#11775,#11776,#11777,#11778,#11779,#11780,#11781,
#11782,#11783,#11784,#11785,#11786,#11787,#11788,#11789,#11790,#11791,#11792,
#11793,#11794,#11795,#11796,#11797,#11798,#11799,#11800,#11801,#11802,#11803,
#11804,#11805,#11806,#11807,#11808,#11809,#11810,#11811,#11812,#11813,#11814,
#11815,#11816,#11817,#11818,#11819,#11820,#11821,#11822,#11823,#11824),
 .UNSPECIFIED.,.F.,.F.,(4,3,3,3,3,3,3,3,3,3,3,3,3,3,3,3,3,3,3,3,3,3,3,3,
3,3,3,3,3,3,3,3,3,3,3,3,3,3,3,3,3,3,3,3,3,3,3,3,3,3,3,3,3,3,3,3,4),(47.123889803848,
47.2517194303792,47.2915200980326,47.3683412951874,47.4450732574017,47.5217322355495,
47.5983344220109,47.6748959638918,47.7519431820806,47.8284873567249,47.9050416367702,
47.9816206017498,48.0590338786628,48.1357453589698,48.2135095341858,48.2912737094019,
48.3688563330162,48.4463463152247,48.5237592924499,48.601110845951,48.6784165128622,
48.7556991059071,48.8329708928507,48.9102458927076,48.9875381236454,49.0649027960103,
49.1423044044427,49.2198122190509,49.2910273207713,49.3725112937265,49.4538906578663,
49.5381440250137,49.6192975201854,49.7003741981444,49.7813596259345,49.790904126456,
49.8719125223601,49.9529967791915,50.0374428174288,50.1187488991358,50.2001326889043,
50.2816373499328,50.2907809321407,50.3682967104038,50.4457310108144,50.5230994292416,
50.6004175143919,50.6777007784363,50.7549778627479,50.8322544432357,50.9095445386331,
50.9868621726374,51.0642683789619,51.1417203882753,51.2192931965973,51.29053454351,
51.3611629585881),.UNSPECIFIED.);
#132=B_SPLINE_CURVE_WITH_KNOTS('',3,(#11825,#11826,#11827,#11828,#11829,
#11830,#11831,#11832,#11833,#11834,#11835,#11836,#11837,#11838,#11839,#11840,
#11841,#11842,#11843,#11844,#11845,#11846,#11847,#11848,#11849,#11850,#11851,
#11852,#11853,#11854,#11855,#11856,#11857,#11858,#11859,#11860,#11861,#11862,
#11863,#11864,#11865,#11866,#11867,#11868,#11869,#11870,#11871,#11872,#11873,
#11874,#11875,#11876,#11877,#11878,#11879,#11880,#11881,#11882,#11883,#11884,
#11885,#11886,#11887,#11888,#11889,#11890,#11891,#11892,#11893,#11894,#11895,
#11896,#11897,#11898,#11899,#11900,#11901,#11902,#11903,#11904,#11905,#11906),
 .UNSPECIFIED.,.F.,.F.,(4,3,3,3,3,3,3,3,3,3,3,3,3,3,3,3,3,3,3,3,3,3,3,3,
3,3,3,4),(45.0767158141578,45.1534176377557,45.2302334351738,45.2920128752938,
45.3695304269119,45.4469606463314,45.5243191892268,45.6016216598141,45.6788836217642,
45.7561308475469,45.8333723587542,45.910622208987,45.9878944538999,46.0652474118709,
46.1426418041797,46.2201501318482,46.2917664866632,46.3680381413798,46.4442228719431,
46.5203373350376,46.5963945826144,46.6724205164471,46.7484300824388,46.8244382133086,
46.9004926659308,46.976569510054,47.0527320234986,47.1238898037382),
 .UNSPECIFIED.);
#133=B_SPLINE_CURVE_WITH_KNOTS('',3,(#11908,#11909,#11910,#11911,#11912,
#11913,#11914,#11915,#11916,#11917,#11918,#11919,#11920,#11921,#11922,#11923,
#11924,#11925,#11926,#11927,#11928,#11929,#11930,#11931,#11932,#11933,#11934,
#11935,#11936,#11937,#11938,#11939,#11940,#11941,#11942,#11943,#11944,#11945,
#11946,#11947,#11948,#11949,#11950,#11951,#11952,#11953,#11954,#11955,#11956,
#11957,#11958,#11959,#11960,#11961,#11962,#11963,#11964,#11965,#11966,#11967,
#11968,#11969,#11970,#11971,#11972,#11973,#11974,#11975,#11976,#11977,#11978,
#11979,#11980,#11981,#11982,#11983),.UNSPECIFIED.,.F.,.F.,(4,3,3,3,3,3,
3,3,3,3,3,3,3,3,3,3,3,3,3,3,3,3,3,3,3,4),(45.0773677530319,45.1598293568857,
45.2422902948563,45.3247505943419,45.4072102827389,45.4896693874409,45.5721279358401,
45.6545859553264,45.7370434732879,45.8237213689479,45.9061881547836,45.9886532681274,
46.0711168186325,46.1535789159302,46.2360396696316,46.3184991893287,46.4009575845963,
46.4834149649933,46.5658813512597,46.6483445532735,46.7308050095539,46.8132631584647,
46.895728763344,46.9781886425586,47.0606527559224,47.1238898038478),
 .UNSPECIFIED.);
#134=B_SPLINE_CURVE_WITH_KNOTS('',3,(#11984,#11985,#11986,#11987,#11988,
#11989,#11990,#11991,#11992,#11993,#11994,#11995,#11996,#11997,#11998,#11999,
#12000,#12001,#12002,#12003,#12004,#12005,#12006,#12007,#12008,#12009,#12010,
#12011,#12012,#12013,#12014,#12015,#12016,#12017,#12018,#12019,#12020,#12021,
#12022,#12023,#12024,#12025,#12026,#12027,#12028,#12029,#12030,#12031,#12032,
#12033,#12034,#12035,#12036,#12037,#12038,#12039,#12040,#12041,#12042,#12043,
#12044,#12045,#12046,#12047,#12048,#12049,#12050,#12051,#12052,#12053,#12054,
#12055,#12056,#12057,#12058,#12059,#12060,#12061,#12062,#12063,#12064,#12065,
#12066,#12067,#12068,#12069,#12070,#12071,#12072,#12073,#12074,#12075,#12076,
#12077,#12078,#12079,#12080,#12081,#12082,#12083,#12084,#12085,#12086,#12087,
#12088,#12089,#12090,#12091,#12092,#12093,#12094,#12095,#12096,#12097,#12098,
#12099,#12100,#12101,#12102,#12103,#12104,#12105,#12106,#12107,#12108,#12109,
#12110,#12111,#12112,#12113,#12114,#12115,#12116,#12117,#12118,#12119,#12120,
#12121,#12122,#12123,#12124,#12125,#12126,#12127,#12128,#12129,#12130,#12131,
#12132,#12133,#12134,#12135,#12136,#12137,#12138,#12139,#12140,#12141,#12142,
#12143,#12144,#12145,#12146,#12147,#12148,#12149),.UNSPECIFIED.,.F.,.F.,
(4,3,3,3,3,3,3,3,3,3,3,3,3,3,3,3,3,3,3,3,3,3,3,3,3,3,3,3,3,3,3,3,3,3,3,
3,3,3,3,3,3,3,3,3,3,3,3,3,3,3,3,3,3,3,3,4),(47.1238898038478,47.2087594582049,
47.2959998780668,47.3815228915232,47.4696220145879,47.5577211376525,47.6345845223047,
47.7113543541143,47.7880468901028,47.8646783252696,47.941264806053,48.0181228485093,
48.0946811714726,48.171245506145,48.2478304192723,48.32490510088,48.4016119217489,
48.4788705337262,48.5561291457034,48.6336593421632,48.7111024367686,48.7884740708243,
48.865789834393,48.9430652771715,49.0203261595911,49.0975814652355,49.1748452355298,
49.2521315140141,49.3294983268062,49.4069066615132,49.4844282180761,49.5545371537543,
49.6320672718176,49.7095103011336,49.7868818829591,49.8641976073189,49.9414730238803,
50.0187338999058,50.095989211252,50.1732529993437,50.2505393077278,50.327906169334,
50.4053145632661,50.482836196138,50.5529451618052,50.6297918919989,50.7065473799042,
50.7832278737467,50.8598420747927,50.9364195440692,51.0129748672405,51.0895226140708,
51.166100998141,51.2426961532365,51.3193532626057,51.3596845371041),
 .UNSPECIFIED.);
#135=B_SPLINE_CURVE_WITH_KNOTS('',3,(#12155,#12156,#12157,#12158,#12159,
#12160,#12161,#12162,#12163,#12164,#12165,#12166,#12167,#12168,#12169,#12170,
#12171,#12172,#12173,#12174,#12175,#12176,#12177,#12178,#12179,#12180,#12181,
#12182,#12183,#12184,#12185,#12186,#12187,#12188,#12189,#12190,#12191,#12192,
#12193,#12194,#12195,#12196,#12197,#12198,#12199,#12200,#12201,#12202,#12203,
#12204,#12205,#12206,#12207,#12208,#12209,#12210,#12211,#12212,#12213,#12214,
#12215,#12216,#12217,#12218,#12219,#12220,#12221,#12222,#12223,#12224,#12225,
#12226,#12227,#12228,#12229,#12230,#12231,#12232,#12233,#12234,#12235,#12236,
#12237,#12238,#12239,#12240,#12241,#12242,#12243,#12244,#12245,#12246,#12247,
#12248,#12249,#12250,#12251,#12252,#12253,#12254,#12255,#12256,#12257,#12258,
#12259,#12260,#12261,#12262,#12263,#12264,#12265,#12266,#12267,#12268,#12269,
#12270,#12271,#12272,#12273,#12274,#12275,#12276,#12277,#12278,#12279,#12280,
#12281,#12282,#12283,#12284,#12285,#12286,#12287,#12288,#12289,#12290,#12291,
#12292,#12293,#12294,#12295,#12296,#12297,#12298,#12299,#12300,#12301,#12302,
#12303,#12304,#12305,#12306,#12307,#12308,#12309,#12310,#12311,#12312,#12313,
#12314,#12315,#12316,#12317,#12318,#12319,#12320,#12321,#12322,#12323,#12324,
#12325,#12326),.UNSPECIFIED.,.F.,.F.,(4,3,3,3,3,3,3,3,3,3,3,3,3,3,3,3,3,
3,3,3,3,3,3,3,3,3,3,3,3,3,3,3,3,3,3,3,3,3,3,3,3,3,3,3,3,3,3,3,3,3,3,3,3,
3,3,3,3,4),(53.4070751111438,53.4835343669011,53.5599178969044,53.63624215006,
53.7125235237776,53.7887875517728,53.8650452206851,53.941311322949,54.0176006546155,
54.0939682612546,54.1703794615919,54.2468951712867,54.2897953776181,54.3666165747729,
54.4433485369872,54.5200075151348,54.5966097015961,54.6731712434767,54.7502184616656,
54.8267626363099,54.9033169163554,54.9798958813348,55.057309158248,55.134020638555,
55.2117848137712,55.2895489889875,55.3671316126018,55.4446215948104,55.5220345720357,
55.5993861255369,55.6766917924485,55.7539743854934,55.8312461724371,55.9085211722938,
55.9858134032314,56.0631780755963,56.1405796840288,56.2180874986371,56.2893026003569,
56.3707865733119,56.4521659374517,56.5364193045992,56.6175727997706,56.6986494777297,
56.7796349055199,56.7891794060416,56.8701878019459,56.9512720587777,57.0357180970148,
57.1170241787221,57.1984079684906,57.2799126295192,57.2890562117262,57.36658694434,
57.4440154159151,57.5213849283417,57.5987011855334,57.6440769298056),
 .UNSPECIFIED.);
#136=B_SPLINE_CURVE_WITH_KNOTS('',3,(#12327,#12328,#12329,#12330,#12331,
#12332,#12333,#12334,#12335,#12336,#12337,#12338,#12339,#12340,#12341,#12342,
#12343,#12344,#12345,#12346,#12347,#12348,#12349,#12350,#12351,#12352,#12353,
#12354,#12355,#12356,#12357,#12358,#12359,#12360,#12361,#12362,#12363,#12364,
#12365,#12366,#12367,#12368,#12369,#12370,#12371,#12372,#12373,#12374,#12375,
#12376,#12377,#12378,#12379,#12380,#12381,#12382,#12383,#12384,#12385,#12386,
#12387,#12388,#12389,#12390,#12391,#12392,#12393,#12394,#12395,#12396,#12397,
#12398,#12399,#12400,#12401,#12402,#12403,#12404,#12405),.UNSPECIFIED.,
 .F.,.F.,(4,3,3,3,3,3,3,3,3,3,3,3,3,3,3,3,3,3,3,3,3,3,3,3,3,3,4),(51.3611629585881,
51.437924793484,51.5146078062219,51.5912282087005,51.6678021628812,51.7456129118809,
51.8221554642554,51.8987029014922,51.9752698002357,52.0540243888966,52.1307129766142,
52.2105005657468,52.2902881548794,52.3678057064975,52.445235925917,52.5225944688125,
52.5998969393998,52.6771589013499,52.7544061271325,52.8316476383397,52.9088974885726,
52.9861697334856,53.0635226914566,53.1409170837653,53.2184254114338,53.2900417662488,
53.4070751110276),.UNSPECIFIED.);
#137=B_SPLINE_CURVE_WITH_KNOTS('',3,(#12407,#12408,#12409,#12410,#12411,
#12412,#12413,#12414,#12415,#12416,#12417,#12418,#12419,#12420,#12421,#12422,
#12423,#12424,#12425,#12426,#12427,#12428,#12429,#12430,#12431,#12432,#12433,
#12434,#12435,#12436,#12437,#12438,#12439,#12440,#12441,#12442,#12443,#12444,
#12445,#12446,#12447,#12448,#12449,#12450,#12451,#12452,#12453,#12454,#12455,
#12456,#12457,#12458,#12459,#12460,#12461,#12462,#12463,#12464,#12465,#12466,
#12467,#12468,#12469,#12470,#12471,#12472,#12473,#12474,#12475,#12476,#12477,
#12478,#12479,#12480,#12481,#12482,#12483,#12484,#12485,#12486,#12487,#12488,
#12489,#12490,#12491),.UNSPECIFIED.,.F.,.F.,(4,3,3,3,3,3,3,3,3,3,3,3,3,
3,3,3,3,3,3,3,3,3,3,3,3,3,3,3,4),(51.3596845371041,51.4364397650722,51.5133076851397,
51.5513531698562,51.6289478392903,51.7064501054006,51.7838755904712,51.8612398618481,
51.938558442939,52.0158541474106,52.0931391920665,52.1704275839996,52.2477333295252,
52.3251113695126,52.4025264412572,52.4800470555284,52.5497611779071,52.63124749234,
52.7126295746991,52.7967134765075,52.8778707953606,52.958951579115,53.0399415711485,
53.0489651819325,53.1255961689623,53.202287407139,53.2790111285547,53.3558252447557,
53.4065880026861),.UNSPECIFIED.);
#138=B_SPLINE_CURVE_WITH_KNOTS('',3,(#12492,#12493,#12494,#12495,#12496,
#12497,#12498,#12499,#12500,#12501,#12502,#12503,#12504,#12505,#12506,#12507,
#12508,#12509,#12510,#12511,#12512,#12513,#12514,#12515,#12516,#12517,#12518,
#12519,#12520,#12521,#12522,#12523,#12524,#12525,#12526,#12527,#12528,#12529,
#12530,#12531,#12532,#12533,#12534,#12535,#12536,#12537,#12538,#12539,#12540,
#12541,#12542,#12543,#12544,#12545,#12546,#12547,#12548,#12549,#12550,#12551,
#12552,#12553,#12554,#12555,#12556,#12557,#12558,#12559,#12560,#12561,#12562,
#12563,#12564,#12565,#12566,#12567,#12568,#12569,#12570,#12571,#12572,#12573,
#12574,#12575,#12576,#12577,#12578,#12579,#12580,#12581,#12582,#12583,#12584,
#12585,#12586,#12587,#12588,#12589,#12590,#12591,#12592,#12593,#12594,#12595,
#12596,#12597,#12598,#12599,#12600,#12601,#12602,#12603,#12604,#12605,#12606,
#12607,#12608,#12609,#12610,#12611,#12612,#12613,#12614,#12615,#12616,#12617,
#12618,#12619,#12620,#12621,#12622,#12623,#12624,#12625,#12626,#12627,#12628,
#12629,#12630,#12631,#12632,#12633,#12634,#12635,#12636,#12637,#12638,#12639,
#12640,#12641,#12642,#12643,#12644,#12645,#12646,#12647,#12648),
 .UNSPECIFIED.,.F.,.F.,(4,3,3,3,3,3,3,3,3,3,3,3,3,3,3,3,3,3,3,3,3,3,3,3,
3,3,3,3,3,3,3,3,3,3,3,3,3,3,3,3,3,3,3,3,3,3,3,3,3,3,3,3,4),(53.4070751110274,
53.4895373170636,53.5719991748034,53.6544606910971,53.7369218727946,53.8193827267458,
53.9018432598001,53.9843034788068,54.0667633906146,54.1492230020723,54.2316823200283,
54.3141413513307,54.3966001028272,54.4790585813658,54.5615167937936,54.6439747469578,
54.7264324477054,54.8088899028833,54.8913471193378,54.9773593458395,55.0606836902629,
55.1431502957084,55.2256160569498,55.3080810014024,55.3905451564784,55.4730085495872,
55.5554712081358,55.6379331595286,55.7203944311673,55.8028550504514,55.8853150447782,
55.9677744415428,56.0502332681379,56.1326915519547,56.215149320382,56.2976066008073,
56.3817398362188,56.4642058343104,56.5466702106659,56.6291330749281,56.7115945367188,
56.7940547056399,56.8765136912755,56.9589716031927,57.0445674487175,57.1270321853176,
57.2094939573196,57.2919532031617,57.3744103611388,57.45687287942,57.539330550275,
57.6217893402258,57.6437383673911),.UNSPECIFIED.);
#139=B_SPLINE_CURVE_WITH_KNOTS('',3,(#12654,#12655,#12656,#12657,#12658,
#12659,#12660,#12661,#12662,#12663,#12664,#12665,#12666,#12667,#12668,#12669,
#12670,#12671,#12672,#12673,#12674,#12675,#12676,#12677,#12678,#12679,#12680,
#12681,#12682,#12683,#12684,#12685,#12686,#12687,#12688,#12689,#12690,#12691,
#12692,#12693,#12694,#12695,#12696,#12697,#12698,#12699,#12700,#12701,#12702,
#12703,#12704,#12705,#12706,#12707,#12708,#12709,#12710,#12711,#12712,#12713,
#12714,#12715,#12716,#12717,#12718,#12719,#12720,#12721,#12722,#12723,#12724,
#12725,#12726,#12727,#12728,#12729,#12730,#12731,#12732,#12733,#12734,#12735,
#12736,#12737,#12738,#12739,#12740,#12741,#12742,#12743,#12744,#12745,#12746,
#12747,#12748,#12749,#12750,#12751,#12752,#12753,#12754,#12755,#12756,#12757,
#12758,#12759,#12760,#12761,#12762,#12763,#12764,#12765,#12766,#12767,#12768,
#12769,#12770,#12771,#12772,#12773,#12774,#12775,#12776,#12777,#12778,#12779,
#12780,#12781,#12782,#12783,#12784,#12785,#12786,#12787,#12788,#12789,#12790,
#12791,#12792,#12793,#12794,#12795,#12796,#12797,#12798,#12799,#12800,#12801,
#12802,#12803,#12804,#12805,#12806,#12807,#12808,#12809,#12810),
 .UNSPECIFIED.,.F.,.F.,(4,3,3,3,3,3,3,3,3,3,3,3,3,3,3,3,3,3,3,3,3,3,3,3,
3,3,3,3,3,3,3,3,3,3,3,3,3,3,3,3,3,3,3,3,3,3,3,3,3,3,3,3,4),(59.6902604182072,
59.7727226242434,59.8551844819832,59.9376459982768,60.0201071799743,60.1025680339255,
60.1850285669798,60.2674887859865,60.3499486977942,60.4324083092519,60.514867627208,
60.5973266585102,60.6797854100069,60.7622438885454,60.8447021009733,60.9271600541376,
61.0096177548854,61.0920752100632,61.1745324265176,61.2605446530193,61.3438689974428,
61.4263356028882,61.5088013641297,61.5912663085822,61.6737304636581,61.756193856767,
61.8386565153156,61.9211184667083,62.003579738347,62.0860403576312,62.168500351958,
62.2509597487226,62.3334185753177,62.4158768591345,62.4983346275619,62.5807919079872,
62.6649251433987,62.7473911414903,62.8298555178458,62.912318382108,62.9947798438987,
63.0772400128198,63.1596989984554,63.2421569103726,63.3277527558974,63.4102174924975,
63.4926792644995,63.5751385103415,63.6575956683186,63.7400581865999,63.822515857455,
63.9049746474057,63.9269236745709),.UNSPECIFIED.);
#140=B_SPLINE_CURVE_WITH_KNOTS('',3,(#12811,#12812,#12813,#12814,#12815,
#12816,#12817,#12818,#12819,#12820,#12821,#12822,#12823,#12824,#12825,#12826,
#12827,#12828,#12829,#12830,#12831,#12832,#12833,#12834,#12835,#12836,#12837,
#12838,#12839,#12840,#12841,#12842,#12843,#12844,#12845,#12846,#12847,#12848,
#12849,#12850,#12851,#12852,#12853,#12854,#12855,#12856,#12857,#12858,#12859,
#12860,#12861,#12862,#12863,#12864,#12865,#12866,#12867,#12868,#12869,#12870,
#12871,#12872,#12873,#12874,#12875,#12876,#12877,#12878,#12879,#12880,#12881,
#12882,#12883,#12884,#12885,#12886,#12887,#12888,#12889,#12890,#12891,#12892),
 .UNSPECIFIED.,.F.,.F.,(4,3,3,3,3,3,3,3,3,3,3,3,3,3,3,3,3,3,3,3,3,3,3,3,
3,3,3,4),(57.6440769298056,57.7246685414669,57.8019436746278,57.8792271368914,
57.9565329492142,58.0338751424344,58.1113087178789,58.1887960545296,58.2663905274488,
58.2888098230956,58.3656584462832,58.4424132926799,58.5190906320844,58.5957066718592,
58.6722775704842,58.7493133034818,58.8258557221875,58.90240405875,58.9789728901979,
59.0563705262647,59.1330616072173,59.2108125208412,59.288563434465,59.3753375230801,
59.4617551097612,59.5479378979409,59.6337172903819,59.6902604182072),
 .UNSPECIFIED.);
#141=B_SPLINE_CURVE_WITH_KNOTS('',3,(#12894,#12895,#12896,#12897,#12898,
#12899,#12900,#12901,#12902,#12903,#12904,#12905,#12906,#12907,#12908,#12909,
#12910,#12911,#12912,#12913,#12914,#12915,#12916,#12917,#12918,#12919,#12920,
#12921,#12922,#12923,#12924,#12925,#12926,#12927,#12928,#12929,#12930,#12931,
#12932,#12933,#12934,#12935,#12936,#12937,#12938,#12939,#12940,#12941,#12942,
#12943,#12944,#12945,#12946,#12947,#12948,#12949,#12950,#12951,#12952,#12953,
#12954,#12955,#12956,#12957,#12958,#12959,#12960,#12961,#12962,#12963,#12964,
#12965,#12966,#12967,#12968,#12969),.UNSPECIFIED.,.F.,.F.,(4,3,3,3,3,3,
3,3,3,3,3,3,3,3,3,3,3,3,3,3,3,3,3,3,3,4),(57.6437383673911,57.7261999712449,
57.8086609092155,57.8911212087012,57.973580897098,58.0560400018002,58.1384985501993,
58.2209565696855,58.3034140876471,58.3900919833071,58.4725587691428,58.5550238824865,
58.6374874329917,58.7199495302894,58.8024102839909,58.884869803688,58.9673281989556,
59.0497855793529,59.1322519656194,59.2147151676331,59.2971756239135,59.3796337728243,
59.4620993777036,59.5445592569181,59.627023370282,59.690260418207),
 .UNSPECIFIED.);
#142=B_SPLINE_CURVE_WITH_KNOTS('',3,(#12970,#12971,#12972,#12973,#12974,
#12975,#12976,#12977,#12978,#12979,#12980,#12981,#12982,#12983,#12984,#12985,
#12986,#12987,#12988,#12989,#12990,#12991,#12992,#12993,#12994,#12995,#12996,
#12997,#12998,#12999,#13000,#13001,#13002,#13003,#13004,#13005,#13006,#13007,
#13008,#13009,#13010,#13011,#13012,#13013,#13014,#13015,#13016,#13017,#13018,
#13019,#13020,#13021,#13022,#13023,#13024,#13025,#13026,#13027,#13028,#13029,
#13030,#13031,#13032,#13033,#13034,#13035,#13036,#13037,#13038,#13039,#13040,
#13041,#13042,#13043,#13044,#13045,#13046,#13047,#13048,#13049,#13050,#13051,
#13052,#13053,#13054,#13055,#13056,#13057,#13058,#13059,#13060,#13061,#13062,
#13063,#13064,#13065,#13066,#13067,#13068,#13069,#13070,#13071,#13072,#13073,
#13074,#13075,#13076,#13077,#13078,#13079,#13080,#13081,#13082,#13083,#13084,
#13085,#13086,#13087,#13088,#13089,#13090,#13091,#13092,#13093,#13094,#13095,
#13096,#13097,#13098,#13099,#13100,#13101,#13102,#13103,#13104,#13105,#13106,
#13107,#13108,#13109,#13110,#13111,#13112,#13113,#13114,#13115,#13116,#13117,
#13118,#13119,#13120,#13121,#13122,#13123,#13124,#13125,#13126,#13127,#13128,
#13129,#13130,#13131,#13132,#13133,#13134,#13135,#13136,#13137,#13138),
 .UNSPECIFIED.,.F.,.F.,(4,3,3,3,3,3,3,3,3,3,3,3,3,3,3,3,3,3,3,3,3,3,3,3,
3,3,3,3,3,3,3,3,3,3,3,3,3,3,3,3,3,3,3,3,3,3,3,3,3,3,3,3,3,3,3,3,4),(59.690777377404,
59.7673619185021,59.8438612447857,59.9203113702036,59.9967242576866,60.037821238289,
60.1188343445795,60.1999230388526,60.284198589718,60.3655080561077,60.4468949573183,
60.5284020960833,60.5370252423144,60.6145533955236,60.6920002704849,60.7693814491924,
60.8467124666531,60.9240088214836,61.0012991218198,61.0785890295582,61.1558925515562,
61.2332236996835,61.3106431895045,61.3881085479264,61.4656939342244,61.5354332503653,
61.6122966350176,61.6890664668272,61.7657590028159,61.8423904379825,61.918976918766,
61.9958349612223,62.0723932841857,62.1489576188581,62.2255425319854,62.3026172135931,
62.379324034462,62.4565826464392,62.5338412584163,62.6113714548761,62.6888145494816,
62.7661861835372,62.8435019471059,62.9207773898842,62.9980382723037,63.075293577948,
63.1525573482421,63.2298436267263,63.3072104395184,63.3846187742254,63.4621403307883,
63.5322492664672,63.6097908036147,63.6891614337623,63.7665285349367,63.8469009295709,
63.9272733242051),.UNSPECIFIED.);
#143=B_SPLINE_CURVE_WITH_KNOTS('',3,(#13144,#13145,#13146,#13147,#13148,
#13149,#13150,#13151,#13152,#13153,#13154,#13155,#13156,#13157,#13158,#13159,
#13160,#13161,#13162,#13163,#13164,#13165,#13166,#13167,#13168,#13169,#13170,
#13171,#13172,#13173,#13174,#13175,#13176,#13177,#13178,#13179,#13180,#13181,
#13182,#13183,#13184,#13185,#13186,#13187,#13188,#13189,#13190,#13191,#13192,
#13193,#13194,#13195,#13196,#13197,#13198,#13199,#13200,#13201,#13202,#13203,
#13204,#13205,#13206,#13207,#13208,#13209,#13210,#13211,#13212,#13213,#13214,
#13215,#13216,#13217,#13218,#13219,#13220,#13221,#13222,#13223,#13224,#13225,
#13226,#13227,#13228,#13229,#13230,#13231,#13232,#13233,#13234,#13235,#13236,
#13237,#13238,#13239,#13240,#13241,#13242,#13243,#13244,#13245,#13246,#13247,
#13248,#13249,#13250,#13251,#13252,#13253,#13254,#13255,#13256,#13257,#13258,
#13259,#13260,#13261,#13262,#13263,#13264,#13265,#13266,#13267,#13268,#13269,
#13270,#13271,#13272,#13273,#13274,#13275,#13276,#13277,#13278,#13279,#13280,
#13281,#13282,#13283,#13284,#13285,#13286,#13287,#13288,#13289,#13290,#13291,
#13292,#13293,#13294,#13295,#13296,#13297,#13298,#13299,#13300,#13301,#13302,
#13303,#13304,#13305,#13306,#13307,#13308,#13309),.UNSPECIFIED.,.F.,.F.,
(4,3,3,3,3,3,3,3,3,3,3,3,3,3,3,3,3,3,3,3,3,3,3,3,3,3,3,3,3,3,3,3,3,3,3,
3,3,3,3,3,3,3,3,3,3,3,3,3,3,3,3,3,3,3,3,4),(65.9734457253868,66.0640275444732,
66.1552001016788,66.2470822494204,66.2868387140505,66.3643562656686,66.4417864850882,
66.5191450279837,66.596447498571,66.6737094605213,66.750956686304,66.8281981975113,
66.905448047744,66.9827202926568,67.0600732506278,67.1374676429365,67.214975970605,
67.2865923254199,67.364109694616,67.4415397620673,67.518898183337,67.5962005625517,
67.6734624633146,67.7507096740056,67.8279511982241,67.9052010895703,67.9824734037138,
68.0598264749397,68.1372210046912,68.2147295096535,68.2863459367893,68.3631671339441,
68.4398990961584,68.5165580743062,68.5931602607676,68.6697218026485,68.7467690208373,
68.8233131954816,68.8998674755269,68.9764464405066,69.0538597174196,69.1305711977265,
69.2083353729425,69.2860995481586,69.3636865021404,69.4411799732403,69.518595601332,
69.5959489704174,69.6732543422776,69.7505336933602,69.8278010512468,69.9050704341445,
69.9823887172598,70.0597308627986,70.1371583399476,70.2096877536336),
 .UNSPECIFIED.);
#144=B_SPLINE_CURVE_WITH_KNOTS('',3,(#13310,#13311,#13312,#13313,#13314,
#13315,#13316,#13317,#13318,#13319,#13320,#13321,#13322,#13323,#13324,#13325,
#13326,#13327,#13328,#13329,#13330,#13331,#13332,#13333,#13334,#13335,#13336,
#13337,#13338,#13339,#13340,#13341,#13342,#13343,#13344,#13345,#13346,#13347,
#13348,#13349,#13350,#13351,#13352,#13353,#13354,#13355,#13356,#13357,#13358,
#13359,#13360,#13361,#13362,#13363,#13364,#13365,#13366,#13367,#13368,#13369,
#13370,#13371,#13372,#13373,#13374,#13375,#13376,#13377,#13378,#13379,#13380,
#13381,#13382,#13383,#13384,#13385),.UNSPECIFIED.,.F.,.F.,(4,3,3,3,3,3,
3,3,3,3,3,3,3,3,3,3,3,3,3,3,3,3,3,3,3,4),(63.9269236745709,64.0093852784247,
64.0918462163953,64.1743065158809,64.2567662042778,64.3392253089798,64.421683857379,
64.5041418768653,64.5865993948268,64.6732772904868,64.7557440763225,64.8382091896663,
64.9206727401714,65.0031348374692,65.0855955911706,65.1680551108677,65.2505135061353,
65.3329708865325,65.415437272799,65.4979004748128,65.5803609310932,65.6628190800038,
65.7452846848831,65.8277445640976,65.9102086774615,65.9734457253868),
 .UNSPECIFIED.);
#145=B_SPLINE_CURVE_WITH_KNOTS('',3,(#13387,#13388,#13389,#13390,#13391,
#13392,#13393,#13394,#13395,#13396,#13397,#13398,#13399,#13400,#13401,#13402,
#13403,#13404,#13405,#13406,#13407,#13408,#13409,#13410,#13411,#13412,#13413,
#13414,#13415,#13416,#13417,#13418,#13419,#13420,#13421,#13422,#13423,#13424,
#13425,#13426,#13427,#13428,#13429,#13430,#13431,#13432,#13433,#13434,#13435,
#13436,#13437,#13438,#13439,#13440,#13441,#13442,#13443,#13444,#13445,#13446,
#13447,#13448,#13449,#13450,#13451,#13452,#13453,#13454,#13455,#13456,#13457,
#13458,#13459,#13460,#13461,#13462,#13463,#13464,#13465,#13466,#13467,#13468),
 .UNSPECIFIED.,.F.,.F.,(4,3,3,3,3,3,3,3,3,3,3,3,3,3,3,3,3,3,3,3,3,3,3,3,
3,3,3,4),(63.9272733242051,64.0045329596442,64.0817885003611,64.1590539876398,
64.2363434656992,64.3137140801567,64.3911275495765,64.4686520662923,64.5306572745181,
64.6074933066408,64.6842403223678,64.7609145599314,64.8375321994535,64.9141093760802,
64.9909788643913,65.0675389669138,65.144109264061,65.2207043250835,65.2977945644549,
65.3745217610364,65.4517935218027,65.529065282569,65.6144079592789,65.6995528569604,
65.7843842943116,65.8690119703541,65.9533377016775,65.9734457253866),
 .UNSPECIFIED.);
#146=B_SPLINE_CURVE_WITH_KNOTS('',3,(#13469,#13470,#13471,#13472,#13473,
#13474,#13475,#13476,#13477,#13478,#13479,#13480,#13481,#13482,#13483,#13484,
#13485,#13486,#13487,#13488,#13489,#13490,#13491,#13492,#13493,#13494,#13495,
#13496,#13497,#13498,#13499,#13500,#13501,#13502,#13503,#13504,#13505,#13506,
#13507,#13508,#13509,#13510,#13511,#13512,#13513,#13514,#13515,#13516,#13517,
#13518,#13519,#13520,#13521,#13522,#13523,#13524,#13525,#13526,#13527,#13528,
#13529,#13530,#13531,#13532,#13533,#13534,#13535,#13536,#13537,#13538,#13539,
#13540,#13541,#13542,#13543,#13544,#13545,#13546,#13547,#13548,#13549,#13550,
#13551,#13552,#13553,#13554,#13555,#13556,#13557,#13558,#13559,#13560,#13561,
#13562,#13563,#13564,#13565,#13566,#13567,#13568,#13569,#13570,#13571,#13572,
#13573,#13574,#13575,#13576,#13577,#13578,#13579,#13580,#13581,#13582,#13583,
#13584,#13585,#13586,#13587,#13588,#13589,#13590,#13591,#13592,#13593,#13594,
#13595,#13596,#13597,#13598,#13599,#13600,#13601,#13602,#13603,#13604,#13605,
#13606,#13607,#13608,#13609,#13610,#13611,#13612,#13613,#13614,#13615,#13616,
#13617,#13618,#13619,#13620,#13621,#13622,#13623,#13624,#13625),
 .UNSPECIFIED.,.F.,.F.,(4,3,3,3,3,3,3,3,3,3,3,3,3,3,3,3,3,3,3,3,3,3,3,3,
3,3,3,3,3,3,3,3,3,3,3,3,3,3,3,3,3,3,3,3,3,3,3,3,3,3,3,3,4),(65.9734457253866,
66.0559079314229,66.1383697891626,66.2208313054562,66.3032924871537,66.3857533411049,
66.4682138741592,66.5506740931658,66.6331340049737,66.7155936164313,66.7980529343874,
66.8805119656898,66.9629707171864,67.0454291957249,67.1278874081526,67.2103453613168,
67.2928030620647,67.3752605172425,67.457717733697,67.5437299601987,67.6270543046221,
67.7095209100676,67.7919866713091,67.8744516157616,67.9569157708375,68.0393791639464,
68.121841822495,68.2043037738878,68.2867650455265,68.3692256648107,68.4516856591375,
68.534145055902,68.6166038824972,68.6990621663138,68.7815199347413,68.8639772151668,
68.9481104505782,69.0305764486698,69.1130408250253,69.1955036892875,69.2779651510782,
69.3604253199993,69.4428843056349,69.5253422175521,69.6109380630769,69.693402799677,
69.775864571679,69.8583238175211,69.9407809754981,70.0232434937793,70.1057011646343,
70.188159954585,70.2101089817503),.UNSPECIFIED.);
#147=B_SPLINE_CURVE_WITH_KNOTS('',3,(#13631,#13632,#13633,#13634,#13635,
#13636,#13637,#13638,#13639,#13640,#13641,#13642,#13643,#13644,#13645,#13646,
#13647,#13648,#13649,#13650,#13651,#13652,#13653,#13654,#13655,#13656,#13657,
#13658,#13659,#13660,#13661,#13662,#13663,#13664,#13665,#13666,#13667,#13668,
#13669,#13670,#13671,#13672,#13673,#13674,#13675,#13676,#13677,#13678,#13679,
#13680,#13681,#13682,#13683,#13684,#13685,#13686,#13687,#13688,#13689,#13690,
#13691,#13692,#13693,#13694,#13695,#13696,#13697,#13698,#13699,#13700,#13701,
#13702,#13703,#13704,#13705,#13706,#13707,#13708,#13709,#13710,#13711,#13712,
#13713,#13714,#13715,#13716,#13717,#13718,#13719,#13720,#13721,#13722,#13723,
#13724,#13725,#13726,#13727,#13728,#13729,#13730,#13731,#13732,#13733,#13734,
#13735,#13736,#13737,#13738,#13739,#13740,#13741,#13742,#13743,#13744,#13745,
#13746,#13747,#13748,#13749,#13750,#13751,#13752,#13753,#13754,#13755,#13756,
#13757,#13758,#13759,#13760,#13761,#13762,#13763,#13764,#13765,#13766,#13767,
#13768,#13769,#13770,#13771,#13772,#13773,#13774,#13775,#13776,#13777,#13778,
#13779,#13780,#13781,#13782,#13783,#13784,#13785,#13786,#13787,#13788,#13789,
#13790,#13791,#13792,#13793,#13794,#13795,#13796,#13797,#13798,#13799),
 .UNSPECIFIED.,.F.,.F.,(4,3,3,3,3,3,3,3,3,3,3,3,3,3,3,3,3,3,3,3,3,3,3,3,
3,3,3,3,3,3,3,3,3,3,3,3,3,3,3,3,3,3,3,3,3,3,3,3,3,3,3,3,3,3,3,3,4),(72.2566310325664,
72.2853603822667,72.3622090054542,72.4389638518509,72.5156411912554,72.5922572310304,
72.6688281296554,72.745863862653,72.8224062813587,72.8989546179213,72.975523449369,
73.0529210854358,73.1296121663885,73.2073630800123,73.2851139936361,73.3626315452542,
73.4400617646737,73.5174203075691,73.5947227781564,73.6719847401067,73.7492319658892,
73.8264734770964,73.9037233273291,73.9809955722419,74.0583485302129,74.1357429225217,
74.2132512501902,74.2848676050055,74.3623849742017,74.4398150416529,74.5171734629223,
74.594475842137,74.6717377429,74.7489849535909,74.8262264778095,74.9034763691557,
74.9807486832996,75.0581017545255,75.1354962842769,75.2130047892393,75.2846212163748,
75.3614424135295,75.4381743757438,75.5148333538919,75.5914355403534,75.6679970822344,
75.7450443004231,75.8215884750676,75.8981427551129,75.9747217200926,76.0521349970055,
76.1288464773124,76.2066106525283,76.2843748277442,76.3619669411825,76.4394513885415,
76.4938209771541),.UNSPECIFIED.);
#148=B_SPLINE_CURVE_WITH_KNOTS('',3,(#13800,#13801,#13802,#13803,#13804,
#13805,#13806,#13807,#13808,#13809,#13810,#13811,#13812,#13813,#13814,#13815,
#13816,#13817,#13818,#13819,#13820,#13821,#13822,#13823,#13824,#13825,#13826,
#13827,#13828,#13829,#13830,#13831,#13832,#13833,#13834,#13835,#13836,#13837,
#13838,#13839,#13840,#13841,#13842,#13843,#13844,#13845,#13846,#13847,#13848,
#13849,#13850,#13851,#13852,#13853,#13854,#13855,#13856,#13857,#13858,#13859,
#13860,#13861,#13862,#13863,#13864,#13865,#13866,#13867,#13868,#13869,#13870,
#13871,#13872,#13873,#13874,#13875,#13876,#13877,#13878,#13879,#13880,#13881,
#13882,#13883,#13884),.UNSPECIFIED.,.F.,.F.,(4,3,3,3,3,3,3,3,3,3,3,3,3,
3,3,3,3,3,3,3,3,3,3,3,3,3,3,3,4),(70.2096877536336,70.285853159528,70.3673371324832,
70.4487164966231,70.5329698637705,70.6141233589421,70.6952000369013,70.7761854646915,
70.7857299652127,70.8667383611168,70.9478226179482,71.0322686561855,71.1135747378926,
71.194958527661,71.2764631886896,71.2856067708974,71.3627095955525,71.43973077825,
71.5166863056749,71.5935921150844,71.6704641059723,71.7473312580087,71.8241995322672,
71.9010832966186,71.9779969254215,72.0549985610845,72.132048764585,72.209212210575,
72.2566310324216),.UNSPECIFIED.);
#149=B_SPLINE_CURVE_WITH_KNOTS('',3,(#13886,#13887,#13888,#13889,#13890,
#13891,#13892,#13893,#13894,#13895,#13896,#13897,#13898,#13899,#13900,#13901,
#13902,#13903,#13904,#13905,#13906,#13907,#13908,#13909,#13910,#13911,#13912,
#13913,#13914,#13915,#13916,#13917,#13918,#13919,#13920,#13921,#13922,#13923,
#13924,#13925,#13926,#13927,#13928,#13929,#13930,#13931,#13932,#13933,#13934,
#13935,#13936,#13937,#13938,#13939,#13940,#13941,#13942,#13943,#13944,#13945,
#13946,#13947,#13948,#13949,#13950,#13951,#13952,#13953,#13954,#13955,#13956,
#13957,#13958,#13959,#13960,#13961),.UNSPECIFIED.,.F.,.F.,(4,3,3,3,3,3,
3,3,3,3,3,3,3,3,3,3,3,3,3,3,3,3,3,3,3,4),(70.2101089817503,70.292570585604,
70.3750315235746,70.4574918230603,70.5399515114572,70.6224106161593,70.7048691645584,
70.7873271840447,70.8697847020062,70.9564625976662,71.0389293835019,71.1213944968457,
71.2038580473508,71.2863201446486,71.36878089835,71.4512404180471,71.5336988133147,
71.6161561937119,71.6986225799783,71.781085781992,71.8635462382725,71.9460043871834,
72.0284699920626,72.1109298712771,72.193393984641,72.2566310325662),
 .UNSPECIFIED.);
#150=B_SPLINE_CURVE_WITH_KNOTS('',3,(#13962,#13963,#13964,#13965,#13966,
#13967,#13968,#13969,#13970,#13971,#13972,#13973,#13974,#13975,#13976,#13977,
#13978,#13979,#13980,#13981,#13982,#13983,#13984,#13985,#13986,#13987,#13988,
#13989,#13990,#13991,#13992,#13993,#13994,#13995,#13996,#13997,#13998,#13999,
#14000,#14001,#14002,#14003,#14004,#14005,#14006,#14007,#14008,#14009,#14010,
#14011,#14012,#14013,#14014,#14015,#14016,#14017,#14018,#14019,#14020,#14021,
#14022,#14023,#14024,#14025,#14026,#14027,#14028,#14029,#14030,#14031,#14032,
#14033,#14034,#14035,#14036,#14037,#14038,#14039,#14040,#14041,#14042,#14043,
#14044,#14045,#14046,#14047,#14048,#14049,#14050,#14051,#14052,#14053,#14054,
#14055,#14056,#14057,#14058,#14059,#14060,#14061,#14062,#14063,#14064,#14065,
#14066,#14067,#14068,#14069,#14070,#14071,#14072,#14073,#14074,#14075,#14076,
#14077,#14078,#14079,#14080,#14081,#14082,#14083,#14084,#14085,#14086,#14087,
#14088,#14089,#14090,#14091,#14092,#14093,#14094,#14095,#14096,#14097,#14098,
#14099,#14100,#14101,#14102,#14103,#14104,#14105,#14106,#14107,#14108,#14109,
#14110,#14111,#14112,#14113,#14114,#14115,#14116,#14117,#14118,#14119,#14120,
#14121,#14122,#14123,#14124,#14125,#14126,#14127,#14128,#14129,#14130),
 .UNSPECIFIED.,.F.,.F.,(4,3,3,3,3,3,3,3,3,3,3,3,3,3,3,3,3,3,3,3,3,3,3,3,
3,3,3,3,3,3,3,3,3,3,3,3,3,3,3,3,3,3,3,3,3,3,3,3,3,3,3,3,3,3,3,3,4),(72.2566310325662,
72.3530747522459,72.4514122093326,72.5179213389254,72.5955160083595,72.6730182744698,
72.7504437595404,72.8278080309172,72.9051266120081,72.9824223164796,73.0597073611356,
73.1369957530686,73.2143014985944,73.2916795385818,73.3690946103264,73.4466152245976,
73.5163293469763,73.5978156614092,73.6791977437682,73.7632816455766,73.8444389644296,
73.925519748184,74.0065097402177,74.0155333510018,74.0965464572923,74.1776351515654,
74.2619107024309,74.3432201688204,74.4246070700312,74.5061142087961,74.5147373550273,
74.5922655082364,74.6697123831978,74.7470935619053,74.8244245793659,74.9017209341962,
74.9790112345324,75.0563011422706,75.1336046642688,75.2109358123959,75.2883553022169,
75.3658206606387,75.4434060469367,75.5131453630782,75.5900097845677,75.66678043819,
75.7434735819713,75.8201054116923,75.8966920743709,75.973257994182,76.0498150013944,
76.1263776610667,76.2029605393919,76.2796199398358,76.3563198459075,76.433127667564,
76.4930533832794),.UNSPECIFIED.);
#151=B_SPLINE_CURVE_WITH_KNOTS('',3,(#14136,#14137,#14138,#14139,#14140,
#14141,#14142,#14143,#14144,#14145,#14146,#14147,#14148,#14149,#14150,#14151,
#14152,#14153,#14154,#14155,#14156,#14157,#14158,#14159,#14160,#14161,#14162,
#14163,#14164,#14165,#14166,#14167,#14168,#14169,#14170,#14171,#14172,#14173,
#14174,#14175,#14176,#14177,#14178,#14179,#14180,#14181,#14182,#14183,#14184,
#14185,#14186,#14187,#14188,#14189,#14190,#14191,#14192,#14193,#14194,#14195,
#14196,#14197,#14198,#14199,#14200,#14201,#14202,#14203,#14204,#14205,#14206,
#14207,#14208,#14209,#14210,#14211,#14212,#14213,#14214,#14215,#14216,#14217,
#14218,#14219,#14220,#14221,#14222,#14223,#14224,#14225,#14226,#14227,#14228,
#14229,#14230,#14231,#14232,#14233,#14234,#14235,#14236,#14237,#14238,#14239,
#14240,#14241,#14242,#14243,#14244,#14245,#14246,#14247,#14248,#14249,#14250,
#14251,#14252,#14253,#14254,#14255,#14256,#14257,#14258,#14259,#14260,#14261,
#14262,#14263,#14264,#14265,#14266,#14267,#14268,#14269,#14270,#14271,#14272,
#14273,#14274,#14275,#14276,#14277,#14278,#14279,#14280,#14281,#14282,#14283,
#14284,#14285,#14286,#14287,#14288,#14289,#14290,#14291,#14292),
 .UNSPECIFIED.,.F.,.F.,(4,3,3,3,3,3,3,3,3,3,3,3,3,3,3,3,3,3,3,3,3,3,3,3,
3,3,3,3,3,3,3,3,3,3,3,3,3,3,3,3,3,3,3,3,3,3,3,3,3,3,3,3,4),(78.539816339746,
78.6222785457822,78.7047404035219,78.7872019198156,78.869663101513,78.9521239554642,
79.0345844885185,79.1170447075251,79.1995046193329,79.2819642307906,79.3644235487466,
79.4468825800489,79.5293413315456,79.6117998100843,79.6942580225122,79.7767159756763,
79.8591736764241,79.941631131602,80.0240883480567,80.1101005745584,80.1934249189818,
80.2758915244273,80.3583572856687,80.4408222301212,80.5232863851971,80.605749778306,
80.6882124368546,80.7706743882473,80.853135659886,80.9355962791702,81.0180562734971,
81.1005156702615,81.1829744968567,81.2654327806733,81.3478905491008,81.430347829526,
81.5144810649375,81.5969470630291,81.6794114393846,81.7618743036468,81.8443357654375,
81.9267959343587,82.0092549199942,82.0917128319114,82.1773086774362,82.2597734140363,
82.3422351860383,82.4246944318803,82.5071515898574,82.5896141081386,82.6720717789937,
82.7545305689444,82.7764795961097),.UNSPECIFIED.);
#152=B_SPLINE_CURVE_WITH_KNOTS('',3,(#14293,#14294,#14295,#14296,#14297,
#14298,#14299,#14300,#14301,#14302,#14303,#14304,#14305,#14306,#14307,#14308,
#14309,#14310,#14311,#14312,#14313,#14314,#14315,#14316,#14317,#14318,#14319,
#14320,#14321,#14322,#14323,#14324,#14325,#14326,#14327,#14328,#14329,#14330,
#14331,#14332,#14333,#14334,#14335,#14336,#14337,#14338,#14339,#14340,#14341,
#14342,#14343,#14344,#14345,#14346,#14347,#14348,#14349,#14350,#14351,#14352,
#14353,#14354,#14355,#14356,#14357,#14358,#14359,#14360,#14361,#14362,#14363,
#14364,#14365,#14366,#14367,#14368,#14369,#14370,#14371,#14372,#14373,#14374,
#14375,#14376,#14377),.UNSPECIFIED.,.F.,.F.,(4,3,3,3,3,3,3,3,3,3,3,3,3,
3,3,3,3,3,3,3,3,3,3,3,3,3,3,3,4),(76.4938209771541,76.5711891910363,76.6485068967613,
76.7279595895554,76.80523291,76.8825056629844,76.9597918661467,77.0408760093884,
77.1182683546864,77.1957074620667,77.2732383485027,77.2841284391136,77.3656124120689,
77.4469917762085,77.5312451433559,77.6123986385272,77.6934753164871,77.7744607442775,
77.7840052447983,77.8650136407026,77.9460978975344,78.0305439357715,78.1118500174784,
78.1932338072473,78.2747384682758,78.2838820504829,78.380327679951,78.4755543569099,
78.539816339746),.UNSPECIFIED.);
#153=B_SPLINE_CURVE_WITH_KNOTS('',3,(#14379,#14380,#14381,#14382,#14383,
#14384,#14385,#14386,#14387,#14388,#14389,#14390,#14391,#14392,#14393,#14394,
#14395,#14396,#14397,#14398,#14399,#14400,#14401,#14402,#14403,#14404,#14405,
#14406,#14407,#14408,#14409,#14410,#14411,#14412,#14413,#14414,#14415,#14416,
#14417,#14418,#14419,#14420,#14421,#14422,#14423,#14424,#14425,#14426,#14427,
#14428,#14429,#14430,#14431,#14432,#14433,#14434,#14435,#14436,#14437,#14438,
#14439,#14440,#14441,#14442,#14443,#14444,#14445,#14446,#14447,#14448,#14449,
#14450,#14451,#14452,#14453,#14454,#14455,#14456,#14457,#14458,#14459,#14460,
#14461,#14462,#14463),.UNSPECIFIED.,.F.,.F.,(4,3,3,3,3,3,3,3,3,3,3,3,3,
3,3,3,3,3,3,3,3,3,3,3,3,3,3,3,4),(76.4930533832794,76.5115533711291,76.5890835675889,
76.6665266621943,76.74389829625,76.8212140598187,76.8984895025971,76.9757503850166,
77.053005690661,77.1302694609553,77.2075557394397,77.2849225522317,77.3623308869388,
77.4398524435017,77.50996137918,77.5874914972433,77.6649345265592,77.7423061083848,
77.8196218327448,77.8968972493061,77.9741581253316,78.0514134366779,78.1286772247696,
78.2059635331534,78.2833303947596,78.3607387886916,78.4382604215636,78.5083693872309,
78.5398163397458),.UNSPECIFIED.);
#154=B_SPLINE_CURVE_WITH_KNOTS('',3,(#14464,#14465,#14466,#14467,#14468,
#14469,#14470,#14471,#14472,#14473,#14474,#14475,#14476,#14477,#14478,#14479,
#14480,#14481,#14482,#14483,#14484,#14485,#14486,#14487,#14488,#14489,#14490,
#14491,#14492,#14493,#14494,#14495,#14496,#14497,#14498,#14499,#14500,#14501,
#14502,#14503,#14504,#14505,#14506,#14507,#14508,#14509,#14510,#14511,#14512,
#14513,#14514,#14515,#14516,#14517,#14518,#14519,#14520,#14521,#14522,#14523,
#14524,#14525,#14526,#14527,#14528,#14529,#14530,#14531,#14532,#14533,#14534,
#14535,#14536,#14537,#14538,#14539,#14540,#14541,#14542,#14543,#14544,#14545,
#14546,#14547,#14548,#14549,#14550,#14551,#14552,#14553,#14554,#14555,#14556,
#14557,#14558,#14559,#14560,#14561,#14562,#14563,#14564,#14565,#14566,#14567,
#14568,#14569,#14570,#14571,#14572,#14573,#14574,#14575,#14576,#14577,#14578,
#14579,#14580,#14581,#14582,#14583,#14584,#14585,#14586,#14587,#14588,#14589,
#14590,#14591,#14592,#14593,#14594,#14595,#14596,#14597,#14598,#14599,#14600,
#14601,#14602,#14603,#14604,#14605,#14606,#14607,#14608,#14609,#14610,#14611,
#14612,#14613,#14614,#14615,#14616,#14617,#14618,#14619,#14620,#14621,#14622,
#14623,#14624,#14625,#14626,#14627,#14628,#14629,#14630,#14631,#14632,#14633,
#14634,#14635),.UNSPECIFIED.,.F.,.F.,(4,3,3,3,3,3,3,3,3,3,3,3,3,3,3,3,3,
3,3,3,3,3,3,3,3,3,3,3,3,3,3,3,3,3,3,3,3,3,3,3,3,3,3,3,3,3,3,3,3,3,3,3,3,
3,3,3,3,4),(78.5398163398252,78.6162568128587,78.6926100374869,78.7688925258994,
78.8451207276279,78.9213110445758,78.9974920317676,79.0736713944741,79.1498639412457,
79.2260844876471,79.302392510473,79.3787481973464,79.4552194143481,79.5067773952818,
79.5843720647159,79.6618743308263,79.7392998158967,79.8166640872737,79.8939826683645,
79.9712783728361,80.048563417492,80.125851809425,80.2031575549505,80.2805355949379,
80.3579506666826,80.4354712809538,80.5051854033328,80.5866717177657,80.6680538001247,
80.7521377019331,80.833295020786,80.9143758045396,80.9953657965727,81.0043894073582,
81.0854025136485,81.1664912079208,81.2507667587865,81.3320762251763,81.4134631263875,
81.4949702651519,81.5035934113837,81.5811215645928,81.6585684395543,81.7359496182619,
81.8132806357227,81.8905769905536,81.9678672908898,82.045157198628,82.1224607206263,
82.1997918687533,82.2772113585743,82.3546767169963,82.4322621032943,82.5020014194346,
82.578859309981,82.6556351312199,82.7323238361827,82.7772962578755),
 .UNSPECIFIED.);
#155=B_SPLINE_CURVE_WITH_KNOTS('',3,(#14641,#14642,#14643,#14644,#14645,
#14646,#14647,#14648,#14649,#14650,#14651,#14652,#14653,#14654,#14655,#14656,
#14657,#14658,#14659,#14660,#14661,#14662,#14663,#14664,#14665,#14666,#14667,
#14668,#14669,#14670,#14671,#14672,#14673,#14674,#14675,#14676,#14677,#14678,
#14679,#14680,#14681,#14682,#14683,#14684,#14685,#14686,#14687,#14688,#14689,
#14690,#14691,#14692,#14693,#14694,#14695,#14696,#14697,#14698,#14699,#14700,
#14701,#14702,#14703,#14704,#14705,#14706,#14707,#14708,#14709,#14710,#14711,
#14712,#14713,#14714,#14715,#14716,#14717,#14718,#14719,#14720,#14721,#14722,
#14723,#14724,#14725,#14726,#14727,#14728,#14729,#14730,#14731,#14732,#14733,
#14734,#14735,#14736,#14737,#14738,#14739,#14740,#14741,#14742,#14743,#14744,
#14745,#14746,#14747,#14748,#14749,#14750,#14751,#14752,#14753,#14754,#14755,
#14756,#14757,#14758,#14759,#14760,#14761,#14762,#14763,#14764,#14765,#14766,
#14767,#14768,#14769,#14770,#14771,#14772,#14773,#14774,#14775,#14776,#14777,
#14778,#14779,#14780,#14781,#14782,#14783,#14784,#14785,#14786,#14787,#14788,
#14789,#14790,#14791,#14792,#14793,#14794,#14795,#14796,#14797,#14798,#14799,
#14800,#14801,#14802,#14803,#14804,#14805,#14806),.UNSPECIFIED.,.F.,.F.,
(4,3,3,3,3,3,3,3,3,3,3,3,3,3,3,3,3,3,3,3,3,3,3,3,3,3,3,3,3,3,3,3,3,3,3,
3,3,3,3,3,3,3,3,3,3,3,3,3,3,3,3,3,3,3,3,4),(84.8230016469256,84.9051841266213,
84.9874806104735,85.0699595040246,85.1525329936525,85.2352616759044,85.2821573300685,
85.3596731083316,85.4371074087423,85.5144758271695,85.5917939123196,85.669077176364,
85.7463542606756,85.8236308411634,85.9009209365608,85.9782385705651,86.0556447768896,
86.133096786203,86.2106695945251,86.2819109414379,86.3587595646253,86.4355144110222,
86.5121917504266,86.5888077902016,86.6653786888265,86.7424144218241,86.8189568405298,
86.8955051770924,86.97207400854,87.0494716446069,87.1261627255596,87.2039136391834,
87.2816645528073,87.3591821044254,87.4366123238449,87.5139708667404,87.5912733373275,
87.6685352992777,87.7457825250603,87.8230240362676,87.9002738865004,87.9775461314133,
88.0548990893843,88.132293481693,88.2098018093615,88.2814181641766,88.3589477898889,
88.4363876561042,88.5142386608849,88.5915371477998,88.668798429308,88.7460365802883,
88.8243263588036,88.9015777359387,88.9803867151441,89.0591956943495),
 .UNSPECIFIED.);
#156=B_SPLINE_CURVE_WITH_KNOTS('',3,(#14807,#14808,#14809,#14810,#14811,
#14812,#14813,#14814,#14815,#14816,#14817,#14818,#14819,#14820,#14821,#14822,
#14823,#14824,#14825,#14826,#14827,#14828,#14829,#14830,#14831,#14832,#14833,
#14834,#14835,#14836,#14837,#14838,#14839,#14840,#14841,#14842,#14843,#14844,
#14845,#14846,#14847,#14848,#14849,#14850,#14851,#14852,#14853,#14854,#14855,
#14856,#14857,#14858,#14859,#14860,#14861,#14862,#14863,#14864,#14865,#14866,
#14867,#14868,#14869,#14870,#14871,#14872,#14873,#14874,#14875,#14876,#14877,
#14878,#14879,#14880,#14881,#14882),.UNSPECIFIED.,.F.,.F.,(4,3,3,3,3,3,
3,3,3,3,3,3,3,3,3,3,3,3,3,3,3,3,3,3,3,4),(82.7764795961097,82.8589411999635,
82.941402137934,83.0238624374197,83.1063221258167,83.1887812305187,83.271239778918,
83.3536977984043,83.4361553163657,83.5228332120257,83.6052999978614,83.6877651112052,
83.7702286617103,83.852690759008,83.9351515127094,84.0176110324066,84.1000694276743,
84.1825268080714,84.2649931943378,84.3474563963516,84.4299168526321,84.5123750015429,
84.5948406064222,84.6773004856367,84.7597645990006,84.8230016469256),
 .UNSPECIFIED.);
#157=B_SPLINE_CURVE_WITH_KNOTS('',3,(#14884,#14885,#14886,#14887,#14888,
#14889,#14890,#14891,#14892,#14893,#14894,#14895,#14896,#14897,#14898,#14899,
#14900,#14901,#14902,#14903,#14904,#14905,#14906,#14907,#14908,#14909,#14910,
#14911,#14912,#14913,#14914,#14915,#14916,#14917,#14918,#14919,#14920,#14921,
#14922,#14923,#14924,#14925,#14926,#14927,#14928,#14929,#14930,#14931,#14932,
#14933,#14934,#14935,#14936,#14937,#14938,#14939,#14940,#14941,#14942,#14943,
#14944,#14945,#14946,#14947,#14948,#14949,#14950,#14951,#14952,#14953,#14954,
#14955,#14956,#14957,#14958,#14959,#14960,#14961,#14962,#14963,#14964,#14965),
 .UNSPECIFIED.,.F.,.F.,(4,3,3,3,3,3,3,3,3,3,3,3,3,3,3,3,3,3,3,3,3,3,3,3,
3,3,3,4),(82.7772962578755,82.8538993615407,82.9304669669959,83.0070270870308,
83.0835871435194,83.1601617015671,83.2367653327514,83.3134533235216,83.3901896333783,
83.4670319898012,83.5004094274855,83.5779396239453,83.655382718551,83.732754352607,
83.8100701161757,83.8873455589542,83.9646064413739,84.0418617470183,84.1191255173126,
84.1964117957971,84.2737786085891,84.3511869432957,84.4287084998586,84.4988174355364,
84.5900064650122,84.6808065702415,84.770854205132,84.8230016468377),
 .UNSPECIFIED.);
#158=B_SPLINE_CURVE_WITH_KNOTS('',3,(#14966,#14967,#14968,#14969,#14970,
#14971,#14972,#14973,#14974,#14975,#14976,#14977,#14978,#14979,#14980,#14981,
#14982,#14983,#14984,#14985,#14986,#14987,#14988,#14989,#14990,#14991,#14992,
#14993,#14994,#14995,#14996,#14997,#14998,#14999,#15000,#15001,#15002,#15003,
#15004,#15005,#15006,#15007,#15008,#15009,#15010,#15011,#15012,#15013,#15014,
#15015,#15016,#15017,#15018,#15019,#15020,#15021,#15022,#15023,#15024,#15025,
#15026,#15027,#15028,#15029,#15030,#15031,#15032,#15033,#15034,#15035,#15036,
#15037,#15038,#15039,#15040,#15041,#15042,#15043,#15044,#15045,#15046,#15047,
#15048,#15049,#15050,#15051,#15052,#15053,#15054,#15055,#15056,#15057,#15058,
#15059,#15060,#15061,#15062,#15063,#15064,#15065,#15066,#15067,#15068,#15069,
#15070,#15071,#15072,#15073,#15074,#15075,#15076,#15077,#15078,#15079,#15080,
#15081,#15082,#15083,#15084,#15085,#15086,#15087,#15088,#15089,#15090,#15091,
#15092,#15093,#15094,#15095,#15096,#15097,#15098,#15099,#15100,#15101,#15102,
#15103,#15104,#15105,#15106,#15107,#15108,#15109,#15110,#15111,#15112,#15113,
#15114,#15115,#15116,#15117,#15118,#15119,#15120,#15121,#15122,#15123,#15124,
#15125,#15126,#15127,#15128,#15129,#15130,#15131,#15132,#15133,#15134,#15135,
#15136,#15137),.UNSPECIFIED.,.F.,.F.,(4,3,3,3,3,3,3,3,3,3,3,3,3,3,3,3,3,
3,3,3,3,3,3,3,3,3,3,3,3,3,3,3,3,3,3,3,3,3,3,3,3,3,3,3,3,3,3,3,3,3,3,3,3,
3,3,3,3,4),(84.8230016469254,84.900259979548,84.9775140309716,85.0547691519919,
85.1320393290555,85.2093385544003,85.2867251748822,85.3641589545451,85.4417070272323,
85.4972254435874,85.57406147571,85.6508084914372,85.7274827290005,85.8041003685221,
85.8806775451493,85.9575470334604,86.0341071359831,86.1106774331304,86.1872724941531,
86.2643627335244,86.3410899301058,86.4183616908721,86.4956334516383,86.5732281210723,
86.6507303871827,86.7281558722534,86.8055201436303,86.8828387247205,86.9601344291921,
87.0374194738481,87.1147078657812,87.1920136113069,87.2693916512942,87.3468067230389,
87.4243273373101,87.4940414596892,87.5755277741222,87.6569098564808,87.7409937582893,
87.8221510771424,87.9032318608979,87.9842218529317,87.9932454637146,88.074258570005,
88.1553472642779,88.2396228151435,88.3209322815331,88.4023191827436,88.4838263215085,
88.4924494677401,88.5699718073358,88.6474167446868,88.724798397842,88.8021308455058,
88.8794289255214,88.9567073170796,89.0339881810012,89.0594182937293),
 .UNSPECIFIED.);
#159=B_SPLINE_CURVE_WITH_KNOTS('',3,(#15143,#15144,#15145,#15146,#15147,
#15148,#15149,#15150,#15151,#15152,#15153,#15154,#15155,#15156,#15157,#15158,
#15159,#15160,#15161,#15162,#15163,#15164,#15165,#15166,#15167,#15168,#15169,
#15170,#15171,#15172,#15173,#15174,#15175,#15176,#15177,#15178,#15179,#15180,
#15181,#15182,#15183,#15184,#15185,#15186,#15187,#15188,#15189,#15190,#15191,
#15192,#15193,#15194,#15195,#15196,#15197,#15198,#15199,#15200,#15201,#15202,
#15203,#15204,#15205,#15206,#15207,#15208,#15209,#15210,#15211,#15212,#15213,
#15214,#15215,#15216,#15217,#15218,#15219,#15220,#15221,#15222,#15223,#15224,
#15225,#15226,#15227,#15228,#15229,#15230,#15231,#15232,#15233,#15234,#15235,
#15236,#15237,#15238,#15239,#15240,#15241,#15242,#15243,#15244,#15245,#15246,
#15247,#15248,#15249,#15250,#15251,#15252,#15253,#15254,#15255,#15256,#15257,
#15258,#15259,#15260,#15261,#15262,#15263,#15264,#15265,#15266,#15267,#15268,
#15269,#15270,#15271,#15272,#15273,#15274,#15275,#15276,#15277,#15278,#15279,
#15280,#15281,#15282,#15283,#15284,#15285,#15286,#15287,#15288,#15289,#15290,
#15291,#15292,#15293,#15294,#15295,#15296,#15297,#15298,#15299),
 .UNSPECIFIED.,.F.,.F.,(4,3,3,3,3,3,3,3,3,3,3,3,3,3,3,3,3,3,3,3,3,3,3,3,
3,3,3,3,3,3,3,3,3,3,3,3,3,3,3,3,3,3,3,3,3,3,3,3,3,3,3,3,4),(91.1061869541052,
91.1886491601415,91.2711110178812,91.3535725341748,91.4360337158723,91.5184945698235,
91.6009551028778,91.6834153218843,91.7658752336922,91.8483348451498,91.9307941631057,
92.0132531944081,92.0957119459048,92.1781704244433,92.2606286368711,92.3430865900354,
92.4255442907829,92.508001745961,92.5904589624156,92.6764711889173,92.7597955333408,
92.8422621387863,92.9247279000277,93.0071928444802,93.0896569995562,93.172120392665,
93.2545830512136,93.3370450026064,93.4195062742451,93.5019668935292,93.584426887856,
93.6668862846205,93.7493451112156,93.8318033950323,93.9142611634597,93.996718443885,
94.0808516792965,94.1633176773882,94.2457820537436,94.3282449180059,94.4107063797965,
94.4931665487176,94.5756255343531,94.6580834462704,94.7436792917952,94.8261440283953,
94.9086058003973,94.9910650462394,95.0735222042164,95.1559847224976,95.2384423933526,
95.3209011833033,95.3428502104689),.UNSPECIFIED.);
#160=B_SPLINE_CURVE_WITH_KNOTS('',3,(#15300,#15301,#15302,#15303,#15304,
#15305,#15306,#15307,#15308,#15309,#15310,#15311,#15312,#15313,#15314,#15315,
#15316,#15317,#15318,#15319,#15320,#15321,#15322,#15323,#15324,#15325,#15326,
#15327,#15328,#15329,#15330,#15331,#15332,#15333,#15334,#15335,#15336,#15337,
#15338,#15339,#15340,#15341,#15342,#15343,#15344,#15345,#15346,#15347,#15348,
#15349,#15350,#15351,#15352,#15353,#15354,#15355,#15356,#15357,#15358,#15359,
#15360,#15361,#15362,#15363,#15364,#15365,#15366,#15367,#15368,#15369,#15370,
#15371,#15372,#15373,#15374,#15375,#15376,#15377,#15378,#15379,#15380,#15381),
 .UNSPECIFIED.,.F.,.F.,(4,3,3,3,3,3,3,3,3,3,3,3,3,3,3,3,3,3,3,3,3,3,3,3,
3,3,3,4),(89.0591956943495,89.1365930519662,89.2141031437056,89.281171775546,
89.3579929727008,89.4347249349151,89.5113839130629,89.5879860995243,89.6645476414052,
89.741594859594,89.8181390342383,89.8946933142836,89.9712722792633,90.0486855561763,
90.1253970364832,90.2031612116993,90.2809253869154,90.3576414403888,90.4342648893733,
90.5108121340303,90.5872920412522,90.663734501548,90.7401542288347,90.8165659204488,
90.8930108655814,90.9694722519528,91.0460033091413,91.105416707111),
 .UNSPECIFIED.);
#161=B_SPLINE_CURVE_WITH_KNOTS('',3,(#15383,#15384,#15385,#15386,#15387,
#15388,#15389,#15390,#15391,#15392,#15393,#15394,#15395,#15396,#15397,#15398,
#15399,#15400,#15401,#15402,#15403,#15404,#15405,#15406,#15407,#15408,#15409,
#15410,#15411,#15412,#15413,#15414,#15415,#15416,#15417,#15418,#15419,#15420,
#15421,#15422,#15423,#15424,#15425,#15426,#15427,#15428,#15429,#15430,#15431,
#15432,#15433,#15434,#15435,#15436,#15437,#15438,#15439,#15440,#15441,#15442,
#15443,#15444,#15445,#15446,#15447,#15448,#15449,#15450,#15451,#15452,#15453,
#15454,#15455,#15456,#15457,#15458,#15459,#15460,#15461,#15462,#15463,#15464),
 .UNSPECIFIED.,.F.,.F.,(4,3,3,3,3,3,3,3,3,3,3,3,3,3,3,3,3,3,3,3,3,3,3,3,
3,3,3,4),(89.0594182937293,89.1367293492698,89.2140726386133,89.2915058024444,
89.3689889815936,89.4465849562361,89.490857475791,89.5677208604433,89.6444906922528,
89.7211832282412,89.7978146634082,89.8744011441913,89.9512591866476,90.027817509611,
90.1043818442834,90.1809667574108,90.2580414390186,90.3347482598874,90.4120068718647,
90.4892654838419,90.5677895481334,90.6462209244004,90.7245725981383,90.8028575049273,
90.8810803650547,90.9592661290473,91.0374327518346,91.106186954105),
 .UNSPECIFIED.);
#162=B_SPLINE_CURVE_WITH_KNOTS('',3,(#15465,#15466,#15467,#15468,#15469,
#15470,#15471,#15472,#15473,#15474,#15475,#15476,#15477,#15478,#15479,#15480,
#15481,#15482,#15483,#15484,#15485,#15486,#15487,#15488,#15489,#15490,#15491,
#15492,#15493,#15494,#15495,#15496,#15497,#15498,#15499,#15500,#15501,#15502,
#15503,#15504,#15505,#15506,#15507,#15508,#15509,#15510,#15511,#15512,#15513,
#15514,#15515,#15516,#15517,#15518,#15519,#15520,#15521,#15522,#15523,#15524,
#15525,#15526,#15527,#15528,#15529,#15530,#15531,#15532,#15533,#15534,#15535,
#15536,#15537,#15538,#15539,#15540,#15541,#15542,#15543,#15544,#15545,#15546,
#15547,#15548,#15549,#15550,#15551,#15552,#15553,#15554,#15555,#15556,#15557,
#15558,#15559,#15560,#15561,#15562,#15563,#15564,#15565,#15566,#15567,#15568,
#15569,#15570,#15571,#15572,#15573,#15574,#15575,#15576,#15577,#15578,#15579,
#15580,#15581,#15582,#15583,#15584,#15585,#15586,#15587,#15588,#15589,#15590,
#15591,#15592,#15593,#15594,#15595,#15596,#15597,#15598,#15599,#15600,#15601,
#15602,#15603,#15604,#15605,#15606,#15607,#15608,#15609,#15610,#15611,#15612,
#15613,#15614,#15615,#15616,#15617,#15618,#15619,#15620,#15621,#15622,#15623,
#15624,#15625,#15626,#15627,#15628,#15629,#15630,#15631,#15632,#15633),
 .UNSPECIFIED.,.F.,.F.,(4,3,3,3,3,3,3,3,3,3,3,3,3,3,3,3,3,3,3,3,3,3,3,3,
3,3,3,3,3,3,3,3,3,3,3,3,3,3,3,3,3,3,3,3,3,3,3,3,3,3,3,3,3,3,3,3,4),(91.106186954195,
91.1920170383312,91.2783242322604,91.3648739223735,91.4517397796147,91.4876734918928,
91.5652036099561,91.642646639272,91.7200182210975,91.7973339454571,91.8746093620186,
91.951870238044,92.0291255493902,92.1063893374818,92.1836756458659,92.2610425074721,
92.3384509014041,92.4159725342761,92.4860814999438,92.5629175320664,92.6396645477935,
92.7163387853568,92.7929564248784,92.8695336015055,92.9464030898166,93.0229631923393,
93.0995334894866,93.1761285505091,93.2532187898805,93.329945986462,93.4072177472283,
93.4844895079947,93.5620841774288,93.6395864435391,93.7170119286096,93.7943761999865,
93.8716947810774,93.9489904855489,94.0262755302049,94.1035639221379,94.1808696676636,
94.258247707651,94.3356627793956,94.4131833936668,94.4828975160456,94.5643838304785,
94.6457659128375,94.7298498146459,94.8110071334989,94.8920879172536,94.9730779092874,
94.9821015200711,95.0630915629816,95.1442058159851,95.2253866236002,95.3066844308499,
95.3424746944017),.UNSPECIFIED.);
#163=B_SPLINE_CURVE_WITH_KNOTS('',3,(#15639,#15640,#15641,#15642,#15643,
#15644,#15645,#15646,#15647,#15648,#15649,#15650,#15651,#15652,#15653,#15654,
#15655,#15656,#15657,#15658,#15659,#15660,#15661,#15662,#15663,#15664,#15665,
#15666,#15667,#15668,#15669,#15670,#15671,#15672,#15673,#15674,#15675,#15676,
#15677,#15678,#15679,#15680,#15681,#15682,#15683,#15684,#15685,#15686,#15687,
#15688,#15689,#15690,#15691,#15692,#15693,#15694,#15695,#15696,#15697,#15698,
#15699,#15700,#15701,#15702,#15703,#15704,#15705,#15706,#15707,#15708,#15709,
#15710,#15711,#15712,#15713,#15714,#15715,#15716,#15717,#15718,#15719,#15720,
#15721,#15722,#15723,#15724,#15725,#15726,#15727,#15728,#15729,#15730,#15731,
#15732,#15733,#15734,#15735,#15736,#15737,#15738,#15739,#15740,#15741,#15742,
#15743,#15744,#15745,#15746,#15747,#15748,#15749,#15750,#15751,#15752,#15753,
#15754,#15755,#15756,#15757,#15758,#15759,#15760,#15761,#15762,#15763,#15764,
#15765,#15766,#15767,#15768,#15769,#15770,#15771,#15772,#15773,#15774,#15775,
#15776,#15777,#15778,#15779,#15780,#15781,#15782,#15783,#15784,#15785,#15786,
#15787,#15788,#15789,#15790,#15791,#15792,#15793,#15794,#15795,#15796,#15797,
#15798,#15799,#15800,#15801,#15802,#15803,#15804,#15805,#15806,#15807,#15808,
#15809,#15810),.UNSPECIFIED.,.F.,.F.,(4,3,3,3,3,3,3,3,3,3,3,3,3,3,3,3,3,
3,3,3,3,3,3,3,3,3,3,3,3,3,3,3,3,3,3,3,3,3,3,3,3,3,3,3,3,3,3,3,3,3,3,3,3,
3,3,3,3,4),(97.3898726090998,97.4662065462312,97.5424567142456,97.6186396946541,
97.6947720072897,97.7708759140936,97.846966464458,97.9230585390012,97.9991670176848,
98.0753453720321,98.1515615244939,98.227877771978,98.2789542778703,98.3604382508255,
98.4418176149653,98.5260709821127,98.6072244772844,98.6883011552429,98.7692865830328,
98.778831083555,98.8598394794593,98.9409237362904,99.0253697745277,99.1066758562345,
99.1880596460033,99.2695643070317,99.2787078892397,99.3562236675028,99.4336579679133,
99.5110263863403,99.5883444714906,99.6656277355348,99.7429048198463,99.8201814003342,
99.8974714957315,99.9747891297362,100.052195336061,100.129647345374,100.207220153696,
100.278461500609,100.355310123796,100.432064970194,100.508742309598,100.585358349373,
100.661929247998,100.738964980996,100.815507399701,100.892055736264,100.968624567712,
101.046022203778,101.122713284731,101.200464198355,101.278215111978,101.355749929111,
101.433174288491,101.510534996438,101.587835153039,101.626359673358),
 .UNSPECIFIED.);
#164=B_SPLINE_CURVE_WITH_KNOTS('',3,(#15811,#15812,#15813,#15814,#15815,
#15816,#15817,#15818,#15819,#15820,#15821,#15822,#15823,#15824,#15825,#15826,
#15827,#15828,#15829,#15830,#15831,#15832,#15833,#15834,#15835,#15836,#15837,
#15838,#15839,#15840,#15841,#15842,#15843,#15844,#15845,#15846,#15847,#15848,
#15849,#15850,#15851,#15852,#15853,#15854,#15855,#15856,#15857,#15858,#15859,
#15860,#15861,#15862,#15863,#15864,#15865,#15866,#15867,#15868,#15869,#15870,
#15871,#15872,#15873,#15874,#15875,#15876,#15877,#15878,#15879,#15880,#15881,
#15882,#15883,#15884,#15885,#15886),.UNSPECIFIED.,.F.,.F.,(4,3,3,3,3,3,
3,3,3,3,3,3,3,3,3,3,3,3,3,3,3,3,3,3,3,4),(95.3428502104689,95.4253118143227,
95.5077727522932,95.5902330517789,95.6726927401757,95.7551518448778,95.837610393277,
95.9200684127633,96.0025259307248,96.0892038263848,96.1716706122204,96.2541357255642,
96.3365992760693,96.4190613733671,96.5015221270684,96.5839816467656,96.6664400420332,
96.7488974224304,96.8313638086968,96.9138270107106,96.9962874669912,97.0787456159018,
97.161211220781,97.2436710999955,97.3261352133594,97.3893722612848),
 .UNSPECIFIED.);
#165=B_SPLINE_CURVE_WITH_KNOTS('',3,(#15888,#15889,#15890,#15891,#15892,
#15893,#15894,#15895,#15896,#15897,#15898,#15899,#15900,#15901,#15902,#15903,
#15904,#15905,#15906,#15907,#15908,#15909,#15910,#15911,#15912,#15913,#15914,
#15915,#15916,#15917,#15918,#15919,#15920,#15921,#15922,#15923,#15924,#15925,
#15926,#15927,#15928,#15929,#15930,#15931,#15932,#15933,#15934,#15935,#15936,
#15937,#15938,#15939,#15940,#15941,#15942,#15943,#15944,#15945,#15946,#15947,
#15948,#15949,#15950,#15951,#15952,#15953,#15954,#15955,#15956,#15957,#15958,
#15959,#15960,#15961,#15962,#15963,#15964,#15965,#15966,#15967,#15968,#15969),
 .UNSPECIFIED.,.F.,.F.,(4,3,3,3,3,3,3,3,3,3,3,3,3,3,3,3,3,3,3,3,3,3,3,3,
3,3,3,4),(95.3424746944017,95.423953095677,95.4813055240965,95.5588336773056,
95.636280552267,95.7136617309745,95.7909927484351,95.8682891032655,95.9455794036017,
96.02286931134,96.1001728333381,96.1775039814651,96.2549234712861,96.3323888297079,
96.409974216006,96.4797135321474,96.5556971028836,96.6315883519272,96.7074041199809,
96.7831611674713,96.8588792362736,96.934577022471,97.0102695900154,97.0859719978792,
97.1617397381996,97.2375397227215,97.3134445270289,97.3887660913681),
 .UNSPECIFIED.);
#166=B_SPLINE_CURVE_WITH_KNOTS('',3,(#15970,#15971,#15972,#15973,#15974,
#15975,#15976,#15977,#15978,#15979,#15980,#15981,#15982,#15983,#15984,#15985,
#15986,#15987,#15988,#15989,#15990,#15991,#15992,#15993,#15994,#15995,#15996,
#15997,#15998,#15999,#16000,#16001,#16002,#16003,#16004,#16005,#16006,#16007,
#16008,#16009,#16010,#16011,#16012,#16013,#16014,#16015,#16016,#16017,#16018,
#16019,#16020,#16021,#16022,#16023,#16024,#16025,#16026,#16027,#16028,#16029,
#16030,#16031,#16032,#16033,#16034,#16035,#16036,#16037,#16038,#16039,#16040,
#16041,#16042,#16043,#16044,#16045,#16046,#16047,#16048,#16049,#16050,#16051,
#16052,#16053,#16054,#16055,#16056,#16057,#16058,#16059,#16060,#16061,#16062,
#16063,#16064,#16065,#16066,#16067,#16068,#16069,#16070,#16071,#16072,#16073,
#16074,#16075,#16076,#16077,#16078,#16079,#16080,#16081,#16082,#16083,#16084,
#16085,#16086,#16087,#16088,#16089,#16090,#16091,#16092,#16093,#16094,#16095,
#16096,#16097,#16098,#16099,#16100,#16101,#16102,#16103,#16104,#16105,#16106,
#16107,#16108,#16109,#16110,#16111,#16112,#16113,#16114,#16115,#16116,#16117,
#16118,#16119,#16120,#16121,#16122,#16123,#16124,#16125,#16126),
 .UNSPECIFIED.,.F.,.F.,(4,3,3,3,3,3,3,3,3,3,3,3,3,3,3,3,3,3,3,3,3,3,3,3,
3,3,3,3,3,3,3,3,3,3,3,3,3,3,3,3,3,3,3,3,3,3,3,3,3,3,3,3,4),(97.3893956674183,
97.4718578733547,97.5543197309966,97.6367812471942,97.7192424287977,97.8017032826569,
97.8841638156211,97.9666240345395,98.0490839462611,98.1315435576345,98.2140028755081,
98.29646190673,98.3789206581482,98.46137913661,98.5438373489633,98.6262953020549,
98.7087530027319,98.791210457841,98.8736676742287,98.9596791693356,99.0430028052203,
99.1254694104373,99.2079351714575,99.2904001156961,99.3728642705655,99.455327663475,
99.5377903218316,99.6202522730397,99.702713544501,99.785174163615,99.867634157779,
99.950093554388,100.032552380835,100.115010664511,100.197468432805,100.279925713104,
100.364057575888,100.446523573561,100.528987949525,100.611450813423,100.693912274877,
100.776372443489,100.858831428843,100.941289340506,101.026882612649,101.109347348554,
101.191809119956,101.274268365294,101.356725522863,101.439188039894,101.521645709882,
101.604104497894,101.626035517648),.UNSPECIFIED.);
#167=B_SPLINE_CURVE_WITH_KNOTS('',3,(#16132,#16133,#16134,#16135,#16136,
#16137,#16138,#16139,#16140,#16141,#16142,#16143,#16144,#16145,#16146,#16147,
#16148,#16149,#16150,#16151,#16152,#16153,#16154,#16155,#16156,#16157,#16158,
#16159,#16160,#16161,#16162,#16163,#16164,#16165,#16166,#16167,#16168,#16169,
#16170,#16171,#16172,#16173,#16174,#16175,#16176,#16177,#16178,#16179,#16180,
#16181,#16182,#16183,#16184,#16185,#16186,#16187,#16188,#16189,#16190,#16191,
#16192,#16193,#16194,#16195,#16196,#16197,#16198,#16199,#16200,#16201,#16202,
#16203,#16204,#16205,#16206,#16207,#16208,#16209,#16210,#16211,#16212,#16213,
#16214,#16215,#16216,#16217,#16218,#16219,#16220,#16221,#16222,#16223,#16224,
#16225,#16226,#16227,#16228,#16229,#16230,#16231,#16232,#16233,#16234,#16235,
#16236,#16237,#16238,#16239,#16240,#16241,#16242,#16243,#16244,#16245,#16246,
#16247,#16248,#16249,#16250,#16251,#16252,#16253,#16254,#16255,#16256,#16257,
#16258,#16259,#16260,#16261,#16262,#16263,#16264,#16265,#16266,#16267,#16268,
#16269,#16270,#16271,#16272,#16273,#16274,#16275,#16276,#16277,#16278,#16279,
#16280,#16281,#16282,#16283,#16284,#16285,#16286,#16287,#16288),
 .UNSPECIFIED.,.F.,.F.,(4,3,3,3,3,3,3,3,3,3,3,3,3,3,3,3,3,3,3,3,3,3,3,3,
3,3,3,3,3,3,3,3,3,3,3,3,3,3,3,3,3,3,3,3,3,3,3,3,3,3,3,3,4),(103.672557568464,
103.7550197745,103.83748163224,103.919943148534,104.002404330231,104.084865184182,
104.167325717237,104.249785936243,104.332245848051,104.414705459509,104.497164777465,
104.579623808767,104.662082560264,104.744541038802,104.82699925123,104.909457204394,
104.991914905142,105.07437236032,105.156829576775,105.242841803276,105.3261661477,
105.408632753145,105.491098514387,105.573563458839,105.656027613915,105.738491007024,
105.820953665572,105.903415616965,105.985876888604,106.068337507888,106.150797502215,
106.233256898979,106.315715725575,106.398174009391,106.480631777819,106.563089058244,
106.647222293656,106.729688291747,106.812152668103,106.894615532365,106.977076994156,
107.059537163077,107.141996148712,107.224454060629,107.310049906154,107.392514642754,
107.474976414756,107.557435660598,107.639892818576,107.722355336857,107.804813007712,
107.887271797662,107.909220824828),.UNSPECIFIED.);
#168=B_SPLINE_CURVE_WITH_KNOTS('',3,(#16289,#16290,#16291,#16292,#16293,
#16294,#16295,#16296,#16297,#16298,#16299,#16300,#16301,#16302,#16303,#16304,
#16305,#16306,#16307,#16308,#16309,#16310,#16311,#16312,#16313,#16314,#16315,
#16316,#16317,#16318,#16319,#16320,#16321,#16322,#16323,#16324,#16325,#16326,
#16327,#16328,#16329,#16330,#16331,#16332,#16333,#16334,#16335,#16336,#16337,
#16338,#16339,#16340,#16341,#16342,#16343,#16344,#16345,#16346,#16347,#16348,
#16349,#16350,#16351,#16352,#16353,#16354,#16355,#16356,#16357,#16358,#16359,
#16360,#16361,#16362,#16363,#16364,#16365,#16366,#16367,#16368,#16369,#16370),
 .UNSPECIFIED.,.F.,.F.,(4,3,3,3,3,3,3,3,3,3,3,3,3,3,3,3,3,3,3,3,3,3,3,3,
3,3,3,4),(101.626359673358,101.703607239662,101.780849858977,101.858093771854,
101.935353031952,102.012641698857,102.090013724377,102.167433491956,102.244956987448,
102.277968723348,102.355486092544,102.432916159996,102.510274581265,102.58757696048,
102.664838861243,102.742086071934,102.819327596153,102.896577487499,102.973849801642,
103.051202872868,103.12859740262,103.206105907582,103.277722334717,103.363331372225,
103.448584455864,103.533612860426,103.618273980915,103.672557568464),
 .UNSPECIFIED.);
#169=B_SPLINE_CURVE_WITH_KNOTS('',3,(#16372,#16373,#16374,#16375,#16376,
#16377,#16378,#16379,#16380,#16381,#16382,#16383,#16384,#16385,#16386,#16387,
#16388,#16389,#16390,#16391,#16392,#16393,#16394,#16395,#16396,#16397,#16398,
#16399,#16400,#16401,#16402,#16403,#16404,#16405,#16406,#16407,#16408,#16409,
#16410,#16411,#16412,#16413,#16414,#16415,#16416,#16417,#16418,#16419,#16420,
#16421,#16422,#16423,#16424,#16425,#16426,#16427,#16428,#16429,#16430,#16431,
#16432,#16433,#16434,#16435,#16436,#16437,#16438,#16439,#16440,#16441,#16442,
#16443,#16444,#16445,#16446,#16447),.UNSPECIFIED.,.F.,.F.,(4,3,3,3,3,3,
3,3,3,3,3,3,3,3,3,3,3,3,3,3,3,3,3,3,3,4),(101.626035517648,101.708497121502,
101.790958059472,101.873418358958,101.955878047355,102.038337152057,102.120795700456,
102.203253719943,102.285711237904,102.372389133564,102.4548559194,102.537321032744,
102.619784583249,102.702246680546,102.784707434248,102.867166953945,102.949625349213,
103.03208272961,103.114549115876,103.19701231789,103.279472774171,103.361930923081,
103.444396527961,103.526856407175,103.609320520539,103.672557568464),
 .UNSPECIFIED.);
#170=B_SPLINE_CURVE_WITH_KNOTS('',3,(#16448,#16449,#16450,#16451,#16452,
#16453,#16454,#16455,#16456,#16457,#16458,#16459,#16460,#16461,#16462,#16463,
#16464,#16465,#16466,#16467,#16468,#16469,#16470,#16471,#16472,#16473,#16474,
#16475,#16476,#16477,#16478,#16479,#16480,#16481,#16482,#16483,#16484,#16485,
#16486,#16487,#16488,#16489,#16490,#16491,#16492,#16493,#16494,#16495,#16496,
#16497,#16498,#16499,#16500,#16501,#16502,#16503,#16504,#16505,#16506,#16507,
#16508,#16509,#16510,#16511,#16512,#16513,#16514,#16515,#16516,#16517,#16518,
#16519,#16520,#16521,#16522,#16523,#16524,#16525,#16526,#16527,#16528,#16529,
#16530,#16531,#16532,#16533,#16534,#16535,#16536,#16537,#16538,#16539,#16540,
#16541,#16542,#16543,#16544,#16545,#16546,#16547,#16548,#16549,#16550,#16551,
#16552,#16553,#16554,#16555,#16556,#16557,#16558,#16559,#16560,#16561,#16562,
#16563,#16564,#16565,#16566,#16567,#16568,#16569,#16570,#16571,#16572,#16573,
#16574,#16575,#16576,#16577,#16578,#16579,#16580,#16581,#16582,#16583,#16584,
#16585,#16586,#16587,#16588,#16589,#16590,#16591,#16592,#16593,#16594,#16595,
#16596,#16597,#16598,#16599,#16600,#16601,#16602,#16603,#16604,#16605,#16606,
#16607,#16608,#16609,#16610,#16611,#16612,#16613,#16614,#16615,#16616),
 .UNSPECIFIED.,.F.,.F.,(4,3,3,3,3,3,3,3,3,3,3,3,3,3,3,3,3,3,3,3,3,3,3,3,
3,3,3,3,3,3,3,3,3,3,3,3,3,3,3,3,3,3,3,3,3,3,3,3,3,3,3,3,3,3,3,3,4),(103.673734240473,
103.74932672623,103.824858365227,103.900345978336,103.975815541418,104.051278467764,
104.126749916025,104.202245051749,104.277819299239,104.353438159594,104.429161669901,
104.466977596555,104.544507793015,104.62195088762,104.699322521676,104.776638285245,
104.853913728023,104.931174610443,105.008429916087,105.085693686381,105.162979964866,
105.240346777658,105.317755112365,105.395276668928,105.465385604606,105.542915722669,
105.620358751985,105.697730333811,105.77504605817,105.852321474732,105.929582350757,
106.006837662104,106.084101450195,106.161387758579,106.238754620185,106.316163014118,
106.39368464699,106.463793612657,106.54062964478,106.617376660507,106.69405089807,
106.770668537592,106.847245714218,106.92411520253,107.000675305052,107.0772456022,
107.153840663222,107.230930902593,107.307658099175,107.384929859941,107.462201620708,
107.539802243061,107.617313191671,107.694730000345,107.772092372968,107.849409710893,
107.909426078052),.UNSPECIFIED.);
#171=B_SPLINE_CURVE_WITH_KNOTS('',3,(#16622,#16623,#16624,#16625,#16626,
#16627,#16628,#16629,#16630,#16631,#16632,#16633,#16634,#16635,#16636,#16637,
#16638,#16639,#16640,#16641,#16642,#16643,#16644,#16645,#16646,#16647,#16648,
#16649,#16650,#16651,#16652,#16653,#16654,#16655,#16656,#16657,#16658,#16659,
#16660,#16661,#16662,#16663,#16664,#16665,#16666,#16667,#16668,#16669,#16670,
#16671,#16672,#16673,#16674,#16675,#16676,#16677,#16678,#16679,#16680,#16681,
#16682,#16683,#16684,#16685,#16686,#16687,#16688,#16689,#16690,#16691,#16692,
#16693,#16694,#16695,#16696,#16697,#16698,#16699,#16700,#16701,#16702,#16703,
#16704,#16705,#16706,#16707,#16708,#16709,#16710,#16711,#16712,#16713,#16714,
#16715,#16716,#16717,#16718,#16719,#16720,#16721,#16722,#16723,#16724,#16725,
#16726,#16727,#16728,#16729,#16730,#16731,#16732,#16733,#16734,#16735,#16736,
#16737,#16738,#16739,#16740,#16741,#16742,#16743,#16744,#16745,#16746,#16747,
#16748,#16749,#16750,#16751,#16752,#16753,#16754,#16755,#16756,#16757,#16758,
#16759,#16760,#16761,#16762,#16763,#16764,#16765,#16766,#16767,#16768,#16769,
#16770,#16771,#16772,#16773,#16774,#16775,#16776,#16777,#16778,#16779,#16780,
#16781,#16782,#16783,#16784,#16785,#16786,#16787,#16788,#16789,#16790),
 .UNSPECIFIED.,.F.,.F.,(4,3,3,3,3,3,3,3,3,3,3,3,3,3,3,3,3,3,3,3,3,3,3,3,
3,3,3,3,3,3,3,3,3,3,3,3,3,3,3,3,3,3,3,3,3,3,3,3,3,3,3,3,3,3,3,3,4),(109.955742875644,
110.04775906347,110.140427565771,110.233832795629,110.275997614303,110.352818811458,
110.429550773672,110.50620975182,110.582811938281,110.659373480162,110.736420698351,
110.812964872995,110.88951915304,110.96609811802,111.043511394933,111.12022287524,
111.197987050456,111.275751225672,111.353333849286,111.430823831495,111.50823680872,
111.585588362221,111.662894029132,111.740176622177,111.817448409121,111.894723408977,
111.972015639915,112.04938031228,112.126781920713,112.204289735321,112.275504837041,
112.356988809996,112.438368174136,112.522621541284,112.603775036455,112.684851714414,
112.765837142205,112.775381642726,112.85639003863,112.937474295461,113.021920333699,
113.103226415406,113.184610205174,113.266114866203,113.275258448411,113.352778156027,
113.430215472643,113.507585997295,113.584905281123,113.662193120441,113.739465144431,
113.816735373775,113.894017825487,113.971363883941,114.048742610616,114.126217904742,
114.192169701311),.UNSPECIFIED.);
#172=B_SPLINE_CURVE_WITH_KNOTS('',3,(#16791,#16792,#16793,#16794,#16795,
#16796,#16797,#16798,#16799,#16800,#16801,#16802,#16803,#16804,#16805,#16806,
#16807,#16808,#16809,#16810,#16811,#16812,#16813,#16814,#16815,#16816,#16817,
#16818,#16819,#16820,#16821,#16822,#16823,#16824,#16825,#16826,#16827,#16828,
#16829,#16830,#16831,#16832,#16833,#16834,#16835,#16836,#16837,#16838,#16839,
#16840,#16841,#16842,#16843,#16844,#16845,#16846,#16847,#16848,#16849,#16850,
#16851,#16852,#16853,#16854,#16855,#16856,#16857,#16858,#16859,#16860,#16861,
#16862,#16863,#16864,#16865,#16866),.UNSPECIFIED.,.F.,.F.,(4,3,3,3,3,3,
3,3,3,3,3,3,3,3,3,3,3,3,3,3,3,3,3,3,3,4),(107.909220824828,107.991682428682,
108.074143366652,108.156603666138,108.239063354535,108.321522459237,108.403981007636,
108.486439027122,108.568896545084,108.655574440744,108.73804122658,108.820506339923,
108.902969890429,108.985431987726,109.067892741428,109.150352261125,109.232810656392,
109.315268036789,109.397734423056,109.48019762507,109.56265808135,109.645116230261,
109.72758183514,109.810041714355,109.892505827719,109.955742875644),
 .UNSPECIFIED.);
#173=B_SPLINE_CURVE_WITH_KNOTS('',3,(#16868,#16869,#16870,#16871,#16872,
#16873,#16874,#16875,#16876,#16877,#16878,#16879,#16880,#16881,#16882,#16883,
#16884,#16885,#16886,#16887,#16888,#16889,#16890,#16891,#16892,#16893,#16894,
#16895,#16896,#16897,#16898,#16899,#16900,#16901,#16902,#16903,#16904,#16905,
#16906,#16907,#16908,#16909,#16910,#16911,#16912,#16913,#16914,#16915,#16916,
#16917,#16918,#16919,#16920,#16921,#16922,#16923,#16924,#16925,#16926,#16927,
#16928,#16929,#16930,#16931,#16932,#16933,#16934,#16935,#16936,#16937,#16938,
#16939,#16940,#16941,#16942,#16943,#16944,#16945,#16946,#16947,#16948,#16949,
#16950,#16951,#16952),.UNSPECIFIED.,.F.,.F.,(4,3,3,3,3,3,3,3,3,3,3,3,3,
3,3,3,3,3,3,3,3,3,3,3,3,3,3,3,4),(107.909426078052,107.986712289755,108.063998718063,
108.141299368798,108.221126933788,108.298533931578,108.379571780168,108.460609628758,
108.542095943191,108.623478025549,108.707561927358,108.788719246211,108.869800029965,
108.950790021998,108.959813632784,109.040826739075,109.121915433348,109.206190984213,
109.287500450603,109.368887351815,109.45039449058,109.459017636809,109.53951051673,
109.619892861137,109.703855364764,109.784009846555,109.864090723313,109.944088707341,
109.955742875644),.UNSPECIFIED.);
#174=B_SPLINE_CURVE_WITH_KNOTS('',3,(#16953,#16954,#16955,#16956,#16957,
#16958,#16959,#16960,#16961,#16962,#16963,#16964,#16965,#16966,#16967,#16968,
#16969,#16970,#16971,#16972,#16973,#16974,#16975,#16976,#16977,#16978,#16979,
#16980,#16981,#16982,#16983,#16984,#16985,#16986,#16987,#16988,#16989,#16990,
#16991,#16992,#16993,#16994,#16995,#16996,#16997,#16998,#16999,#17000,#17001,
#17002,#17003,#17004,#17005,#17006,#17007,#17008,#17009,#17010,#17011,#17012,
#17013,#17014,#17015,#17016,#17017,#17018,#17019,#17020,#17021,#17022,#17023,
#17024,#17025,#17026,#17027,#17028,#17029,#17030,#17031,#17032,#17033,#17034,
#17035,#17036,#17037,#17038,#17039,#17040,#17041,#17042,#17043,#17044,#17045,
#17046,#17047,#17048,#17049,#17050,#17051,#17052,#17053,#17054,#17055,#17056,
#17057,#17058,#17059,#17060,#17061,#17062,#17063,#17064,#17065,#17066,#17067,
#17068,#17069,#17070,#17071,#17072,#17073,#17074,#17075,#17076,#17077,#17078,
#17079,#17080,#17081,#17082,#17083,#17084,#17085,#17086,#17087,#17088,#17089,
#17090,#17091,#17092,#17093,#17094,#17095,#17096,#17097,#17098,#17099,#17100,
#17101,#17102,#17103,#17104,#17105,#17106,#17107,#17108,#17109,#17110,#17111,
#17112,#17113,#17114,#17115,#17116,#17117,#17118),.UNSPECIFIED.,.F.,.F.,
(4,3,3,3,3,3,3,3,3,3,3,3,3,3,3,3,3,3,3,3,3,3,3,3,3,3,3,3,3,3,3,3,3,3,3,
3,3,3,3,3,3,3,3,3,3,3,3,3,3,3,3,3,3,3,3,4),(109.955742875756,110.037633904134,
110.119660663075,110.204101908521,110.286477313102,110.371951478981,110.45742564486,
110.534289029512,110.611058861322,110.68775139731,110.764382832477,110.840969313261,
110.917827355717,110.99438567868,111.070950013353,111.14753492648,111.224609608088,
111.301316428957,111.378575040934,111.455833652911,111.533363849371,111.610806943976,
111.688178578032,111.765494341601,111.842769784379,111.920030666799,111.997285972443,
112.074549742738,112.151836021222,112.229202834014,112.306611168721,112.384132725284,
112.454241660962,112.531771779025,112.609214808341,112.686586390167,112.763902114527,
112.841177531088,112.918438407113,112.99569371846,113.072957506551,113.150243814935,
113.227610676542,113.305019070474,113.382540703346,113.452649669013,113.529500559795,
113.606259420334,113.682926572603,113.759541261625,113.836118100225,113.912671675508,
113.989233366542,114.065798318672,114.142407825684,114.191567845393),
 .UNSPECIFIED.);
#175=B_SPLINE_CURVE_WITH_KNOTS('',3,(#17124,#17125,#17126,#17127,#17128,
#17129,#17130,#17131,#17132,#17133,#17134,#17135,#17136,#17137,#17138,#17139,
#17140,#17141,#17142,#17143,#17144,#17145,#17146,#17147,#17148,#17149,#17150,
#17151,#17152,#17153,#17154,#17155,#17156,#17157,#17158,#17159,#17160,#17161,
#17162,#17163,#17164,#17165,#17166,#17167,#17168,#17169,#17170,#17171,#17172,
#17173,#17174,#17175,#17176,#17177,#17178,#17179,#17180,#17181,#17182,#17183,
#17184,#17185,#17186,#17187,#17188,#17189,#17190,#17191,#17192,#17193,#17194,
#17195,#17196,#17197,#17198,#17199,#17200,#17201,#17202,#17203,#17204,#17205,
#17206,#17207,#17208,#17209,#17210,#17211,#17212,#17213,#17214,#17215,#17216,
#17217,#17218,#17219,#17220,#17221,#17222,#17223,#17224,#17225,#17226,#17227,
#17228,#17229,#17230,#17231,#17232,#17233,#17234,#17235,#17236,#17237,#17238,
#17239,#17240,#17241,#17242,#17243,#17244,#17245,#17246,#17247,#17248,#17249,
#17250,#17251,#17252,#17253,#17254,#17255,#17256,#17257,#17258,#17259,#17260,
#17261,#17262,#17263,#17264,#17265,#17266,#17267,#17268,#17269,#17270,#17271,
#17272,#17273,#17274,#17275,#17276,#17277,#17278,#17279,#17280,#17281,#17282,
#17283,#17284,#17285,#17286,#17287,#17288,#17289,#17290,#17291,#17292,#17293,
#17294,#17295),.UNSPECIFIED.,.F.,.F.,(4,3,3,3,3,3,3,3,3,3,3,3,3,3,3,3,3,
3,3,3,3,3,3,3,3,3,3,3,3,3,3,3,3,3,3,3,3,3,3,3,3,3,3,3,3,3,3,3,3,3,3,3,3,
3,3,3,3,4),(116.238928182824,116.274519282519,116.352036651715,116.429466719167,
116.506825140436,116.584127519651,116.661389420414,116.738636631105,116.815878155324,
116.89312804667,116.970400360813,117.047753432039,117.125147961791,117.202656466753,
117.274272893888,117.351094091043,117.427826053257,117.504485031405,117.581087217866,
117.657648759747,117.734695977936,117.81124015258,117.887794432626,117.964373397605,
118.041786674519,118.118498154826,118.196262330042,118.274026505258,118.351609128872,
118.429099111081,118.506512088306,118.583863641807,118.661169308719,118.738451901764,
118.815723688708,118.892998688564,118.970290919503,119.047655591867,119.1250572003,
119.202565014908,119.273780116627,119.355264089582,119.436643453721,119.520896820869,
119.60205031604,119.683126993999,119.764112421789,119.773656922312,119.854665318216,
119.935749575048,120.020195613285,120.101501694992,120.182885484761,120.264390145789,
120.273533727996,120.351058891167,120.428490576211,120.47615534713),
 .UNSPECIFIED.);
#176=B_SPLINE_CURVE_WITH_KNOTS('',3,(#17296,#17297,#17298,#17299,#17300,
#17301,#17302,#17303,#17304,#17305,#17306,#17307,#17308,#17309,#17310,#17311,
#17312,#17313,#17314,#17315,#17316,#17317,#17318,#17319,#17320,#17321,#17322,
#17323,#17324,#17325,#17326,#17327,#17328,#17329,#17330,#17331,#17332,#17333,
#17334,#17335,#17336,#17337,#17338,#17339,#17340,#17341,#17342,#17343,#17344,
#17345,#17346,#17347,#17348,#17349,#17350,#17351,#17352,#17353,#17354,#17355,
#17356,#17357,#17358,#17359,#17360,#17361,#17362,#17363,#17364,#17365,#17366,
#17367,#17368,#17369,#17370,#17371,#17372,#17373,#17374,#17375,#17376,#17377,
#17378,#17379,#17380),.UNSPECIFIED.,.F.,.F.,(4,3,3,3,3,3,3,3,3,3,3,3,3,
3,3,3,3,3,3,3,3,3,3,3,3,3,3,3,4),(114.192169701311,114.269773263717,114.27501205978,
114.351860682967,114.428615529364,114.505292868769,114.581908908544,114.658479807169,
114.735515540166,114.812057958872,114.888606295434,114.965175126882,115.042572762949,
115.119263843902,115.197014757526,115.27476567115,115.351855019129,115.428857167646,
115.50578817035,115.582664026712,115.659500694152,115.736324251519,115.813143990561,
115.889974319783,115.966829651356,116.043764396594,116.120743639361,116.197826713264,
116.238928182687),.UNSPECIFIED.);
#177=B_SPLINE_CURVE_WITH_KNOTS('',3,(#17382,#17383,#17384,#17385,#17386,
#17387,#17388,#17389,#17390,#17391,#17392,#17393,#17394,#17395,#17396,#17397,
#17398,#17399,#17400,#17401,#17402,#17403,#17404,#17405,#17406,#17407,#17408,
#17409,#17410,#17411,#17412,#17413,#17414,#17415,#17416,#17417,#17418,#17419,
#17420,#17421,#17422,#17423,#17424,#17425,#17426,#17427,#17428,#17429,#17430,
#17431,#17432,#17433,#17434,#17435,#17436,#17437,#17438,#17439,#17440,#17441,
#17442,#17443,#17444,#17445,#17446,#17447,#17448,#17449,#17450,#17451,#17452,
#17453,#17454,#17455,#17456,#17457,#17458,#17459,#17460,#17461,#17462,#17463,
#17464,#17465,#17466),.UNSPECIFIED.,.F.,.F.,(4,3,3,3,3,3,3,3,3,3,3,3,3,
3,3,3,3,3,3,3,3,3,3,3,3,3,3,3,4),(114.191567845393,114.268277197137,114.345039195796,
114.42191142385,114.451057677064,114.528652346498,114.606154612608,114.683580097679,
114.760944369056,114.838262950147,114.915558654618,114.992843699274,115.070132091207,
115.147437836733,115.22481587672,115.302230948465,115.379751562736,115.449465685115,
115.530951999548,115.612334081907,115.696417983715,115.777575302568,115.858656086323,
115.939646078357,115.94866968914,116.024039768399,116.099422917702,116.174874532357,
116.238928182733),.UNSPECIFIED.);
#178=B_SPLINE_CURVE_WITH_KNOTS('',3,(#17467,#17468,#17469,#17470,#17471,
#17472,#17473,#17474,#17475,#17476,#17477,#17478,#17479,#17480,#17481,#17482,
#17483,#17484,#17485,#17486,#17487,#17488,#17489,#17490,#17491,#17492,#17493,
#17494,#17495,#17496,#17497,#17498,#17499,#17500,#17501,#17502,#17503,#17504,
#17505,#17506,#17507,#17508,#17509,#17510,#17511,#17512,#17513,#17514,#17515,
#17516,#17517,#17518,#17519,#17520,#17521,#17522,#17523,#17524,#17525,#17526,
#17527,#17528,#17529,#17530,#17531,#17532,#17533,#17534,#17535,#17536,#17537,
#17538,#17539,#17540,#17541,#17542,#17543,#17544,#17545,#17546,#17547,#17548,
#17549,#17550,#17551,#17552,#17553,#17554,#17555,#17556,#17557,#17558,#17559,
#17560,#17561,#17562,#17563,#17564,#17565,#17566,#17567,#17568,#17569,#17570,
#17571,#17572,#17573,#17574,#17575,#17576,#17577,#17578,#17579,#17580,#17581,
#17582,#17583,#17584,#17585,#17586,#17587,#17588,#17589,#17590,#17591,#17592,
#17593,#17594,#17595,#17596,#17597,#17598,#17599,#17600,#17601,#17602,#17603,
#17604,#17605,#17606,#17607,#17608,#17609,#17610,#17611,#17612,#17613,#17614,
#17615,#17616,#17617,#17618,#17619,#17620,#17621,#17622,#17623,#17624,#17625,
#17626,#17627,#17628,#17629,#17630,#17631,#17632),.UNSPECIFIED.,.F.,.F.,
(4,3,3,3,3,3,3,3,3,3,3,3,3,3,3,3,3,3,3,3,3,3,3,3,3,3,3,3,3,3,3,3,3,3,3,
3,3,3,3,3,3,3,3,3,3,3,3,3,3,3,3,3,3,3,3,4),(116.238928182823,116.343400937995,
116.447873693166,116.525401846375,116.602848721337,116.680229900044,116.757560917505,
116.834857272335,116.912147572671,116.98943748041,117.066741002408,117.144072150535,
117.221491640356,117.298956998778,117.376542385076,117.446281701217,117.523145085869,
117.599914917679,117.676607453668,117.753238888834,117.829825369618,117.906683412074,
117.983241735037,118.05980606971,118.136390982837,118.213465664445,118.290172485314,
118.367431097291,118.444689709268,118.522219905728,118.599663000333,118.677034634389,
118.754350397958,118.831625840736,118.908886723155,118.9861420288,119.063405799094,
119.140692077578,119.21805889037,119.295467225077,119.37298878164,119.443097717319,
119.520627835382,119.598070864698,119.675442446524,119.752758170883,119.830033587445,
119.90729446347,119.984549774816,120.061813562908,120.139099871292,120.216466732898,
120.29387512683,120.371396759702,120.441505725369,120.47591264955),
 .UNSPECIFIED.);
#179=B_SPLINE_CURVE_WITH_KNOTS('',3,(#17638,#17639,#17640,#17641,#17642,
#17643,#17644,#17645,#17646,#17647,#17648,#17649,#17650,#17651,#17652,#17653,
#17654,#17655,#17656,#17657,#17658,#17659,#17660,#17661,#17662,#17663,#17664,
#17665,#17666,#17667,#17668,#17669,#17670,#17671,#17672,#17673,#17674,#17675,
#17676,#17677,#17678,#17679,#17680,#17681,#17682,#17683,#17684,#17685,#17686,
#17687,#17688,#17689,#17690,#17691,#17692,#17693,#17694,#17695,#17696,#17697,
#17698,#17699,#17700,#17701,#17702,#17703,#17704,#17705,#17706,#17707,#17708,
#17709,#17710,#17711,#17712,#17713,#17714,#17715,#17716,#17717,#17718,#17719,
#17720,#17721,#17722,#17723,#17724,#17725,#17726,#17727,#17728,#17729,#17730,
#17731,#17732,#17733,#17734,#17735,#17736,#17737,#17738,#17739,#17740,#17741,
#17742,#17743,#17744,#17745,#17746,#17747,#17748,#17749,#17750,#17751,#17752,
#17753,#17754,#17755,#17756,#17757,#17758,#17759,#17760,#17761,#17762,#17763,
#17764,#17765,#17766,#17767,#17768,#17769,#17770,#17771,#17772,#17773,#17774,
#17775,#17776,#17777,#17778,#17779,#17780,#17781,#17782,#17783,#17784,#17785,
#17786,#17787,#17788,#17789,#17790,#17791,#17792,#17793,#17794),
 .UNSPECIFIED.,.F.,.F.,(4,3,3,3,3,3,3,3,3,3,3,3,3,3,3,3,3,3,3,3,3,3,3,3,
3,3,3,3,3,3,3,3,3,3,3,3,3,3,3,3,3,3,3,3,3,3,3,3,3,3,3,3,4),(122.522113490003,
122.604575696039,122.687037553779,122.769499070073,122.85196025177,122.934421105721,
123.016881638776,123.099341857782,123.18180176959,123.264261381048,123.346720699004,
123.429179730306,123.511638481803,123.594096960342,123.67655517277,123.759013125934,
123.841470826682,123.92392828186,124.006385498314,124.092397724816,124.175722069239,
124.258188674685,124.340654435926,124.423119380379,124.505583535455,124.588046928563,
124.670509587112,124.752971538505,124.835432810143,124.917893429428,125.000353423754,
125.082812820519,125.165271647114,125.247729930931,125.330187699358,125.412644979784,
125.496778215195,125.579244213287,125.661708589642,125.744171453904,125.826632915695,
125.909093084616,125.991552070252,126.074009982169,126.159605827694,126.242070564294,
126.324532336296,126.406991582138,126.489448740115,126.571911258396,126.654368929251,
126.736827719202,126.758776746367),.UNSPECIFIED.);
#180=B_SPLINE_CURVE_WITH_KNOTS('',3,(#17795,#17796,#17797,#17798,#17799,
#17800,#17801,#17802,#17803,#17804,#17805,#17806,#17807,#17808,#17809,#17810,
#17811,#17812,#17813,#17814,#17815,#17816,#17817,#17818,#17819,#17820,#17821,
#17822,#17823,#17824,#17825,#17826,#17827,#17828,#17829,#17830,#17831,#17832,
#17833,#17834,#17835,#17836,#17837,#17838,#17839,#17840,#17841,#17842,#17843,
#17844,#17845,#17846,#17847,#17848,#17849,#17850,#17851,#17852,#17853,#17854,
#17855,#17856,#17857,#17858,#17859,#17860,#17861,#17862,#17863,#17864,#17865,
#17866,#17867,#17868,#17869,#17870,#17871,#17872,#17873,#17874,#17875,#17876),
 .UNSPECIFIED.,.F.,.F.,(4,3,3,3,3,3,3,3,3,3,3,3,3,3,3,3,3,3,3,3,3,3,3,3,
3,3,3,4),(120.47615534713,120.553490920204,120.630785720323,120.711098422703,
120.788373593687,120.865657447954,120.942964006615,121.020307300857,121.097742078208,
121.175230936057,121.252826406552,121.273287339366,121.350135962554,121.42689080895,
121.503568148355,121.58018418813,121.656755086755,121.733790819752,121.810333238458,
121.886881575021,121.963450406469,122.040848042535,122.117539123488,122.195290037111,
122.273040950735,122.376675837801,122.477853026382,122.522113490003),
 .UNSPECIFIED.);
#181=B_SPLINE_CURVE_WITH_KNOTS('',3,(#17878,#17879,#17880,#17881,#17882,
#17883,#17884,#17885,#17886,#17887,#17888,#17889,#17890,#17891,#17892,#17893,
#17894,#17895,#17896,#17897,#17898,#17899,#17900,#17901,#17902,#17903,#17904,
#17905,#17906,#17907,#17908,#17909,#17910,#17911,#17912,#17913,#17914,#17915,
#17916,#17917,#17918,#17919,#17920,#17921,#17922,#17923,#17924,#17925,#17926,
#17927,#17928,#17929,#17930,#17931,#17932,#17933,#17934,#17935,#17936,#17937,
#17938,#17939,#17940,#17941,#17942,#17943,#17944,#17945,#17946,#17947,#17948,
#17949,#17950,#17951,#17952,#17953,#17954,#17955,#17956,#17957,#17958,#17959),
 .UNSPECIFIED.,.F.,.F.,(4,3,3,3,3,3,3,3,3,3,3,3,3,3,3,3,3,3,3,3,3,3,3,3,
3,3,3,4),(120.47591264955,120.55270682257,120.629419256148,120.706066160806,
120.782663694973,120.859227977659,120.935788714438,121.012351541726,121.088931025486,
121.165541739534,121.242242394116,121.318993148849,121.395858281635,121.43991373342,
121.517508402854,121.595010668965,121.672436154035,121.749800425412,121.827119006503,
121.904414710975,121.981699755631,122.058988147564,122.136293893089,122.213671933077,
122.291087004821,122.368607619093,122.438321741471,122.522113490003),
 .UNSPECIFIED.);
#182=B_SPLINE_CURVE_WITH_KNOTS('',3,(#17960,#17961,#17962,#17963,#17964,
#17965,#17966,#17967,#17968,#17969,#17970,#17971,#17972,#17973,#17974,#17975,
#17976,#17977,#17978,#17979,#17980,#17981,#17982,#17983,#17984,#17985,#17986,
#17987,#17988,#17989,#17990,#17991,#17992,#17993,#17994,#17995,#17996,#17997,
#17998,#17999,#18000,#18001,#18002,#18003,#18004,#18005,#18006,#18007,#18008,
#18009,#18010,#18011,#18012,#18013,#18014,#18015,#18016,#18017,#18018,#18019,
#18020,#18021,#18022,#18023,#18024,#18025,#18026,#18027,#18028,#18029,#18030,
#18031,#18032,#18033,#18034,#18035,#18036,#18037,#18038,#18039,#18040,#18041,
#18042,#18043,#18044,#18045,#18046,#18047,#18048,#18049,#18050,#18051,#18052,
#18053,#18054,#18055,#18056,#18057,#18058,#18059,#18060,#18061,#18062,#18063,
#18064,#18065,#18066,#18067,#18068,#18069,#18070,#18071,#18072,#18073,#18074,
#18075,#18076,#18077,#18078,#18079,#18080,#18081,#18082,#18083,#18084,#18085,
#18086,#18087,#18088,#18089,#18090,#18091,#18092,#18093,#18094,#18095,#18096,
#18097,#18098,#18099,#18100,#18101,#18102,#18103,#18104,#18105,#18106,#18107,
#18108,#18109,#18110,#18111,#18112,#18113,#18114,#18115,#18116,#18117,#18118,
#18119,#18120,#18121,#18122,#18123,#18124,#18125,#18126,#18127,#18128,#18129,
#18130,#18131),.UNSPECIFIED.,.F.,.F.,(4,3,3,3,3,3,3,3,3,3,3,3,3,3,3,3,3,
3,3,3,3,3,3,3,3,3,3,3,3,3,3,3,3,3,3,3,3,3,3,3,3,3,3,3,3,3,3,3,3,3,3,3,3,
3,3,3,3,4),(122.522113490138,122.600488126397,122.678775016274,122.756968288714,
122.835107118422,122.913196242504,122.937525745497,123.018538851787,123.099627546061,
123.183903096926,123.265212563315,123.346599464526,123.428106603291,123.436729749522,
123.514257902731,123.591704777692,123.6690859564,123.746416973861,123.823713328691,
123.901003629027,123.978293536765,124.055597058764,124.132928206891,124.210347696712,
124.287813055134,124.365398441432,124.435137757573,124.512001142225,124.588770974035,
124.665463510023,124.74209494519,124.818681425974,124.89553946843,124.972097791393,
125.048662126066,125.125247039194,125.202321720801,125.27902854167,125.356287153647,
125.433545765624,125.511075962084,125.588519056689,125.665890690745,125.743206454314,
125.820481897092,125.897742779511,125.974998085156,126.05226185545,126.129548133934,
126.206914946726,126.284323281433,126.361844837996,126.431953773675,126.509503675387,
126.586943713325,126.664320168059,126.741635992966,126.759271559359),
 .UNSPECIFIED.);
#183=B_SPLINE_CURVE_WITH_KNOTS('',3,(#18137,#18138,#18139,#18140,#18141,
#18142,#18143,#18144,#18145,#18146,#18147,#18148,#18149,#18150,#18151,#18152,
#18153,#18154,#18155,#18156,#18157,#18158,#18159,#18160,#18161,#18162,#18163,
#18164,#18165,#18166,#18167,#18168,#18169,#18170,#18171,#18172,#18173,#18174,
#18175,#18176,#18177,#18178,#18179,#18180,#18181,#18182,#18183,#18184,#18185,
#18186,#18187,#18188,#18189,#18190,#18191,#18192,#18193,#18194,#18195,#18196,
#18197,#18198,#18199,#18200,#18201,#18202,#18203,#18204,#18205,#18206,#18207,
#18208,#18209,#18210,#18211,#18212,#18213,#18214,#18215,#18216,#18217,#18218,
#18219,#18220,#18221,#18222,#18223,#18224,#18225,#18226,#18227,#18228,#18229,
#18230,#18231,#18232,#18233,#18234,#18235,#18236,#18237,#18238,#18239,#18240,
#18241,#18242,#18243,#18244,#18245,#18246,#18247,#18248,#18249,#18250,#18251,
#18252,#18253,#18254,#18255,#18256,#18257,#18258,#18259,#18260,#18261,#18262,
#18263,#18264,#18265,#18266,#18267,#18268,#18269,#18270,#18271,#18272,#18273,
#18274,#18275,#18276,#18277,#18278,#18279,#18280,#18281,#18282,#18283,#18284,
#18285,#18286,#18287,#18288,#18289,#18290,#18291,#18292,#18293,#18294,#18295,
#18296,#18297,#18298,#18299,#18300,#18301,#18302),.UNSPECIFIED.,.F.,.F.,
(4,3,3,3,3,3,3,3,3,3,3,3,3,3,3,3,3,3,3,3,3,3,3,3,3,3,3,3,3,3,3,3,3,3,3,
3,3,3,3,3,3,3,3,3,3,3,3,3,3,3,3,3,3,3,3,4),(128.805298797183,128.886590232838,
128.968013348574,129.049656555529,129.131416007228,129.213377057373,129.271316230321,
129.348833781939,129.426264001358,129.503622544254,129.580925014841,129.658186976791,
129.735434202574,129.812675713781,129.889925564013,129.967197808926,130.044550766897,
130.121945159206,130.199453486874,130.27106984169,130.348587210886,130.426017278337,
130.503375699607,130.580678078822,130.657939979585,130.735187190276,130.812428714494,
130.88967860584,130.966950919984,131.04430399121,131.121698520961,131.199207025924,
131.270823453059,131.347644650214,131.424376612428,131.501035590576,131.577637777037,
131.654199318918,131.731246537107,131.807790711751,131.884344991797,131.960923956776,
132.03833723369,132.115048713996,132.192812889213,132.270577064429,132.348173410429,
132.425674585281,132.503077670776,132.580424226377,132.657728326265,132.735004017898,
132.812281275791,132.889556293537,132.966874340892,133.041412044979),
 .UNSPECIFIED.);
#184=B_SPLINE_CURVE_WITH_KNOTS('',3,(#18303,#18304,#18305,#18306,#18307,
#18308,#18309,#18310,#18311,#18312,#18313,#18314,#18315,#18316,#18317,#18318,
#18319,#18320,#18321,#18322,#18323,#18324,#18325,#18326,#18327,#18328,#18329,
#18330,#18331,#18332,#18333,#18334,#18335,#18336,#18337,#18338,#18339,#18340,
#18341,#18342,#18343,#18344,#18345,#18346,#18347,#18348,#18349,#18350,#18351,
#18352,#18353,#18354,#18355,#18356,#18357,#18358,#18359,#18360,#18361,#18362,
#18363,#18364,#18365,#18366,#18367,#18368,#18369,#18370,#18371,#18372,#18373,
#18374,#18375,#18376,#18377,#18378),.UNSPECIFIED.,.F.,.F.,(4,3,3,3,3,3,
3,3,3,3,3,3,3,3,3,3,3,3,3,3,3,3,3,3,3,4),(126.758776746367,126.841238350221,
126.923699288191,127.006159587677,127.088619276074,127.171078380776,127.253536929175,
127.335994948661,127.418452466623,127.505130362283,127.587597148119,127.670062261462,
127.752525811968,127.834987909265,127.917448662967,127.999908182664,128.082366577931,
128.164823958328,128.247290344595,128.329753546609,128.412214002889,128.4946721518,
128.577137756679,128.659597635894,128.742061749258,128.805298797183),
 .UNSPECIFIED.);
#185=B_SPLINE_CURVE_WITH_KNOTS('',3,(#18380,#18381,#18382,#18383,#18384,
#18385,#18386,#18387,#18388,#18389,#18390,#18391,#18392,#18393,#18394,#18395,
#18396,#18397,#18398,#18399,#18400,#18401,#18402,#18403,#18404,#18405,#18406,
#18407,#18408,#18409,#18410,#18411,#18412,#18413,#18414,#18415,#18416,#18417,
#18418,#18419,#18420,#18421,#18422,#18423,#18424,#18425,#18426,#18427,#18428,
#18429,#18430,#18431,#18432,#18433,#18434,#18435,#18436,#18437,#18438,#18439,
#18440,#18441,#18442,#18443,#18444,#18445,#18446,#18447,#18448,#18449,#18450,
#18451,#18452,#18453,#18454,#18455,#18456,#18457,#18458,#18459,#18460,#18461),
 .UNSPECIFIED.,.F.,.F.,(4,3,3,3,3,3,3,3,3,3,3,3,3,3,3,3,3,3,3,3,3,3,3,3,
3,3,3,4),(126.759271559359,126.836539945911,126.913798313184,126.991054323545,
127.06832201822,127.145615442332,127.222990672096,127.300410320789,127.377938467087,
127.430361781726,127.507197813849,127.583944829576,127.660619067139,127.73723670666,
127.813813883287,127.890683371598,127.967243474121,128.043813771268,128.12040883229,
128.197499071661,128.274226268243,128.35149802901,128.428769789777,128.522902041628,
128.612256050619,128.701233126335,128.789600144613,128.805298797183),
 .UNSPECIFIED.);
#186=B_SPLINE_CURVE_WITH_KNOTS('',3,(#18462,#18463,#18464,#18465,#18466,
#18467,#18468,#18469,#18470,#18471,#18472,#18473,#18474,#18475,#18476,#18477,
#18478,#18479,#18480,#18481,#18482,#18483,#18484,#18485,#18486,#18487,#18488,
#18489,#18490,#18491,#18492,#18493,#18494,#18495,#18496,#18497,#18498,#18499,
#18500,#18501,#18502,#18503,#18504,#18505,#18506,#18507,#18508,#18509,#18510,
#18511,#18512,#18513,#18514,#18515,#18516,#18517,#18518,#18519,#18520,#18521,
#18522,#18523,#18524,#18525,#18526,#18527,#18528,#18529,#18530,#18531,#18532,
#18533,#18534,#18535,#18536,#18537,#18538,#18539,#18540,#18541,#18542,#18543,
#18544,#18545,#18546,#18547,#18548,#18549,#18550,#18551,#18552,#18553,#18554,
#18555,#18556,#18557,#18558,#18559,#18560,#18561,#18562,#18563,#18564,#18565,
#18566,#18567,#18568,#18569,#18570,#18571,#18572,#18573,#18574,#18575,#18576,
#18577,#18578,#18579,#18580,#18581,#18582,#18583,#18584,#18585,#18586,#18587,
#18588,#18589,#18590,#18591,#18592,#18593,#18594,#18595,#18596,#18597,#18598,
#18599,#18600,#18601,#18602,#18603,#18604,#18605,#18606,#18607,#18608,#18609,
#18610,#18611,#18612,#18613,#18614,#18615,#18616,#18617,#18618),
 .UNSPECIFIED.,.F.,.F.,(4,3,3,3,3,3,3,3,3,3,3,3,3,3,3,3,3,3,3,3,3,3,3,3,
3,3,3,3,3,3,3,3,3,3,3,3,3,3,3,3,3,3,3,3,3,3,3,3,3,3,3,3,4),(128.805298797183,
128.887761003219,128.970222860959,129.052684377253,129.13514555895,129.217606412901,
129.300066945956,129.382527164962,129.46498707677,129.547446688228,129.629906006184,
129.712365037486,129.794823788983,129.877282267521,129.959740479949,130.042198433113,
130.124656133861,130.207113589039,130.289570805493,130.375583031995,130.458907376419,
130.541373981864,130.623839743105,130.706304687558,130.788768842634,130.871232235743,
130.953694894291,131.036156845684,131.118618117323,131.201078736607,131.283538730934,
131.365998127698,131.448456954294,131.53091523811,131.613373006538,131.695830286963,
131.779963522374,131.862429520466,131.944893896822,132.027356761084,132.109818222874,
132.192278391796,132.274737377431,132.357195289348,132.442791134873,132.525255871473,
132.607717643475,132.690176889317,132.772634047294,132.855096565576,132.93755423643,
133.020013026381,133.041962053546),.UNSPECIFIED.);
#187=B_SPLINE_CURVE_WITH_KNOTS('',3,(#18624,#18625,#18626,#18627,#18628,
#18629,#18630,#18631,#18632,#18633,#18634,#18635,#18636,#18637,#18638,#18639,
#18640,#18641,#18642,#18643,#18644,#18645,#18646,#18647,#18648,#18649,#18650,
#18651,#18652,#18653,#18654,#18655,#18656,#18657,#18658,#18659,#18660,#18661,
#18662,#18663,#18664,#18665,#18666,#18667,#18668,#18669,#18670,#18671,#18672,
#18673,#18674,#18675,#18676,#18677,#18678,#18679,#18680,#18681,#18682,#18683,
#18684,#18685,#18686,#18687,#18688,#18689,#18690,#18691,#18692,#18693,#18694,
#18695,#18696,#18697,#18698,#18699,#18700,#18701,#18702,#18703,#18704,#18705,
#18706,#18707,#18708,#18709,#18710,#18711,#18712,#18713,#18714,#18715,#18716,
#18717,#18718,#18719,#18720,#18721,#18722,#18723,#18724,#18725,#18726,#18727,
#18728,#18729,#18730,#18731,#18732,#18733,#18734,#18735,#18736,#18737,#18738,
#18739,#18740,#18741,#18742,#18743,#18744,#18745,#18746,#18747,#18748,#18749,
#18750,#18751,#18752,#18753,#18754,#18755,#18756,#18757,#18758,#18759,#18760,
#18761,#18762,#18763,#18764,#18765,#18766,#18767,#18768,#18769,#18770,#18771,
#18772,#18773,#18774,#18775,#18776,#18777,#18778,#18779,#18780),
 .UNSPECIFIED.,.F.,.F.,(4,3,3,3,3,3,3,3,3,3,3,3,3,3,3,3,3,3,3,3,3,3,3,3,
3,3,3,3,3,3,3,3,3,3,3,3,3,3,3,3,3,3,3,3,3,3,3,3,3,3,3,3,4),(135.088484104362,
135.170946310398,135.253408168138,135.335869684432,135.418330866129,135.50079172008,
135.583252253135,135.665712472141,135.748172383949,135.830631995407,135.913091313363,
135.995550344665,136.078009096162,136.1604675747,136.242925787128,136.325383740292,
136.40784144104,136.490298896218,136.572756112673,136.658768339175,136.742092683598,
136.824559289043,136.907025050285,136.989489994737,137.071954149813,137.154417542922,
137.236880201471,137.319342152864,137.401803424502,137.484264043786,137.566724038113,
137.649183434878,137.731642261473,137.81410054529,137.896558313717,137.979015594142,
138.063148829554,138.145614827645,138.228079204001,138.310542068263,138.393003530054,
138.475463698975,138.557922684611,138.640380596528,138.725976442053,138.808441178653,
138.890902950655,138.973362196497,139.055819354474,139.138281872755,139.22073954361,
139.303198333561,139.325147360726),.UNSPECIFIED.);
#188=B_SPLINE_CURVE_WITH_KNOTS('',3,(#18781,#18782,#18783,#18784,#18785,
#18786,#18787,#18788,#18789,#18790,#18791,#18792,#18793,#18794,#18795,#18796,
#18797,#18798,#18799,#18800,#18801,#18802,#18803,#18804,#18805,#18806,#18807,
#18808,#18809,#18810,#18811,#18812,#18813,#18814,#18815,#18816,#18817,#18818,
#18819,#18820,#18821,#18822,#18823,#18824,#18825,#18826,#18827,#18828,#18829,
#18830,#18831,#18832,#18833,#18834,#18835,#18836,#18837,#18838,#18839,#18840,
#18841,#18842,#18843,#18844,#18845,#18846,#18847,#18848,#18849,#18850,#18851,
#18852,#18853,#18854,#18855,#18856,#18857,#18858,#18859,#18860,#18861,#18862,
#18863,#18864,#18865),.UNSPECIFIED.,.F.,.F.,(4,3,3,3,3,3,3,3,3,3,3,3,3,
3,3,3,3,3,3,3,3,3,3,3,3,3,3,3,4),(133.041412044979,133.118812100158,133.19631907369,
133.270330675798,133.351814648753,133.433194012892,133.51744738004,133.598600875211,
133.67967755317,133.76066298096,133.770207481483,133.851215877387,133.932300134219,
134.016746172456,134.098052254163,134.179436043931,134.26094070496,134.270084287167,
134.346164168423,134.42216215834,134.498094981456,134.573978218577,134.649834970144,
134.725680252268,134.801529071145,134.877429864499,134.953357532579,135.029372167759,
135.087670040789),.UNSPECIFIED.);
#189=B_SPLINE_CURVE_WITH_KNOTS('',3,(#18867,#18868,#18869,#18870,#18871,
#18872,#18873,#18874,#18875,#18876,#18877,#18878,#18879,#18880,#18881,#18882,
#18883,#18884,#18885,#18886,#18887,#18888,#18889,#18890,#18891,#18892,#18893,
#18894,#18895,#18896,#18897,#18898,#18899,#18900,#18901,#18902,#18903,#18904,
#18905,#18906,#18907,#18908,#18909,#18910,#18911,#18912,#18913,#18914,#18915,
#18916,#18917,#18918,#18919,#18920,#18921,#18922,#18923,#18924,#18925,#18926,
#18927,#18928,#18929,#18930,#18931,#18932,#18933,#18934,#18935,#18936,#18937,
#18938,#18939,#18940,#18941,#18942),.UNSPECIFIED.,.F.,.F.,(4,3,3,3,3,3,
3,3,3,3,3,3,3,3,3,3,3,3,3,3,3,3,3,3,3,4),(133.041962053546,133.1244236574,
133.206884595371,133.289344894856,133.371804583253,133.454263687955,133.536722236354,
133.619180255841,133.701637773802,133.788315669462,133.870782455298,133.953247568642,
134.035711119147,134.118173216444,134.200633970146,134.283093489843,134.365551885111,
134.448009265508,134.530475651774,134.612938853788,134.695399310068,134.777857458979,
134.860323063858,134.942782943073,135.025247056437,135.088484104362),
 .UNSPECIFIED.);
#190=B_SPLINE_CURVE_WITH_KNOTS('',3,(#18943,#18944,#18945,#18946,#18947,
#18948,#18949,#18950,#18951,#18952,#18953,#18954,#18955,#18956,#18957,#18958,
#18959,#18960,#18961,#18962,#18963,#18964,#18965,#18966,#18967,#18968,#18969,
#18970,#18971,#18972,#18973,#18974,#18975,#18976,#18977,#18978,#18979,#18980,
#18981,#18982,#18983,#18984,#18985,#18986,#18987,#18988,#18989,#18990,#18991,
#18992,#18993,#18994,#18995,#18996,#18997,#18998,#18999,#19000,#19001,#19002,
#19003,#19004,#19005,#19006,#19007,#19008,#19009,#19010,#19011,#19012,#19013,
#19014,#19015,#19016,#19017,#19018,#19019,#19020,#19021,#19022,#19023,#19024,
#19025,#19026,#19027,#19028,#19029,#19030,#19031,#19032,#19033,#19034,#19035,
#19036,#19037,#19038,#19039,#19040,#19041,#19042,#19043,#19044,#19045,#19046,
#19047,#19048,#19049,#19050,#19051,#19052,#19053,#19054,#19055,#19056,#19057,
#19058,#19059,#19060,#19061,#19062,#19063,#19064,#19065,#19066,#19067,#19068,
#19069,#19070,#19071,#19072,#19073,#19074,#19075,#19076,#19077,#19078,#19079,
#19080,#19081,#19082,#19083,#19084,#19085,#19086,#19087,#19088,#19089,#19090,
#19091,#19092,#19093,#19094,#19095,#19096,#19097,#19098,#19099,#19100,#19101,
#19102,#19103,#19104,#19105,#19106,#19107,#19108,#19109,#19110,#19111),
 .UNSPECIFIED.,.F.,.F.,(4,3,3,3,3,3,3,3,3,3,3,3,3,3,3,3,3,3,3,3,3,3,3,3,
3,3,3,3,3,3,3,3,3,3,3,3,3,3,3,3,3,3,3,3,3,3,3,3,3,3,3,3,3,3,3,3,4),(135.088484104362,
135.17791010341,135.267858742395,135.358486777205,135.417625846133,135.495220515567,
135.572722781677,135.650148266748,135.727512538125,135.804831119216,135.882126823688,
135.959411868344,136.036700260277,136.114006005803,136.19138404579,136.268799117535,
136.346319731806,136.416033854184,136.497520168617,136.578902250976,136.662986152784,
136.744143471637,136.825224255392,136.906214247426,136.91523785821,136.9962509645,
137.077339658773,137.161615209639,137.242924676028,137.324311577239,137.405818716004,
137.414441862235,137.491970015444,137.569416890405,137.646798069113,137.724129086573,
137.801425441404,137.87871574174,137.956005649478,138.033309171476,138.110640319603,
138.188059809424,138.265525167846,138.343110554144,138.412849870286,138.489718235985,
138.566492041822,138.643187549574,138.719820957949,138.796408239568,138.87297091787,
138.949523565454,139.026080746546,139.102691812507,139.179329837236,139.256058308962,
139.324627500385),.UNSPECIFIED.);
#191=B_SPLINE_CURVE_WITH_KNOTS('',3,(#19117,#19118,#19119,#19120,#19121,
#19122,#19123,#19124,#19125,#19126,#19127,#19128,#19129,#19130,#19131,#19132,
#19133,#19134,#19135,#19136,#19137,#19138,#19139,#19140,#19141,#19142,#19143,
#19144,#19145,#19146,#19147,#19148,#19149,#19150,#19151,#19152,#19153,#19154,
#19155,#19156,#19157,#19158,#19159,#19160,#19161,#19162,#19163,#19164,#19165,
#19166,#19167,#19168,#19169,#19170,#19171,#19172,#19173,#19174,#19175,#19176,
#19177,#19178,#19179,#19180,#19181,#19182,#19183,#19184,#19185,#19186,#19187,
#19188,#19189,#19190,#19191,#19192,#19193,#19194,#19195,#19196,#19197,#19198,
#19199,#19200,#19201,#19202,#19203,#19204,#19205,#19206,#19207,#19208,#19209,
#19210,#19211,#19212,#19213,#19214,#19215,#19216,#19217,#19218,#19219,#19220,
#19221,#19222,#19223,#19224,#19225,#19226,#19227,#19228,#19229,#19230,#19231,
#19232,#19233,#19234,#19235,#19236,#19237,#19238,#19239,#19240,#19241,#19242,
#19243,#19244,#19245,#19246,#19247,#19248,#19249,#19250,#19251,#19252,#19253,
#19254,#19255,#19256,#19257,#19258,#19259,#19260,#19261,#19262,#19263,#19264,
#19265,#19266,#19267,#19268,#19269,#19270,#19271,#19272,#19273,#19274,#19275,
#19276,#19277,#19278,#19279,#19280,#19281,#19282,#19283,#19284,#19285),
 .UNSPECIFIED.,.F.,.F.,(4,3,3,3,3,3,3,3,3,3,3,3,3,3,3,3,3,3,3,3,3,3,3,3,
3,3,3,3,3,3,3,3,3,3,3,3,3,3,3,3,3,3,3,3,3,3,3,3,3,3,3,3,3,3,3,3,4),(141.372263151081,
141.448917194025,141.525499836524,141.602027358791,141.6785159959,141.754993398329,
141.831467912504,141.907954196066,141.984466911852,142.061064659906,142.137708459711,
142.214465870369,142.268113178122,142.344961801309,142.421716647706,142.498393987111,
142.575010026885,142.65158092551,142.728616658508,142.805159077214,142.881707413776,
142.958276245224,143.035673881291,143.112364962244,143.190115875868,143.267866789492,
143.34538434111,143.42281456053,143.500173103425,143.577475574013,143.654737535963,
143.731984761746,143.809226272953,143.886476123186,143.963748368098,144.041101326069,
144.118495718378,144.196004046047,144.267620400861,144.345137770057,144.422567837509,
144.499926258778,144.577228637993,144.654490538756,144.731737749447,144.808979273666,
144.886229165012,144.963501479155,145.040854550381,145.118249080132,145.195757585095,
145.267374012231,145.344213795142,145.42094068026,145.497602569752,145.57420299272,
145.608744731738),.UNSPECIFIED.);
#192=B_SPLINE_CURVE_WITH_KNOTS('',3,(#19286,#19287,#19288,#19289,#19290,
#19291,#19292,#19293,#19294,#19295,#19296,#19297,#19298,#19299,#19300,#19301,
#19302,#19303,#19304,#19305,#19306,#19307,#19308,#19309,#19310,#19311,#19312,
#19313,#19314,#19315,#19316,#19317,#19318,#19319,#19320,#19321,#19322,#19323,
#19324,#19325,#19326,#19327,#19328,#19329,#19330,#19331,#19332,#19333,#19334,
#19335,#19336,#19337,#19338,#19339,#19340,#19341,#19342,#19343,#19344,#19345,
#19346,#19347,#19348,#19349,#19350,#19351,#19352,#19353,#19354,#19355,#19356,
#19357,#19358,#19359,#19360,#19361),.UNSPECIFIED.,.F.,.F.,(4,3,3,3,3,3,
3,3,3,3,3,3,3,3,3,3,3,3,3,3,3,3,3,3,3,4),(139.325147360726,139.40760896458,
139.49006990255,139.572530202036,139.654989890433,139.737448995135,139.819907543534,
139.90236556302,139.984823080982,140.071500976642,140.153967762478,140.236432875821,
140.318896426327,140.401358523624,140.483819277326,140.566278797023,140.64873719229,
140.731194572688,140.813660958954,140.896124160968,140.978584617248,141.061042766159,
141.143508371038,141.225968250253,141.308432363617,141.371669411542),
 .UNSPECIFIED.);
#193=B_SPLINE_CURVE_WITH_KNOTS('',3,(#19363,#19364,#19365,#19366,#19367,
#19368,#19369,#19370,#19371,#19372,#19373,#19374,#19375,#19376,#19377,#19378,
#19379,#19380,#19381,#19382,#19383,#19384,#19385,#19386,#19387,#19388,#19389,
#19390,#19391,#19392,#19393,#19394,#19395,#19396,#19397,#19398,#19399,#19400,
#19401,#19402,#19403,#19404,#19405,#19406,#19407,#19408,#19409,#19410,#19411,
#19412,#19413,#19414,#19415,#19416,#19417,#19418,#19419,#19420,#19421,#19422,
#19423,#19424,#19425,#19426,#19427,#19428,#19429,#19430,#19431,#19432,#19433,
#19434,#19435,#19436,#19437,#19438,#19439,#19440,#19441,#19442,#19443,#19444,
#19445,#19446,#19447),.UNSPECIFIED.,.F.,.F.,(4,3,3,3,3,3,3,3,3,3,3,3,3,
3,3,3,3,3,3,3,3,3,3,3,3,3,3,3,4),(139.324627500385,139.401481316582,139.411257878337,
139.488788074797,139.566231169402,139.643602803458,139.720918567027,139.798194009805,
139.875454892224,139.952710197869,140.029973968163,140.107260246647,140.18462705944,
140.262035394147,140.33955695071,140.409665886388,140.48672274472,140.563692688849,
140.640591798251,140.717436098154,140.794241571758,140.871034465617,140.947823924016,
141.024624379267,141.101450267632,141.178355915937,141.255306485282,141.332360681074,
141.371669411465),.UNSPECIFIED.);
#194=B_SPLINE_CURVE_WITH_KNOTS('',3,(#19448,#19449,#19450,#19451,#19452,
#19453,#19454,#19455,#19456,#19457,#19458,#19459,#19460,#19461,#19462,#19463,
#19464,#19465,#19466,#19467,#19468,#19469,#19470,#19471,#19472,#19473,#19474,
#19475,#19476,#19477,#19478,#19479,#19480,#19481,#19482,#19483,#19484,#19485,
#19486,#19487,#19488,#19489,#19490,#19491,#19492,#19493,#19494,#19495,#19496,
#19497,#19498,#19499,#19500,#19501,#19502,#19503,#19504,#19505,#19506,#19507,
#19508,#19509,#19510,#19511,#19512,#19513,#19514,#19515,#19516,#19517,#19518,
#19519,#19520,#19521,#19522,#19523,#19524,#19525,#19526,#19527,#19528,#19529,
#19530,#19531,#19532,#19533,#19534,#19535,#19536,#19537,#19538,#19539,#19540,
#19541,#19542,#19543,#19544,#19545,#19546,#19547,#19548,#19549,#19550,#19551,
#19552,#19553,#19554,#19555,#19556,#19557,#19558,#19559,#19560,#19561,#19562,
#19563,#19564,#19565,#19566,#19567,#19568,#19569,#19570,#19571,#19572,#19573,
#19574,#19575,#19576,#19577,#19578,#19579,#19580,#19581,#19582,#19583,#19584,
#19585,#19586,#19587,#19588,#19589,#19590,#19591,#19592,#19593,#19594,#19595,
#19596,#19597,#19598,#19599,#19600,#19601,#19602,#19603,#19604,#19605,#19606,
#19607,#19608,#19609,#19610,#19611,#19612,#19613,#19614,#19615,#19616,#19617,
#19618,#19619),.UNSPECIFIED.,.F.,.F.,(4,3,3,3,3,3,3,3,3,3,3,3,3,3,3,3,3,
3,3,3,3,3,3,3,3,3,3,3,3,3,3,3,3,3,3,3,3,3,3,3,3,3,3,3,3,3,3,3,3,3,3,3,3,
3,3,3,3,4),(141.371669411542,141.408073894439,141.484909926562,141.561656942289,
141.638331179852,141.714948819374,141.791525996001,141.868395484312,141.944955586835,
142.021525883982,142.098120945005,142.175211184376,142.251938380958,142.329210141724,
142.40648190249,142.484076571924,142.561578838034,142.639004323105,142.716368594482,
142.793687175573,142.870982880044,142.9482679247,143.025556316633,143.102862062159,
143.180240102146,143.257655173891,143.335175788162,143.404889910541,143.486376224974,
143.567758307333,143.651842209141,143.732999527994,143.814080311748,143.895070303782,
143.904093914566,143.985107020856,144.066195715129,144.150471265995,144.231780732384,
144.313167633595,144.39467477236,144.403297918591,144.4808260718,144.558272946762,
144.635654125469,144.71298514293,144.79028149776,144.867571798096,144.944861705834,
145.022165227832,145.09949637596,145.176915865781,145.254381224202,145.331966610501,
145.401705926642,145.478579288395,145.555343991007,145.609203979305),
 .UNSPECIFIED.);
#195=B_SPLINE_CURVE_WITH_KNOTS('',3,(#19625,#19626,#19627,#19628,#19629,
#19630,#19631,#19632,#19633,#19634,#19635,#19636,#19637,#19638,#19639,#19640,
#19641,#19642,#19643,#19644,#19645,#19646,#19647,#19648,#19649,#19650,#19651,
#19652,#19653,#19654,#19655,#19656,#19657,#19658,#19659,#19660,#19661,#19662,
#19663,#19664,#19665,#19666,#19667,#19668,#19669,#19670,#19671,#19672,#19673,
#19674,#19675,#19676,#19677,#19678,#19679,#19680,#19681,#19682,#19683,#19684,
#19685,#19686,#19687,#19688,#19689,#19690,#19691,#19692,#19693,#19694,#19695,
#19696,#19697,#19698,#19699,#19700,#19701,#19702,#19703,#19704,#19705,#19706,
#19707,#19708,#19709,#19710,#19711,#19712,#19713,#19714,#19715,#19716,#19717,
#19718,#19719,#19720,#19721,#19722,#19723,#19724,#19725,#19726,#19727,#19728,
#19729,#19730,#19731,#19732,#19733,#19734,#19735,#19736,#19737,#19738,#19739,
#19740,#19741,#19742,#19743,#19744,#19745,#19746,#19747,#19748,#19749,#19750,
#19751,#19752,#19753,#19754,#19755,#19756,#19757,#19758,#19759,#19760,#19761,
#19762,#19763,#19764,#19765,#19766,#19767,#19768,#19769,#19770,#19771,#19772,
#19773,#19774,#19775,#19776,#19777,#19778,#19779,#19780,#19781),
 .UNSPECIFIED.,.F.,.F.,(4,3,3,3,3,3,3,3,3,3,3,3,3,3,3,3,3,3,3,3,3,3,3,3,
3,3,3,3,3,3,3,3,3,3,3,3,3,3,3,3,3,3,3,3,3,3,3,3,3,3,3,3,4),(147.654854718721,
147.737316924757,147.819778782497,147.902240298791,147.984701480488,148.067162334439,
148.149622867494,148.2320830865,148.314542998308,148.397002609766,148.479461927722,
148.561920959024,148.644379710521,148.726838189059,148.809296401487,148.891754354652,
148.974212055399,149.056669510577,149.139126727032,149.225138953534,149.308463297957,
149.390929903402,149.473395664644,149.555860609096,149.638324764172,149.720788157281,
149.80325081583,149.885712767223,149.968174038861,150.050634658146,150.133094652472,
150.215554049237,150.298012875832,150.380471159649,150.462928928076,150.545386208501,
150.629519443913,150.711985442004,150.79444981836,150.876912682622,150.959374144413,
151.041834313334,151.124293298969,151.206751210887,151.292347056411,151.374811793012,
151.457273565014,151.539732810856,151.622189968833,151.704652487114,151.787110157969,
151.86956894792,151.891517975085),.UNSPECIFIED.);
#196=B_SPLINE_CURVE_WITH_KNOTS('',3,(#19782,#19783,#19784,#19785,#19786,
#19787,#19788,#19789,#19790,#19791,#19792,#19793,#19794,#19795,#19796,#19797,
#19798,#19799,#19800,#19801,#19802,#19803,#19804,#19805,#19806,#19807,#19808,
#19809,#19810,#19811,#19812,#19813,#19814,#19815,#19816,#19817,#19818,#19819,
#19820,#19821,#19822,#19823,#19824,#19825,#19826,#19827,#19828,#19829,#19830,
#19831,#19832,#19833,#19834,#19835,#19836,#19837,#19838,#19839,#19840,#19841,
#19842,#19843,#19844,#19845,#19846,#19847,#19848,#19849,#19850,#19851,#19852,
#19853,#19854,#19855,#19856,#19857,#19858,#19859,#19860,#19861,#19862,#19863),
 .UNSPECIFIED.,.F.,.F.,(4,3,3,3,3,3,3,3,3,3,3,3,3,3,3,3,3,3,3,3,3,3,3,3,
3,3,3,4),(145.608744731738,145.685293209367,145.761838066389,145.838384935465,
145.914948392851,145.99154302266,146.06822781809,146.144962671921,146.221812557441,
146.2671276236,146.344710247214,146.422200229423,146.499613206648,146.576964760148,
146.654270427059,146.731553020104,146.808824807048,146.886099806905,146.963392037843,
147.040756710208,147.11815831864,147.195666133248,147.266881234969,147.352578401241,
147.438023806837,147.523300561661,147.608298891338,147.654854718721),
 .UNSPECIFIED.);
#197=B_SPLINE_CURVE_WITH_KNOTS('',3,(#19865,#19866,#19867,#19868,#19869,
#19870,#19871,#19872,#19873,#19874,#19875,#19876,#19877,#19878,#19879,#19880,
#19881,#19882,#19883,#19884,#19885,#19886,#19887,#19888,#19889,#19890,#19891,
#19892,#19893,#19894,#19895,#19896,#19897,#19898,#19899,#19900,#19901,#19902,
#19903,#19904,#19905,#19906,#19907,#19908,#19909,#19910,#19911,#19912,#19913,
#19914,#19915,#19916,#19917,#19918,#19919,#19920,#19921,#19922,#19923,#19924,
#19925,#19926,#19927,#19928,#19929,#19930,#19931,#19932,#19933,#19934,#19935,
#19936,#19937,#19938,#19939,#19940,#19941,#19942,#19943,#19944,#19945,#19946),
 .UNSPECIFIED.,.F.,.F.,(4,3,3,3,3,3,3,3,3,3,3,3,3,3,3,3,3,3,3,3,3,3,3,3,
3,3,3,4),(145.609203979305,145.685851916934,145.762450096981,145.842158076695,
145.918717225157,145.995278590263,146.071856737559,146.148466240428,146.225160926237,
146.301905983306,146.378753985428,146.400113934693,146.477644131153,146.555087225758,
146.632458859814,146.709774623383,146.787050066161,146.864310948581,146.941566254225,
147.018830024519,147.096116303004,147.173483115796,147.250891450503,147.328413007066,
147.398521942744,147.497828613867,147.595438794475,147.654854718574),
 .UNSPECIFIED.);
#198=B_SPLINE_CURVE_WITH_KNOTS('',3,(#19947,#19948,#19949,#19950,#19951,
#19952,#19953,#19954,#19955,#19956,#19957,#19958,#19959,#19960,#19961,#19962,
#19963,#19964,#19965,#19966,#19967,#19968,#19969,#19970,#19971,#19972,#19973,
#19974,#19975,#19976,#19977,#19978,#19979,#19980,#19981,#19982,#19983,#19984,
#19985,#19986,#19987,#19988,#19989,#19990,#19991,#19992,#19993,#19994,#19995,
#19996,#19997,#19998,#19999,#20000,#20001,#20002,#20003,#20004,#20005,#20006,
#20007,#20008,#20009,#20010,#20011,#20012,#20013,#20014,#20015,#20016,#20017,
#20018,#20019,#20020,#20021,#20022,#20023,#20024,#20025,#20026,#20027,#20028,
#20029,#20030,#20031,#20032,#20033,#20034,#20035,#20036,#20037,#20038,#20039,
#20040,#20041,#20042,#20043,#20044,#20045,#20046,#20047,#20048,#20049,#20050,
#20051,#20052,#20053,#20054,#20055,#20056,#20057,#20058,#20059,#20060,#20061,
#20062,#20063,#20064,#20065,#20066,#20067,#20068,#20069,#20070,#20071,#20072,
#20073,#20074,#20075,#20076,#20077,#20078,#20079,#20080,#20081,#20082,#20083,
#20084,#20085,#20086,#20087,#20088,#20089,#20090,#20091,#20092,#20093,#20094,
#20095,#20096,#20097,#20098,#20099,#20100,#20101,#20102,#20103,#20104,#20105,
#20106,#20107,#20108,#20109,#20110,#20111,#20112,#20113,#20114,#20115,#20116,
#20117,#20118),.UNSPECIFIED.,.F.,.F.,(4,3,3,3,3,3,3,3,3,3,3,3,3,3,3,3,3,
3,3,3,3,3,3,3,3,3,3,3,3,3,3,3,3,3,3,3,3,3,3,3,3,3,3,3,3,3,3,3,3,3,3,3,3,
3,3,3,3,4),(147.654854718721,147.73146308114,147.808029341825,147.884579267218,
147.961123174402,148.037675664688,148.114251342376,148.190906657983,148.267605147702,
148.34441194142,148.396929950795,148.473765982918,148.550512998645,148.627187236208,
148.70380487573,148.780382052357,148.857251540668,148.933811643191,149.010381940338,
149.08697700136,149.164067240732,149.240794437313,149.31806619808,149.395337958846,
149.47293262828,149.55043489439,149.627860379461,149.705224650838,149.782543231928,
149.8598389364,149.937123981056,150.014412372988,150.091718118514,150.169096158502,
150.246511230246,150.324031844517,150.393745966897,150.47523228133,150.556614363689,
150.640698265497,150.72185558435,150.802936368105,150.883926360138,150.892949970922,
150.973963077213,151.055051771486,151.139327322352,151.220636788742,151.302023689953,
151.383530828717,151.392153974948,151.469682119129,151.547131796174,151.624517128286,
151.701846132548,151.779142456503,151.856423902883,151.891456894454),
 .UNSPECIFIED.);
#199=B_SPLINE_CURVE_WITH_KNOTS('',3,(#20124,#20125,#20126,#20127,#20128,
#20129,#20130,#20131,#20132,#20133,#20134,#20135,#20136,#20137,#20138,#20139,
#20140,#20141,#20142,#20143,#20144,#20145,#20146,#20147,#20148,#20149,#20150,
#20151,#20152,#20153,#20154,#20155,#20156,#20157,#20158,#20159,#20160,#20161,
#20162,#20163,#20164,#20165,#20166,#20167,#20168,#20169,#20170,#20171,#20172,
#20173,#20174,#20175,#20176,#20177,#20178,#20179,#20180,#20181,#20182,#20183,
#20184,#20185,#20186,#20187,#20188,#20189,#20190,#20191,#20192,#20193,#20194,
#20195,#20196,#20197,#20198,#20199,#20200,#20201,#20202,#20203,#20204,#20205,
#20206,#20207,#20208,#20209,#20210,#20211,#20212,#20213,#20214,#20215,#20216,
#20217,#20218,#20219,#20220,#20221,#20222,#20223,#20224,#20225,#20226,#20227,
#20228,#20229,#20230,#20231,#20232,#20233,#20234,#20235,#20236,#20237,#20238,
#20239,#20240,#20241,#20242,#20243,#20244,#20245,#20246,#20247,#20248,#20249,
#20250,#20251,#20252,#20253,#20254,#20255,#20256,#20257,#20258,#20259,#20260,
#20261,#20262,#20263,#20264,#20265,#20266,#20267,#20268,#20269,#20270,#20271,
#20272,#20273,#20274,#20275,#20276,#20277,#20278,#20279,#20280,#20281,#20282,
#20283,#20284,#20285,#20286,#20287,#20288,#20289,#20290,#20291,#20292),
 .UNSPECIFIED.,.F.,.F.,(4,3,3,3,3,3,3,3,3,3,3,3,3,3,3,3,3,3,3,3,3,3,3,3,
3,3,3,3,3,3,3,3,3,3,3,3,3,3,3,3,3,3,3,3,3,3,3,3,3,3,3,3,3,3,3,3,4),(153.938040025901,
154.026398361422,154.115124679214,154.204323905769,154.265156514555,154.34664048751,
154.428019851649,154.512273218797,154.593426713968,154.674503391927,154.755488819716,
154.76503332024,154.846041716144,154.927125972976,155.011572011213,155.09287809292,
155.174261882689,155.255766543717,155.264910125924,155.342425904187,155.419860204598,
155.497228623025,155.574546708175,155.65182997222,155.729107056531,155.806383637019,
155.883673732416,155.960991366421,156.038397572745,156.115849582059,156.193422390381,
156.264663737294,156.341512360481,156.418267206878,156.494944546283,156.571560586058,
156.648131484683,156.72516721768,156.801709636386,156.878257972948,156.954826804396,
157.032224440463,157.108915521415,157.186666435039,157.264417348663,157.341939624551,
157.419373573263,157.496734854269,157.574039074757,157.651302890406,157.728545527247,
157.805781044169,157.883023493393,157.960320239351,158.037645216973,158.115056529675,
158.174289778564),.UNSPECIFIED.);
#200=B_SPLINE_CURVE_WITH_KNOTS('',3,(#20293,#20294,#20295,#20296,#20297,
#20298,#20299,#20300,#20301,#20302,#20303,#20304,#20305,#20306,#20307,#20308,
#20309,#20310,#20311,#20312,#20313,#20314,#20315,#20316,#20317,#20318,#20319,
#20320,#20321,#20322,#20323,#20324,#20325,#20326,#20327,#20328,#20329,#20330,
#20331,#20332,#20333,#20334,#20335,#20336,#20337,#20338,#20339,#20340,#20341,
#20342,#20343,#20344,#20345,#20346,#20347,#20348,#20349,#20350,#20351,#20352,
#20353,#20354,#20355,#20356,#20357,#20358,#20359,#20360,#20361,#20362,#20363,
#20364,#20365,#20366,#20367,#20368),.UNSPECIFIED.,.F.,.F.,(4,3,3,3,3,3,
3,3,3,3,3,3,3,3,3,3,3,3,3,3,3,3,3,3,3,4),(151.891517975085,151.973979578939,
152.056440516909,152.138900816395,152.221360504792,152.303819609494,152.386278157893,
152.46873617738,152.551193695341,152.637871591001,152.720338376837,152.80280349018,
152.885267040686,152.967729137983,153.050189891685,153.132649411382,153.215107806649,
153.297565187046,153.380031573313,153.462494775327,153.544955231607,153.627413380518,
153.709878985397,153.792338864612,153.874802977975,153.938040025901),
 .UNSPECIFIED.);
#201=B_SPLINE_CURVE_WITH_KNOTS('',3,(#20370,#20371,#20372,#20373,#20374,
#20375,#20376,#20377,#20378,#20379,#20380,#20381,#20382,#20383,#20384,#20385,
#20386,#20387,#20388,#20389,#20390,#20391,#20392,#20393,#20394,#20395,#20396,
#20397,#20398,#20399,#20400,#20401,#20402,#20403,#20404,#20405,#20406,#20407,
#20408,#20409,#20410,#20411,#20412,#20413,#20414,#20415,#20416,#20417,#20418,
#20419,#20420,#20421,#20422,#20423,#20424,#20425,#20426,#20427,#20428,#20429,
#20430,#20431,#20432,#20433,#20434,#20435,#20436,#20437,#20438,#20439,#20440,
#20441,#20442,#20443,#20444,#20445,#20446,#20447,#20448,#20449,#20450,#20451),
 .UNSPECIFIED.,.F.,.F.,(4,3,3,3,3,3,3,3,3,3,3,3,3,3,3,3,3,3,3,3,3,3,3,3,
3,3,3,4),(151.891456894454,151.968751236879,152.046065543027,152.123413829604,
152.200852531408,152.27834282066,152.355943247076,152.390561982999,152.467425367651,
152.544195199461,152.620887735449,152.697519170616,152.774105651399,152.850963693856,
152.927522016819,153.004086351492,153.080671264619,153.157745946227,153.234452767096,
153.311711379073,153.38896999105,153.469176480459,153.549273741512,153.629271620513,
153.709148776534,153.788955061789,153.868679826393,153.938040025901),
 .UNSPECIFIED.);
#202=B_SPLINE_CURVE_WITH_KNOTS('',3,(#20452,#20453,#20454,#20455,#20456,
#20457,#20458,#20459,#20460,#20461,#20462,#20463,#20464,#20465,#20466,#20467,
#20468,#20469,#20470,#20471,#20472,#20473,#20474,#20475,#20476,#20477,#20478,
#20479,#20480,#20481,#20482,#20483,#20484,#20485,#20486,#20487,#20488,#20489,
#20490,#20491,#20492,#20493,#20494,#20495,#20496,#20497,#20498,#20499,#20500,
#20501,#20502,#20503,#20504,#20505,#20506,#20507,#20508,#20509,#20510,#20511,
#20512,#20513,#20514,#20515,#20516,#20517,#20518,#20519,#20520,#20521,#20522,
#20523,#20524,#20525,#20526,#20527,#20528,#20529,#20530,#20531,#20532,#20533,
#20534,#20535,#20536,#20537,#20538,#20539,#20540,#20541,#20542,#20543,#20544,
#20545,#20546,#20547,#20548,#20549,#20550,#20551,#20552,#20553,#20554,#20555,
#20556,#20557,#20558,#20559,#20560,#20561,#20562,#20563,#20564,#20565,#20566,
#20567,#20568,#20569,#20570,#20571,#20572,#20573,#20574,#20575,#20576,#20577,
#20578,#20579,#20580,#20581,#20582,#20583,#20584,#20585,#20586,#20587,#20588,
#20589,#20590,#20591,#20592,#20593,#20594,#20595,#20596,#20597,#20598,#20599,
#20600,#20601,#20602,#20603,#20604,#20605,#20606,#20607,#20608,#20609,#20610,
#20611,#20612,#20613,#20614,#20615,#20616,#20617,#20618,#20619,#20620),
 .UNSPECIFIED.,.F.,.F.,(4,3,3,3,3,3,3,3,3,3,3,3,3,3,3,3,3,3,3,3,3,3,3,3,
3,3,3,3,3,3,3,3,3,3,3,3,3,3,3,3,3,3,3,3,3,3,3,3,3,3,3,3,3,3,3,3,4),(153.93804002599,
154.020503748665,154.103125959518,154.185989566382,154.268982219652,154.352171395724,
154.387377999101,154.464908117164,154.54235114648,154.619722728306,154.697038452665,
154.774313869227,154.851574745252,154.928830056598,155.00609384469,155.083380153074,
155.16074701468,155.238155408612,155.315677041484,155.385786007152,155.462622039275,
155.539369055002,155.616043292565,155.692660932086,155.769238108713,155.846107597024,
155.922667699547,155.999237996694,156.075833057717,156.152923297088,156.229650493669,
156.306922254436,156.384194015202,156.461788684636,156.539290950746,156.616716435817,
156.694080707194,156.771399288285,156.848694992756,156.925980037412,157.003268429345,
157.080574174871,157.157952214858,157.235367286603,157.312887900874,157.382602023253,
157.464088337686,157.545470420045,157.629554321854,157.710711640707,157.791792424462,
157.872782416495,157.881806027279,157.962834259542,158.043923776839,158.12512824495,
158.174223456389),.UNSPECIFIED.);
#203=B_SPLINE_CURVE_WITH_KNOTS('',3,(#20626,#20627,#20628,#20629,#20630,
#20631,#20632,#20633,#20634,#20635,#20636,#20637,#20638,#20639,#20640,#20641,
#20642,#20643,#20644,#20645,#20646,#20647,#20648,#20649,#20650,#20651,#20652,
#20653,#20654,#20655,#20656,#20657,#20658,#20659,#20660,#20661,#20662,#20663,
#20664,#20665,#20666,#20667,#20668,#20669,#20670,#20671,#20672,#20673,#20674,
#20675,#20676,#20677,#20678,#20679,#20680,#20681,#20682,#20683,#20684,#20685,
#20686,#20687,#20688,#20689,#20690,#20691,#20692,#20693,#20694,#20695,#20696,
#20697,#20698,#20699,#20700,#20701,#20702,#20703,#20704,#20705,#20706,#20707,
#20708,#20709,#20710,#20711,#20712,#20713,#20714,#20715,#20716,#20717,#20718,
#20719,#20720,#20721,#20722,#20723,#20724,#20725,#20726,#20727,#20728,#20729,
#20730,#20731,#20732,#20733,#20734,#20735,#20736,#20737,#20738,#20739,#20740,
#20741,#20742,#20743,#20744,#20745,#20746,#20747,#20748,#20749,#20750,#20751,
#20752,#20753,#20754,#20755,#20756,#20757,#20758,#20759,#20760,#20761,#20762,
#20763,#20764,#20765,#20766,#20767,#20768,#20769,#20770,#20771,#20772,#20773,
#20774,#20775,#20776,#20777,#20778,#20779,#20780,#20781,#20782),
 .UNSPECIFIED.,.F.,.F.,(4,3,3,3,3,3,3,3,3,3,3,3,3,3,3,3,3,3,3,3,3,3,3,3,
3,3,3,3,3,3,3,3,3,3,3,3,3,3,3,3,3,3,3,3,3,3,3,3,3,3,3,3,4),(160.221293919461,
160.303756125205,160.386217982658,160.46867949867,160.551140680093,160.633601533774,
160.716062066564,160.798522285313,160.880982196868,160.963441808079,161.045901125793,
161.12836015686,161.210818908127,161.293277386441,161.37573559865,161.458193551602,
161.540651252142,161.623108707119,161.705565923378,161.791576006692,161.874898274903,
161.957364879679,162.039830640272,162.122295584098,162.204759738569,162.287223131093,
162.369685789079,162.452147739931,162.53460901105,162.617069629836,162.699529623685,
162.781989019994,162.864447846155,162.946906129559,163.029363897595,163.11182117765,
163.195950390887,163.278416387752,163.360880762961,163.443343626157,163.525805086962,
163.608265254977,163.690724239787,163.773182150959,163.85877045577,163.941235190332,
164.023696960577,164.106156204942,164.188613361723,164.271075876341,164.353533544655,
164.435992328928,164.457888589444),.UNSPECIFIED.);
#204=B_SPLINE_CURVE_WITH_KNOTS('',3,(#20783,#20784,#20785,#20786,#20787,
#20788,#20789,#20790,#20791,#20792,#20793,#20794,#20795,#20796,#20797,#20798,
#20799,#20800,#20801,#20802,#20803,#20804,#20805,#20806,#20807,#20808,#20809,
#20810,#20811,#20812,#20813,#20814,#20815,#20816,#20817,#20818,#20819,#20820,
#20821,#20822,#20823,#20824,#20825,#20826,#20827,#20828,#20829,#20830,#20831,
#20832,#20833,#20834,#20835,#20836,#20837,#20838,#20839,#20840,#20841,#20842,
#20843,#20844,#20845,#20846,#20847,#20848,#20849,#20850,#20851,#20852,#20853,
#20854,#20855,#20856,#20857,#20858,#20859,#20860,#20861,#20862,#20863,#20864,
#20865,#20866,#20867),.UNSPECIFIED.,.F.,.F.,(4,3,3,3,3,3,3,3,3,3,3,3,3,
3,3,3,3,3,3,3,3,3,3,3,3,3,3,3,4),(158.174289778564,158.25182298141,158.264170960032,
158.341688329228,158.419118396679,158.496476817949,158.573779197164,158.651041097927,
158.728288308618,158.805529832837,158.882779724183,158.960052038326,159.037405109552,
159.114799639304,159.192308144266,159.263924571402,159.340232490144,159.416451593538,
159.492598491568,159.568689727161,159.644741792255,159.720782406705,159.796820324337,
159.872870430293,159.948947616582,160.025109268506,160.101317979426,160.177636942526,
160.220785774833),.UNSPECIFIED.);
#205=B_SPLINE_CURVE_WITH_KNOTS('',3,(#20869,#20870,#20871,#20872,#20873,
#20874,#20875,#20876,#20877,#20878,#20879,#20880,#20881,#20882,#20883,#20884,
#20885,#20886,#20887,#20888,#20889,#20890,#20891,#20892,#20893,#20894,#20895,
#20896,#20897,#20898,#20899,#20900,#20901,#20902,#20903,#20904,#20905,#20906,
#20907,#20908,#20909,#20910,#20911,#20912,#20913,#20914,#20915,#20916,#20917,
#20918,#20919,#20920,#20921,#20922,#20923,#20924,#20925,#20926,#20927,#20928,
#20929,#20930,#20931,#20932,#20933,#20934,#20935,#20936,#20937,#20938,#20939,
#20940,#20941,#20942,#20943,#20944,#20945,#20946,#20947,#20948,#20949,#20950),
 .UNSPECIFIED.,.F.,.F.,(4,3,3,3,3,3,3,3,3,3,3,3,3,3,3,3,3,3,3,3,3,3,3,3,
3,3,3,4),(158.174223456389,158.255576040659,158.337061991695,158.381010031304,
158.458538184513,158.535985059474,158.613366238182,158.690697255642,158.767993610473,
158.845283910809,158.922573818547,158.999877340545,159.077208488672,159.154627978493,
159.232093336915,159.309678723213,159.379418039355,159.455165032216,159.530819705694,
159.606399033243,159.683142945243,159.758622758066,159.834082616388,159.909537686717,
159.987240847348,160.062760807305,160.141555568273,160.220350329241),
 .UNSPECIFIED.);
#206=B_SPLINE_CURVE_WITH_KNOTS('',3,(#20951,#20952,#20953,#20954,#20955,
#20956,#20957,#20958,#20959,#20960,#20961,#20962,#20963,#20964,#20965,#20966,
#20967,#20968,#20969,#20970,#20971,#20972,#20973,#20974,#20975,#20976,#20977,
#20978,#20979,#20980,#20981,#20982,#20983,#20984,#20985,#20986,#20987,#20988,
#20989,#20990,#20991,#20992,#20993,#20994,#20995,#20996,#20997,#20998,#20999,
#21000,#21001,#21002,#21003,#21004,#21005,#21006,#21007,#21008,#21009,#21010,
#21011,#21012,#21013,#21014,#21015,#21016,#21017,#21018,#21019,#21020,#21021,
#21022,#21023,#21024,#21025,#21026,#21027,#21028,#21029,#21030,#21031,#21032,
#21033,#21034,#21035,#21036,#21037,#21038,#21039,#21040,#21041,#21042,#21043,
#21044,#21045,#21046,#21047,#21048,#21049,#21050,#21051,#21052,#21053,#21054,
#21055,#21056,#21057,#21058,#21059,#21060,#21061,#21062,#21063,#21064,#21065,
#21066,#21067,#21068,#21069,#21070,#21071,#21072,#21073,#21074,#21075,#21076,
#21077,#21078,#21079,#21080,#21081,#21082,#21083,#21084,#21085,#21086,#21087,
#21088,#21089,#21090,#21091,#21092,#21093,#21094,#21095,#21096,#21097,#21098,
#21099,#21100,#21101,#21102,#21103,#21104,#21105,#21106,#21107),
 .UNSPECIFIED.,.F.,.F.,(4,3,3,3,3,3,3,3,3,3,3,3,3,3,3,3,3,3,3,3,3,3,3,3,
3,3,3,3,3,3,3,3,3,3,3,3,3,3,3,3,3,3,3,3,3,3,3,3,3,3,3,3,4),(160.22122533308,
160.303687539116,160.386149396856,160.46861091315,160.551072094847,160.633532948798,
160.715993481853,160.798453700859,160.880913612667,160.963373224125,161.045832542081,
161.128291573383,161.21075032488,161.293208803418,161.375667015846,161.45812496901,
161.540582669758,161.623040124936,161.70549734139,161.791509567892,161.874833912315,
161.957300517761,162.039766279002,162.122231223455,162.204695378531,162.28715877164,
162.369621430188,162.452083381581,162.53454465322,162.617005272504,162.699465266831,
162.781924663595,162.86438349019,162.946841774007,163.029299542434,163.11175682286,
163.195890058271,163.278356056363,163.360820432718,163.443283296981,163.525744758771,
163.608204927692,163.690663913328,163.773121825245,163.85871767077,163.94118240737,
164.023644179372,164.106103425214,164.188560583191,164.271023101472,164.353480772327,
164.435939562278,164.457888589444),.UNSPECIFIED.);
#207=B_SPLINE_CURVE_WITH_KNOTS('',3,(#21113,#21114,#21115,#21116,#21117,
#21118,#21119,#21120,#21121,#21122,#21123,#21124,#21125,#21126,#21127,#21128,
#21129,#21130,#21131,#21132,#21133,#21134,#21135,#21136,#21137,#21138,#21139,
#21140,#21141,#21142,#21143,#21144,#21145,#21146,#21147,#21148,#21149,#21150,
#21151,#21152,#21153,#21154,#21155,#21156,#21157,#21158,#21159,#21160,#21161,
#21162,#21163,#21164,#21165,#21166,#21167,#21168,#21169,#21170,#21171,#21172,
#21173,#21174,#21175,#21176,#21177,#21178,#21179,#21180,#21181,#21182,#21183,
#21184,#21185,#21186,#21187,#21188,#21189,#21190,#21191,#21192,#21193,#21194,
#21195,#21196,#21197,#21198,#21199,#21200,#21201,#21202,#21203,#21204,#21205,
#21206,#21207,#21208,#21209,#21210,#21211,#21212,#21213,#21214,#21215,#21216,
#21217,#21218,#21219,#21220,#21221,#21222,#21223,#21224,#21225,#21226,#21227,
#21228,#21229,#21230,#21231,#21232,#21233,#21234,#21235,#21236,#21237,#21238,
#21239,#21240,#21241,#21242,#21243,#21244,#21245,#21246,#21247,#21248,#21249,
#21250,#21251,#21252,#21253,#21254,#21255,#21256,#21257,#21258,#21259,#21260,
#21261,#21262,#21263,#21264,#21265,#21266,#21267,#21268,#21269),
 .UNSPECIFIED.,.F.,.F.,(4,3,3,3,3,3,3,3,3,3,3,3,3,3,3,3,3,3,3,3,3,3,3,3,
3,3,3,3,3,3,3,3,3,3,3,3,3,3,3,3,3,3,3,3,3,3,3,3,3,3,3,3,4),(166.50441064026,
166.586872846296,166.669334704036,166.75179622033,166.834257402027,166.916718255978,
166.999178789033,167.081639008039,167.164098919847,167.246558531305,167.329017849261,
167.411476880563,167.49393563206,167.576394110598,167.658852323026,167.741310276191,
167.823767976939,167.906225432117,167.988682648571,168.074694875073,168.158019219496,
168.240485824942,168.322951586183,168.405416530636,168.487880685712,168.570344078821,
168.652806737369,168.735268688762,168.817729960401,168.900190579685,168.982650574012,
169.065109970776,169.147568797371,169.230027081188,169.312484849615,169.394942130041,
169.479075365452,169.561541363544,169.644005739899,169.726468604162,169.808930065952,
169.891390234873,169.973849220509,170.056307132426,170.141902977951,170.224367714551,
170.306829486553,170.389288732395,170.471745890372,170.554208408653,170.636666079508,
170.719124869459,170.741073896624),.UNSPECIFIED.);
#208=B_SPLINE_CURVE_WITH_KNOTS('',3,(#21270,#21271,#21272,#21273,#21274,
#21275,#21276,#21277,#21278,#21279,#21280,#21281,#21282,#21283,#21284,#21285,
#21286,#21287,#21288,#21289,#21290,#21291,#21292,#21293,#21294,#21295,#21296,
#21297,#21298,#21299,#21300,#21301,#21302,#21303,#21304,#21305,#21306,#21307,
#21308,#21309,#21310,#21311,#21312,#21313,#21314,#21315,#21316,#21317,#21318,
#21319,#21320,#21321,#21322,#21323,#21324,#21325,#21326,#21327,#21328,#21329,
#21330,#21331,#21332,#21333,#21334,#21335,#21336,#21337,#21338,#21339,#21340,
#21341,#21342,#21343,#21344,#21345),.UNSPECIFIED.,.F.,.F.,(4,3,3,3,3,3,
3,3,3,3,3,3,3,3,3,3,3,3,3,3,3,3,3,3,3,4),(164.457888589444,164.540350193298,
164.622811131269,164.705271430754,164.787731119151,164.870190223853,164.952648772253,
165.035106791739,165.1175643097,165.204242205355,165.28670899119,165.369174104534,
165.451637655039,165.534099752337,165.616560506038,165.699020025736,165.781478421003,
165.8639358014,165.946402187667,166.028865389681,166.111325845961,166.193783994872,
166.276249599751,166.358709478965,166.441173592329,166.50441064017),
 .UNSPECIFIED.);
#209=B_SPLINE_CURVE_WITH_KNOTS('',3,(#21347,#21348,#21349,#21350,#21351,
#21352,#21353,#21354,#21355,#21356,#21357,#21358,#21359,#21360,#21361,#21362,
#21363,#21364,#21365,#21366,#21367,#21368,#21369,#21370,#21371,#21372,#21373,
#21374,#21375,#21376,#21377,#21378,#21379,#21380,#21381,#21382,#21383,#21384,
#21385,#21386,#21387,#21388,#21389,#21390,#21391,#21392,#21393,#21394,#21395,
#21396,#21397,#21398,#21399,#21400,#21401,#21402,#21403,#21404,#21405,#21406,
#21407,#21408,#21409,#21410,#21411,#21412,#21413,#21414,#21415,#21416,#21417,
#21418,#21419,#21420,#21421,#21422),.UNSPECIFIED.,.F.,.F.,(4,3,3,3,3,3,
3,3,3,3,3,3,3,3,3,3,3,3,3,3,3,3,3,3,3,4),(164.457888589444,164.540350193298,
164.622811131268,164.705271430754,164.787731119151,164.870190223853,164.952648772252,
165.035106791738,165.1175643097,165.20424220536,165.286708991196,165.369174104539,
165.451637655044,165.534099752342,165.616560506044,165.699020025741,165.781478421009,
165.863935801406,165.946402187672,166.028865389686,166.111325845966,166.193783994877,
166.276249599756,166.358709478971,166.441173592335,166.50441064026),
 .UNSPECIFIED.);
#210=B_SPLINE_CURVE_WITH_KNOTS('',3,(#21423,#21424,#21425,#21426,#21427,
#21428,#21429,#21430,#21431,#21432,#21433,#21434,#21435,#21436,#21437,#21438,
#21439,#21440,#21441,#21442,#21443,#21444,#21445,#21446,#21447,#21448,#21449,
#21450,#21451,#21452,#21453,#21454,#21455,#21456,#21457,#21458,#21459,#21460,
#21461,#21462,#21463,#21464,#21465,#21466,#21467,#21468,#21469,#21470,#21471,
#21472,#21473,#21474,#21475,#21476,#21477,#21478,#21479,#21480,#21481,#21482,
#21483,#21484,#21485,#21486,#21487,#21488,#21489,#21490,#21491,#21492,#21493,
#21494,#21495,#21496,#21497,#21498,#21499,#21500,#21501,#21502,#21503,#21504,
#21505,#21506,#21507,#21508,#21509,#21510,#21511,#21512,#21513,#21514,#21515,
#21516,#21517,#21518,#21519,#21520,#21521,#21522,#21523,#21524,#21525,#21526,
#21527,#21528,#21529,#21530,#21531,#21532,#21533,#21534,#21535,#21536,#21537,
#21538,#21539,#21540,#21541,#21542,#21543,#21544,#21545,#21546,#21547,#21548,
#21549,#21550,#21551,#21552,#21553,#21554,#21555,#21556,#21557,#21558,#21559,
#21560,#21561,#21562,#21563,#21564,#21565,#21566,#21567,#21568,#21569,#21570,
#21571,#21572,#21573,#21574,#21575,#21576,#21577,#21578,#21579,#21580,#21581,
#21582,#21583,#21584,#21585,#21586,#21587,#21588,#21589,#21590,#21591),
 .UNSPECIFIED.,.F.,.F.,(4,3,3,3,3,3,3,3,3,3,3,3,3,3,3,3,3,3,3,3,3,3,3,3,
3,3,3,3,3,3,3,3,3,3,3,3,3,3,3,3,3,3,3,3,3,3,3,3,3,3,3,3,3,3,3,3,4),(166.50541292827,
166.581074695536,166.656660402689,166.732186932408,166.811498828828,166.886966429492,
166.962429663997,167.037903691478,167.113403679882,167.188983704042,167.264610390849,
167.34033877611,167.366682103763,167.444212300223,167.521655394828,167.599027028884,
167.676342792453,167.753618235231,167.83087911765,167.908134423295,167.985398193589,
168.062684472073,168.140051284865,168.217459619572,168.294981176135,168.365090111813,
168.442620229876,168.520063259192,168.597434841018,168.674750565378,168.752025981939,
168.829286857964,168.90654216931,168.983805957402,169.061092265786,169.138459127392,
169.215867521324,169.293389154196,169.363498119864,169.440334151987,169.517081167714,
169.593755405277,169.670373044799,169.746950221425,169.823819709737,169.900379812259,
169.976950109407,170.053545170429,170.130635409801,170.207362606382,170.284634367149,
170.361906127915,170.439515156729,170.517006394961,170.594430128243,170.671788667788,
170.74144325617),.UNSPECIFIED.);
#211=B_SPLINE_CURVE_WITH_KNOTS('',3,(#21597,#21598,#21599,#21600,#21601,
#21602,#21603,#21604,#21605,#21606,#21607,#21608,#21609,#21610,#21611,#21612,
#21613,#21614,#21615,#21616,#21617,#21618,#21619,#21620,#21621,#21622,#21623,
#21624,#21625,#21626,#21627,#21628,#21629,#21630,#21631,#21632,#21633,#21634,
#21635,#21636,#21637,#21638,#21639,#21640,#21641,#21642,#21643,#21644,#21645,
#21646,#21647,#21648,#21649,#21650,#21651,#21652,#21653,#21654,#21655,#21656,
#21657,#21658,#21659,#21660,#21661,#21662,#21663,#21664,#21665,#21666,#21667,
#21668,#21669,#21670,#21671,#21672,#21673,#21674,#21675,#21676,#21677,#21678,
#21679,#21680,#21681,#21682,#21683,#21684,#21685,#21686,#21687,#21688,#21689,
#21690,#21691,#21692,#21693,#21694,#21695,#21696,#21697,#21698,#21699,#21700,
#21701,#21702,#21703,#21704,#21705,#21706,#21707,#21708,#21709,#21710,#21711,
#21712,#21713,#21714,#21715,#21716,#21717,#21718,#21719,#21720,#21721,#21722,
#21723,#21724,#21725,#21726,#21727,#21728,#21729,#21730,#21731,#21732,#21733,
#21734,#21735,#21736,#21737,#21738,#21739,#21740,#21741,#21742,#21743,#21744,
#21745,#21746,#21747,#21748,#21749,#21750,#21751,#21752,#21753,#21754,#21755,
#21756,#21757,#21758,#21759,#21760,#21761,#21762,#21763,#21764,#21765),
 .UNSPECIFIED.,.F.,.F.,(4,3,3,3,3,3,3,3,3,3,3,3,3,3,3,3,3,3,3,3,3,3,3,3,
3,3,3,3,3,3,3,3,3,3,3,3,3,3,3,3,3,3,3,3,3,3,3,3,3,3,3,3,3,3,3,3,4),(172.78759594744,
172.86986216778,172.952274762003,173.034920623703,173.117686797904,173.200653382848,
173.260475130573,173.337296327728,173.414028289942,173.49068726809,173.567289454552,
173.643850996432,173.720898214621,173.797442389266,173.873996669311,173.950575634291,
174.027988911204,174.104700391511,174.182464566726,174.260228741942,174.337811365556,
174.415301347765,174.49271432499,174.570065878491,174.647371545402,174.724654138447,
174.801925925391,174.879200925247,174.956493156185,175.03385782855,175.111259436983,
175.188767251591,175.259982353312,175.341466326267,175.422845690407,175.507099057554,
175.588252552726,175.669329230685,175.750314658476,175.759859158996,175.8408675549,
175.921951811731,176.006397849968,176.087703931675,176.169087721443,176.250592382472,
176.259735964681,176.337263655425,176.414707268943,176.492069608677,176.569385657828,
176.646669470485,176.723935079898,176.801217331499,176.87850613038,176.95584990749,
177.023722386416),.UNSPECIFIED.);
#212=B_SPLINE_CURVE_WITH_KNOTS('',3,(#21766,#21767,#21768,#21769,#21770,
#21771,#21772,#21773,#21774,#21775,#21776,#21777,#21778,#21779,#21780,#21781,
#21782,#21783,#21784,#21785,#21786,#21787,#21788,#21789,#21790,#21791,#21792,
#21793,#21794,#21795,#21796,#21797,#21798,#21799,#21800,#21801,#21802,#21803,
#21804,#21805,#21806,#21807,#21808,#21809,#21810,#21811,#21812,#21813,#21814,
#21815,#21816,#21817,#21818,#21819,#21820,#21821,#21822,#21823,#21824,#21825,
#21826,#21827,#21828,#21829,#21830,#21831,#21832,#21833,#21834,#21835,#21836,
#21837,#21838,#21839,#21840,#21841),.UNSPECIFIED.,.F.,.F.,(4,3,3,3,3,3,
3,3,3,3,3,3,3,3,3,3,3,3,3,3,3,3,3,3,3,4),(170.741073896624,170.823535500478,
170.905996438448,170.988456737934,171.070916426331,171.153375531033,171.235834079432,
171.318292098918,171.40074961688,171.48742751254,171.569894298376,171.652359411719,
171.734822962225,171.817285059522,171.899745813224,171.982205332921,172.064663728188,
172.147121108585,172.229587494852,172.312050696865,172.394511153146,172.476969302057,
172.559434906936,172.641894786151,172.724358899514,172.78759594744),
 .UNSPECIFIED.);
#213=B_SPLINE_CURVE_WITH_KNOTS('',3,(#21843,#21844,#21845,#21846,#21847,
#21848,#21849,#21850,#21851,#21852,#21853,#21854,#21855,#21856,#21857,#21858,
#21859,#21860,#21861,#21862,#21863,#21864,#21865,#21866,#21867,#21868,#21869,
#21870,#21871,#21872,#21873,#21874,#21875,#21876,#21877,#21878,#21879,#21880,
#21881,#21882,#21883,#21884,#21885,#21886,#21887,#21888,#21889,#21890,#21891,
#21892,#21893,#21894,#21895,#21896,#21897,#21898,#21899,#21900,#21901,#21902,
#21903,#21904,#21905,#21906,#21907,#21908,#21909,#21910,#21911,#21912,#21913,
#21914,#21915,#21916,#21917,#21918,#21919,#21920,#21921,#21922,#21923,#21924,
#21925,#21926,#21927),.UNSPECIFIED.,.F.,.F.,(4,3,3,3,3,3,3,3,3,3,3,3,3,
3,3,3,3,3,3,3,3,3,3,3,3,3,3,3,4),(170.74144325617,170.818802116145,170.896087588298,
170.973375029628,171.050678446185,171.12808736863,171.205498258243,171.283016619449,
171.360314135966,171.441800450399,171.523182532758,171.607266434566,171.688423753419,
171.769504537174,171.850494529207,171.859518139992,171.940531246283,172.021619940555,
172.105895491421,172.187204957811,172.268591859021,172.350098997786,172.358722144017,
172.44182853159,172.528270385522,172.61101135579,172.693618768605,172.776046178395,
172.787595947318),.UNSPECIFIED.);
#214=B_SPLINE_CURVE_WITH_KNOTS('',3,(#21928,#21929,#21930,#21931,#21932,
#21933,#21934,#21935,#21936,#21937,#21938,#21939,#21940,#21941,#21942,#21943,
#21944,#21945,#21946,#21947,#21948,#21949,#21950,#21951,#21952,#21953,#21954,
#21955,#21956,#21957,#21958,#21959,#21960,#21961,#21962,#21963,#21964,#21965,
#21966,#21967,#21968,#21969,#21970,#21971,#21972,#21973,#21974,#21975,#21976,
#21977,#21978,#21979,#21980,#21981,#21982,#21983,#21984,#21985,#21986,#21987,
#21988,#21989,#21990,#21991,#21992,#21993,#21994,#21995,#21996,#21997,#21998,
#21999,#22000,#22001,#22002,#22003,#22004,#22005,#22006,#22007,#22008,#22009,
#22010,#22011,#22012,#22013,#22014,#22015,#22016,#22017,#22018,#22019,#22020,
#22021,#22022,#22023,#22024,#22025,#22026,#22027,#22028,#22029,#22030,#22031,
#22032,#22033,#22034,#22035,#22036,#22037,#22038,#22039,#22040,#22041,#22042,
#22043,#22044,#22045,#22046,#22047,#22048,#22049,#22050,#22051,#22052,#22053,
#22054,#22055,#22056,#22057,#22058,#22059,#22060,#22061,#22062,#22063,#22064,
#22065,#22066,#22067,#22068,#22069,#22070,#22071,#22072,#22073,#22074,#22075,
#22076,#22077,#22078,#22079,#22080,#22081,#22082,#22083,#22084,#22085,#22086,
#22087,#22088,#22089,#22090,#22091,#22092,#22093),.UNSPECIFIED.,.F.,.F.,
(4,3,3,3,3,3,3,3,3,3,3,3,3,3,3,3,3,3,3,3,3,3,3,3,3,3,3,3,3,3,3,3,3,3,3,
3,3,3,3,3,3,3,3,3,3,3,3,3,3,3,3,3,3,3,3,4),(172.78759594744,172.867358168951,
172.947180515715,173.027072473787,173.109586893358,173.189701149854,173.273415650961,
173.357130152068,173.43399353672,173.51076336853,173.587455904518,173.664087339685,
173.740673820468,173.817531862925,173.894090185888,173.97065452056,174.047239433687,
174.124314115295,174.201020936164,174.278279548142,174.355538160119,174.433068356579,
174.510511451184,174.58788308524,174.665198848809,174.742474291587,174.819735174007,
174.896990479651,174.974254249945,175.05154052843,175.128907341222,175.206315675929,
175.283837232491,175.35394616817,175.431476286233,175.508919315549,175.586290897375,
175.663606621735,175.740882038296,175.818142914321,175.895398225668,175.972662013759,
176.049948322143,176.127315183749,176.204723577681,176.282245210553,176.352354176221,
176.42920941739,176.50594720523,176.582616756367,176.659232722429,176.735809718978,
176.812371831209,176.888923699021,176.965501877551,177.023545810813),
 .UNSPECIFIED.);
#215=B_SPLINE_CURVE_WITH_KNOTS('',3,(#22099,#22100,#22101,#22102,#22103,
#22104,#22105,#22106,#22107,#22108,#22109,#22110,#22111,#22112,#22113,#22114,
#22115,#22116,#22117,#22118,#22119,#22120,#22121,#22122,#22123,#22124,#22125,
#22126,#22127,#22128,#22129,#22130,#22131,#22132,#22133,#22134,#22135,#22136,
#22137,#22138,#22139,#22140,#22141,#22142,#22143,#22144,#22145,#22146,#22147,
#22148,#22149,#22150,#22151,#22152,#22153,#22154,#22155,#22156,#22157,#22158,
#22159,#22160,#22161,#22162,#22163,#22164,#22165,#22166,#22167,#22168,#22169,
#22170,#22171,#22172,#22173,#22174,#22175,#22176,#22177,#22178,#22179,#22180,
#22181,#22182,#22183,#22184,#22185,#22186,#22187,#22188,#22189,#22190,#22191,
#22192,#22193,#22194,#22195,#22196,#22197,#22198,#22199,#22200,#22201,#22202,
#22203,#22204,#22205,#22206,#22207,#22208,#22209,#22210,#22211,#22212,#22213,
#22214,#22215,#22216,#22217,#22218,#22219,#22220,#22221,#22222,#22223,#22224,
#22225,#22226,#22227,#22228,#22229,#22230,#22231,#22232,#22233,#22234,#22235,
#22236,#22237,#22238,#22239,#22240,#22241,#22242,#22243,#22244,#22245,#22246,
#22247,#22248,#22249,#22250,#22251,#22252,#22253,#22254,#22255,#22256,#22257,
#22258,#22259,#22260,#22261,#22262,#22263,#22264,#22265,#22266,#22267),
 .UNSPECIFIED.,.F.,.F.,(4,3,3,3,3,3,3,3,3,3,3,3,3,3,3,3,3,3,3,3,3,3,3,3,
3,3,3,3,3,3,3,3,3,3,3,3,3,3,3,3,3,3,3,3,3,3,3,3,3,3,3,3,3,3,3,3,4),(179.070781254619,
179.183730485173,179.258996798789,179.336514167985,179.413944235437,179.491302656706,
179.568605035921,179.645866936684,179.723114147375,179.800355671594,179.87760556294,
179.954877877083,180.032230948309,180.109625478061,180.187133983023,180.258750410158,
180.335571607313,180.412303569527,180.488962547675,180.565564734136,180.642126276017,
180.719173494206,180.79571766885,180.872271948896,180.948850913875,181.026264190788,
181.102975671095,181.180739846312,181.258504021528,181.336086645142,181.413576627351,
181.490989604576,181.568341158077,181.645646824989,181.722929418034,181.800201204978,
181.877476204834,181.954768435773,182.032133108138,182.10953471657,182.187042531178,
182.258257632897,182.339741605852,182.421120969991,182.505374337139,182.58652783231,
182.667604510269,182.748589938059,182.758134438582,182.839142834486,182.920227091318,
183.004673129555,183.085979211262,183.167363001031,183.24886766206,183.258011244266,
183.307783619138),.UNSPECIFIED.);
#216=B_SPLINE_CURVE_WITH_KNOTS('',3,(#22268,#22269,#22270,#22271,#22272,
#22273,#22274,#22275,#22276,#22277,#22278,#22279,#22280,#22281,#22282,#22283,
#22284,#22285,#22286,#22287,#22288,#22289,#22290,#22291,#22292,#22293,#22294,
#22295,#22296,#22297,#22298,#22299,#22300,#22301,#22302,#22303,#22304,#22305,
#22306,#22307,#22308,#22309,#22310,#22311,#22312,#22313,#22314,#22315,#22316,
#22317,#22318,#22319,#22320,#22321,#22322,#22323,#22324,#22325,#22326,#22327,
#22328,#22329,#22330,#22331,#22332,#22333,#22334,#22335,#22336,#22337,#22338,
#22339,#22340,#22341,#22342,#22343,#22344,#22345,#22346,#22347,#22348,#22349),
 .UNSPECIFIED.,.F.,.F.,(4,3,3,3,3,3,3,3,3,3,3,3,3,3,3,3,3,3,3,3,3,3,3,3,
3,3,3,4),(177.023722386416,177.101168095,177.180328835525,177.25948957605,
177.336338199237,177.413093045634,177.489770385039,177.566386424814,177.642957323439,
177.719993056436,177.796535475142,177.873083811704,177.949652643152,178.027050279219,
178.103741360172,178.181492273796,178.25924318742,178.335709385331,178.412087926232,
178.488395345374,178.564643301564,178.640858774118,178.717056604626,178.793251620891,
178.869486590712,178.945742773932,179.022071940622,179.070781254518),
 .UNSPECIFIED.);
#217=B_SPLINE_CURVE_WITH_KNOTS('',3,(#22351,#22352,#22353,#22354,#22355,
#22356,#22357,#22358,#22359,#22360,#22361,#22362,#22363,#22364,#22365,#22366,
#22367,#22368,#22369,#22370,#22371,#22372,#22373,#22374,#22375,#22376,#22377,
#22378,#22379,#22380,#22381,#22382,#22383,#22384,#22385,#22386,#22387,#22388,
#22389,#22390,#22391,#22392,#22393,#22394,#22395,#22396,#22397,#22398,#22399,
#22400,#22401,#22402,#22403,#22404,#22405,#22406,#22407,#22408,#22409,#22410,
#22411,#22412,#22413,#22414,#22415,#22416,#22417,#22418,#22419,#22420,#22421,
#22422,#22423,#22424,#22425,#22426,#22427,#22428,#22429,#22430,#22431,#22432,
#22433,#22434,#22435),.UNSPECIFIED.,.F.,.F.,(4,3,3,3,3,3,3,3,3,3,3,3,3,
3,3,3,3,3,3,3,3,3,3,3,3,3,3,3,4),(177.023545810813,177.100169179658,177.176883966167,
177.253652922408,177.330529681703,177.350762184272,177.428356853706,177.505859119816,
177.583284604887,177.660648876263,177.737967457355,177.815263161827,177.892548206483,
177.969836598416,178.047142343942,178.124520383929,178.201935455673,178.279456069945,
178.349170192323,178.430656506756,178.512038589115,178.596122490923,178.677279809776,
178.758360593529,178.839350585564,178.848374196348,178.922846731534,178.997365107791,
179.070781254619),.UNSPECIFIED.);
#218=B_SPLINE_CURVE_WITH_KNOTS('',3,(#22436,#22437,#22438,#22439,#22440,
#22441,#22442,#22443,#22444,#22445,#22446,#22447,#22448,#22449,#22450,#22451,
#22452,#22453,#22454,#22455,#22456,#22457,#22458,#22459,#22460,#22461,#22462,
#22463,#22464,#22465,#22466,#22467,#22468,#22469,#22470,#22471,#22472,#22473,
#22474,#22475,#22476,#22477,#22478,#22479,#22480,#22481,#22482,#22483,#22484,
#22485,#22486,#22487,#22488,#22489,#22490,#22491,#22492,#22493,#22494,#22495,
#22496,#22497,#22498,#22499,#22500,#22501,#22502,#22503,#22504,#22505,#22506,
#22507,#22508,#22509,#22510,#22511,#22512,#22513,#22514,#22515,#22516,#22517,
#22518,#22519,#22520,#22521,#22522,#22523,#22524,#22525,#22526,#22527,#22528,
#22529,#22530,#22531,#22532,#22533,#22534,#22535,#22536,#22537,#22538,#22539,
#22540,#22541,#22542,#22543,#22544,#22545,#22546,#22547,#22548,#22549,#22550,
#22551,#22552,#22553,#22554,#22555,#22556,#22557,#22558,#22559,#22560,#22561,
#22562,#22563,#22564,#22565,#22566,#22567,#22568,#22569,#22570,#22571,#22572,
#22573,#22574,#22575,#22576,#22577,#22578,#22579,#22580,#22581,#22582,#22583,
#22584,#22585,#22586,#22587,#22588,#22589,#22590,#22591,#22592,#22593,#22594,
#22595,#22596,#22597,#22598,#22599,#22600,#22601),.UNSPECIFIED.,.F.,.F.,
(4,3,3,3,3,3,3,3,3,3,3,3,3,3,3,3,3,3,3,3,3,3,3,3,3,3,3,3,3,3,3,3,3,3,3,
3,3,3,3,3,3,3,3,3,3,3,3,3,3,3,3,3,3,3,3,4),(179.070781254733,179.163109084924,
179.256222027202,179.347578200374,179.425106353583,179.502553228544,179.579934407252,
179.657265424712,179.734561779543,179.811852079879,179.889141987617,179.966445509615,
180.043776657743,180.121196147563,180.198661505985,180.276246892283,180.345986208424,
180.422849593076,180.499619424886,180.576311960874,180.652943396041,180.729529876824,
180.806387919281,180.882946242244,180.959510576916,181.036095490044,181.113170171652,
181.18987699252,181.267135604498,181.344394216475,181.421924412935,181.49936750754,
181.576739141596,181.654054905165,181.731330347943,181.808591230363,181.885846536007,
181.963110306301,182.040396584786,182.117763397578,182.195171732285,182.272693288848,
182.342802224526,182.420334076243,182.497778465331,182.575151034455,182.652467374736,
182.729743036649,182.807002031298,182.884254933068,182.961515782812,183.038798623121,
183.116154358625,183.193551410602,183.271044226858,183.307393789556),
 .UNSPECIFIED.);
#219=B_SPLINE_CURVE_WITH_KNOTS('',3,(#22607,#22608,#22609,#22610,#22611,
#22612,#22613,#22614,#22615,#22616,#22617,#22618,#22619,#22620,#22621,#22622,
#22623,#22624,#22625,#22626,#22627,#22628,#22629,#22630,#22631,#22632,#22633,
#22634,#22635,#22636,#22637,#22638,#22639,#22640,#22641,#22642,#22643,#22644,
#22645,#22646,#22647,#22648,#22649,#22650,#22651,#22652,#22653,#22654,#22655,
#22656,#22657,#22658,#22659,#22660,#22661,#22662,#22663,#22664,#22665,#22666,
#22667,#22668,#22669,#22670,#22671,#22672,#22673,#22674,#22675,#22676,#22677,
#22678,#22679,#22680,#22681,#22682,#22683,#22684,#22685,#22686,#22687,#22688,
#22689,#22690,#22691,#22692,#22693,#22694,#22695,#22696,#22697,#22698,#22699,
#22700,#22701,#22702,#22703,#22704,#22705,#22706,#22707,#22708,#22709,#22710,
#22711,#22712,#22713,#22714,#22715,#22716,#22717,#22718,#22719,#22720,#22721,
#22722,#22723,#22724,#22725,#22726,#22727,#22728,#22729,#22730,#22731,#22732,
#22733,#22734,#22735,#22736,#22737,#22738,#22739,#22740,#22741,#22742,#22743,
#22744,#22745,#22746,#22747,#22748,#22749,#22750,#22751,#22752,#22753,#22754,
#22755,#22756,#22757,#22758,#22759,#22760,#22761,#22762,#22763,#22764,#22765,
#22766,#22767,#22768,#22769,#22770,#22771,#22772),.UNSPECIFIED.,.F.,.F.,
(4,3,3,3,3,3,3,3,3,3,3,3,3,3,3,3,3,3,3,3,3,3,3,3,3,3,3,3,3,3,3,3,3,3,3,
3,3,3,3,3,3,3,3,3,3,3,3,3,3,3,3,3,3,3,3,4),(185.353966561943,185.430445028092,
185.506843351555,185.583177999209,185.659465382457,185.735729770735,185.811983844163,
185.888242397231,185.964520225521,186.040874639006,186.117269092864,186.193773470763,
186.257272078375,186.334789447571,186.412219515022,186.489577936292,186.566880315507,
186.64414221627,186.721389426961,186.798630951179,186.875880842525,186.953153156669,
187.030506227895,187.107900757646,187.185409262608,187.257025689744,187.333846886899,
187.410578849113,187.487237827261,187.563840013722,187.640401555603,187.717448773792,
187.793992948436,187.870547228482,187.947126193461,188.024539470374,188.101250950681,
188.179015125897,188.256779301113,188.334361924727,188.411851906936,188.489264884161,
188.566616437662,188.643922104574,188.721204697618,188.798476484562,188.875751484419,
188.953043715357,189.030408387722,189.107809996154,189.185317810762,189.256532912483,
189.340169471562,189.421534418449,189.506306783624,189.591079148798),
 .UNSPECIFIED.);
#220=B_SPLINE_CURVE_WITH_KNOTS('',3,(#22773,#22774,#22775,#22776,#22777,
#22778,#22779,#22780,#22781,#22782,#22783,#22784,#22785,#22786,#22787,#22788,
#22789,#22790,#22791,#22792,#22793,#22794,#22795,#22796,#22797,#22798,#22799,
#22800,#22801,#22802,#22803,#22804,#22805,#22806,#22807,#22808,#22809,#22810,
#22811,#22812,#22813,#22814,#22815,#22816,#22817,#22818,#22819,#22820,#22821,
#22822,#22823,#22824,#22825,#22826,#22827,#22828,#22829,#22830,#22831,#22832,
#22833,#22834,#22835,#22836,#22837,#22838,#22839,#22840,#22841,#22842,#22843,
#22844,#22845,#22846,#22847,#22848,#22849,#22850,#22851,#22852,#22853,#22854),
 .UNSPECIFIED.,.F.,.F.,(4,3,3,3,3,3,3,3,3,3,3,3,3,3,3,3,3,3,3,3,3,3,3,3,
3,3,3,4),(183.307783619138,183.385245296581,183.462635514118,183.539969836095,
183.617263786572,183.697326420205,183.774601632708,183.851885846054,183.929193081493,
184.006537370534,184.083973232362,184.161463460977,184.239059834349,184.257764855636,
184.334613478824,184.41136832522,184.488045664625,184.5646617044,184.641232603025,
184.718268336023,184.794810754728,184.871359091291,184.947927922739,185.025325558805,
185.102016639758,185.179767553382,185.257518467005,185.353966561799),
 .UNSPECIFIED.);
#221=B_SPLINE_CURVE_WITH_KNOTS('',3,(#22856,#22857,#22858,#22859,#22860,
#22861,#22862,#22863,#22864,#22865,#22866,#22867,#22868,#22869,#22870,#22871,
#22872,#22873,#22874,#22875,#22876,#22877,#22878,#22879,#22880,#22881,#22882,
#22883,#22884,#22885,#22886,#22887,#22888,#22889,#22890,#22891,#22892,#22893,
#22894,#22895,#22896,#22897,#22898,#22899,#22900,#22901,#22902,#22903,#22904,
#22905,#22906,#22907,#22908,#22909,#22910,#22911,#22912,#22913,#22914,#22915,
#22916,#22917,#22918,#22919,#22920,#22921,#22922,#22923,#22924,#22925,#22926,
#22927,#22928,#22929,#22930,#22931,#22932,#22933,#22934,#22935,#22936,#22937,
#22938,#22939,#22940),.UNSPECIFIED.,.F.,.F.,(4,3,3,3,3,3,3,3,3,3,3,3,3,
3,3,3,3,3,3,3,3,3,3,3,3,3,3,3,4),(183.307393789556,183.341210232577,183.4180462647,
183.494793280427,183.57146751799,183.648085157511,183.724662334139,183.80153182245,
183.878091924972,183.95466222212,184.031257283142,184.108347522514,184.185074719095,
184.262346479862,184.339618240628,184.417212910062,184.494715176172,184.572140661243,
184.64950493262,184.726823513711,184.804119218182,184.881404262838,184.958692654771,
185.035998400297,185.113376440285,185.190791512029,185.2683121263,185.338026248679,
185.353966561707),.UNSPECIFIED.);
#222=B_SPLINE_CURVE_WITH_KNOTS('',3,(#22941,#22942,#22943,#22944,#22945,
#22946,#22947,#22948,#22949,#22950,#22951,#22952,#22953,#22954,#22955,#22956,
#22957,#22958,#22959,#22960,#22961,#22962,#22963,#22964,#22965,#22966,#22967,
#22968,#22969,#22970,#22971,#22972,#22973,#22974,#22975,#22976,#22977,#22978,
#22979,#22980,#22981,#22982,#22983,#22984,#22985,#22986,#22987,#22988,#22989,
#22990,#22991,#22992,#22993,#22994,#22995,#22996,#22997,#22998,#22999,#23000,
#23001,#23002,#23003,#23004,#23005,#23006,#23007,#23008,#23009,#23010,#23011,
#23012,#23013,#23014,#23015,#23016,#23017,#23018,#23019,#23020,#23021,#23022,
#23023,#23024,#23025,#23026,#23027,#23028,#23029,#23030,#23031,#23032,#23033,
#23034,#23035,#23036,#23037,#23038,#23039,#23040,#23041,#23042,#23043,#23044,
#23045,#23046,#23047,#23048,#23049,#23050,#23051,#23052,#23053,#23054,#23055,
#23056,#23057,#23058,#23059,#23060,#23061,#23062,#23063,#23064,#23065,#23066,
#23067,#23068,#23069,#23070,#23071,#23072,#23073,#23074,#23075,#23076,#23077,
#23078,#23079,#23080,#23081,#23082,#23083,#23084,#23085,#23086,#23087,#23088,
#23089,#23090,#23091,#23092,#23093,#23094,#23095,#23096,#23097,#23098,#23099,
#23100,#23101,#23102,#23103,#23104,#23105,#23106,#23107,#23108,#23109),
 .UNSPECIFIED.,.F.,.F.,(4,3,3,3,3,3,3,3,3,3,3,3,3,3,3,3,3,3,3,3,3,3,3,3,
3,3,3,3,3,3,3,3,3,3,3,3,3,3,3,3,3,3,3,3,3,3,3,3,3,3,3,3,3,3,3,3,4),(185.353966561799,
185.434768406434,185.515467769198,185.596036962336,185.676529401149,185.756926595685,
185.837230252705,185.918243358995,185.999332053268,186.083607604134,186.164917070524,
186.246303971735,186.327811110499,186.33643425673,186.413962409939,186.491409284901,
186.568790463608,186.646121481069,186.723417835899,186.800708136235,186.877998043973,
186.955301565971,187.032632714098,187.110052203919,187.187517562341,187.265102948639,
187.334842264781,187.411705649433,187.488475481243,187.565168017232,187.641799452398,
187.718385933182,187.795243975638,187.871802298601,187.948366633274,188.024951546401,
188.102026228009,188.178733048878,188.255991660855,188.333250272832,188.410780469292,
188.488223563897,188.565595197953,188.642910961522,188.7201864043,188.79744728672,
188.874702592364,188.951966362658,189.029252641143,189.106619453935,189.184027788642,
189.261549345205,189.331658280883,189.409186417329,189.486637831798,189.564009604359,
189.59121340711),.UNSPECIFIED.);
#223=B_SPLINE_CURVE_WITH_KNOTS('',3,(#23115,#23116,#23117,#23118,#23119,
#23120,#23121,#23122,#23123,#23124,#23125,#23126,#23127,#23128,#23129,#23130,
#23131,#23132,#23133,#23134,#23135,#23136,#23137,#23138,#23139,#23140,#23141,
#23142,#23143,#23144,#23145,#23146,#23147,#23148,#23149,#23150,#23151,#23152,
#23153,#23154,#23155,#23156,#23157,#23158,#23159,#23160,#23161,#23162,#23163,
#23164,#23165,#23166,#23167,#23168,#23169,#23170,#23171,#23172,#23173,#23174,
#23175,#23176,#23177,#23178,#23179,#23180,#23181,#23182,#23183,#23184,#23185,
#23186,#23187,#23188,#23189,#23190,#23191,#23192,#23193,#23194,#23195,#23196,
#23197,#23198,#23199,#23200,#23201,#23202,#23203,#23204,#23205,#23206,#23207,
#23208,#23209,#23210,#23211,#23212,#23213,#23214,#23215,#23216,#23217,#23218,
#23219,#23220,#23221,#23222,#23223,#23224,#23225,#23226,#23227,#23228,#23229,
#23230,#23231,#23232,#23233,#23234,#23235,#23236,#23237,#23238,#23239,#23240,
#23241,#23242,#23243,#23244,#23245,#23246,#23247,#23248,#23249,#23250,#23251,
#23252,#23253,#23254,#23255,#23256,#23257,#23258,#23259,#23260,#23261,#23262,
#23263,#23264,#23265,#23266,#23267,#23268,#23269,#23270,#23271),
 .UNSPECIFIED.,.F.,.F.,(4,3,3,3,3,3,3,3,3,3,3,3,3,3,3,3,3,3,3,3,3,3,3,3,
3,3,3,3,3,3,3,3,3,3,3,3,3,3,3,3,3,3,3,3,3,3,3,3,3,3,3,3,4),(191.637151868978,
191.719614075014,191.802075932754,191.884537449048,191.966998630745,192.049459484696,
192.131920017751,192.214380236757,192.296840148565,192.379299760023,192.461759077979,
192.544218109281,192.626676860778,192.709135339316,192.791593551744,192.874051504908,
192.956509205656,193.038966660834,193.121423877288,193.20743610379,193.290760448213,
193.373227053659,193.4556928149,193.538157759353,193.620621914429,193.703085307538,
193.785547966086,193.868009917479,193.950471189118,194.032931808402,194.115391802729,
194.197851199493,194.280310026088,194.362768309905,194.445226078333,194.527683358758,
194.611816594169,194.694282592261,194.776746968617,194.859209832879,194.941671294669,
195.024131463591,195.106590449226,195.189048361143,195.274644206668,195.357108943268,
195.43957071527,195.522029961112,195.604487119089,195.686949637371,195.769407308226,
195.851866098176,195.873815125342),.UNSPECIFIED.);
#224=B_SPLINE_CURVE_WITH_KNOTS('',3,(#23272,#23273,#23274,#23275,#23276,
#23277,#23278,#23279,#23280,#23281,#23282,#23283,#23284,#23285,#23286,#23287,
#23288,#23289,#23290,#23291,#23292,#23293,#23294,#23295,#23296,#23297,#23298,
#23299,#23300,#23301,#23302,#23303,#23304,#23305,#23306,#23307,#23308,#23309,
#23310,#23311,#23312,#23313,#23314,#23315,#23316,#23317,#23318,#23319,#23320,
#23321,#23322,#23323,#23324,#23325,#23326,#23327,#23328,#23329,#23330,#23331,
#23332,#23333,#23334,#23335,#23336,#23337,#23338,#23339,#23340,#23341,#23342,
#23343,#23344,#23345,#23346,#23347,#23348,#23349,#23350,#23351,#23352,#23353),
 .UNSPECIFIED.,.F.,.F.,(4,3,3,3,3,3,3,3,3,3,3,3,3,3,3,3,3,3,3,3,3,3,3,3,
3,3,3,4),(189.591079148798,189.673744433483,189.756409718167,189.837418114071,
189.918502370903,190.00294840914,190.084254490847,190.165638280615,190.247142941643,
190.256286523852,190.333802302115,190.411236602526,190.488605020953,190.565923106103,
190.643206370148,190.72048345446,190.797760034947,190.875050130344,190.952367764349,
191.029773970673,191.107225979987,191.184798788309,191.256040135221,191.342802993755,
191.42913778928,191.51519425617,191.600806779982,191.637151868978),
 .UNSPECIFIED.);
#225=B_SPLINE_CURVE_WITH_KNOTS('',3,(#23355,#23356,#23357,#23358,#23359,
#23360,#23361,#23362,#23363,#23364,#23365,#23366,#23367,#23368,#23369,#23370,
#23371,#23372,#23373,#23374,#23375,#23376,#23377,#23378,#23379,#23380,#23381,
#23382,#23383,#23384,#23385,#23386,#23387,#23388,#23389,#23390,#23391,#23392,
#23393,#23394,#23395,#23396,#23397,#23398,#23399,#23400,#23401,#23402,#23403,
#23404,#23405,#23406,#23407,#23408,#23409,#23410,#23411,#23412,#23413,#23414,
#23415,#23416,#23417,#23418,#23419,#23420,#23421,#23422,#23423,#23424,#23425,
#23426,#23427,#23428,#23429,#23430,#23431,#23432,#23433,#23434,#23435,#23436),
 .UNSPECIFIED.,.F.,.F.,(4,3,3,3,3,3,3,3,3,3,3,3,3,3,3,3,3,3,3,3,3,3,3,3,
3,3,3,4),(189.59121340711,189.668513177153,189.745778103156,189.823035420156,
189.900292112866,189.977562222576,190.054859795428,190.132239819409,190.209665821967,
190.287197824615,190.330066288934,190.406902321057,190.483649336784,190.560323574347,
190.636941213869,190.713518390495,190.790387878807,190.866947981329,190.943518278477,
191.020113339499,191.097203578871,191.173930775452,191.251202536219,191.328474296985,
191.425080755061,191.52096575684,191.615472617705,191.637151868978),
 .UNSPECIFIED.);
#226=B_SPLINE_CURVE_WITH_KNOTS('',3,(#23437,#23438,#23439,#23440,#23441,
#23442,#23443,#23444,#23445,#23446,#23447,#23448,#23449,#23450,#23451,#23452,
#23453,#23454,#23455,#23456,#23457,#23458,#23459,#23460,#23461,#23462,#23463,
#23464,#23465,#23466,#23467,#23468,#23469,#23470,#23471,#23472,#23473,#23474,
#23475,#23476,#23477,#23478,#23479,#23480,#23481,#23482,#23483,#23484,#23485,
#23486,#23487,#23488,#23489,#23490,#23491,#23492,#23493,#23494,#23495,#23496,
#23497,#23498,#23499,#23500,#23501,#23502,#23503,#23504,#23505,#23506,#23507,
#23508,#23509,#23510,#23511,#23512,#23513,#23514,#23515,#23516,#23517,#23518,
#23519,#23520,#23521,#23522,#23523,#23524,#23525,#23526,#23527,#23528,#23529,
#23530,#23531,#23532,#23533,#23534,#23535,#23536,#23537,#23538,#23539,#23540,
#23541,#23542,#23543,#23544,#23545,#23546,#23547,#23548,#23549,#23550,#23551,
#23552,#23553,#23554,#23555,#23556,#23557,#23558,#23559,#23560,#23561,#23562,
#23563,#23564,#23565,#23566,#23567,#23568,#23569,#23570,#23571,#23572,#23573,
#23574,#23575,#23576,#23577,#23578,#23579,#23580,#23581,#23582,#23583,#23584,
#23585,#23586,#23587,#23588,#23589,#23590,#23591,#23592,#23593),
 .UNSPECIFIED.,.F.,.F.,(4,3,3,3,3,3,3,3,3,3,3,3,3,3,3,3,3,3,3,3,3,3,3,3,
3,3,3,3,3,3,3,3,3,3,3,3,3,3,3,3,3,3,3,3,3,3,3,3,3,3,3,3,4),(191.637151868978,
191.719614075014,191.802075932754,191.884537449048,191.966998630745,192.049459484696,
192.131920017751,192.214380236757,192.296840148565,192.379299760023,192.461759077979,
192.544218109281,192.626676860778,192.709135339316,192.791593551744,192.874051504908,
192.956509205656,193.038966660834,193.121423877288,193.20743610379,193.290760448214,
193.373227053659,193.4556928149,193.538157759353,193.620621914429,193.703085307538,
193.785547966086,193.868009917479,193.950471189118,194.032931808402,194.115391802729,
194.197851199493,194.280310026089,194.362768309905,194.445226078333,194.527683358758,
194.61181659417,194.694282592261,194.776746968617,194.859209832879,194.94167129467,
195.024131463591,195.106590449226,195.189048361143,195.274644206668,195.357108943268,
195.43957071527,195.522029961112,195.604487119089,195.686949637371,195.769407308226,
195.851866098176,195.873815125342),.UNSPECIFIED.);
#227=B_SPLINE_CURVE_WITH_KNOTS('',3,(#23599,#23600,#23601,#23602,#23603,
#23604,#23605,#23606,#23607,#23608,#23609,#23610,#23611,#23612,#23613,#23614,
#23615,#23616,#23617,#23618,#23619,#23620,#23621,#23622,#23623,#23624,#23625,
#23626,#23627,#23628,#23629,#23630,#23631,#23632,#23633,#23634,#23635,#23636,
#23637,#23638,#23639,#23640,#23641,#23642,#23643,#23644,#23645,#23646,#23647,
#23648,#23649,#23650,#23651,#23652,#23653,#23654,#23655,#23656,#23657,#23658,
#23659,#23660,#23661,#23662,#23663,#23664,#23665,#23666,#23667,#23668,#23669,
#23670,#23671,#23672,#23673,#23674,#23675,#23676,#23677,#23678,#23679,#23680,
#23681,#23682,#23683,#23684,#23685,#23686,#23687,#23688,#23689,#23690,#23691,
#23692,#23693,#23694,#23695,#23696,#23697,#23698,#23699,#23700,#23701,#23702,
#23703,#23704,#23705,#23706,#23707,#23708,#23709,#23710,#23711,#23712,#23713,
#23714,#23715,#23716,#23717,#23718,#23719,#23720,#23721,#23722,#23723,#23724,
#23725,#23726,#23727,#23728,#23729,#23730,#23731,#23732,#23733,#23734,#23735,
#23736,#23737,#23738,#23739,#23740,#23741,#23742,#23743,#23744,#23745,#23746,
#23747,#23748,#23749,#23750,#23751,#23752,#23753,#23754,#23755,#23756,#23757,
#23758,#23759,#23760,#23761,#23762,#23763,#23764),.UNSPECIFIED.,.F.,.F.,
(4,3,3,3,3,3,3,3,3,3,3,3,3,3,3,3,3,3,3,3,3,3,3,3,3,3,3,3,3,3,3,3,3,3,3,
3,3,3,3,3,3,3,3,3,3,3,3,3,3,3,3,3,3,3,3,4),(197.920337176158,198.012592287876,
198.105554173127,198.199343179307,198.254315414807,198.331164037994,198.407918884391,
198.484596223796,198.561212263571,198.637783162196,198.714818895193,198.791361313899,
198.867909650462,198.944478481909,199.021876117976,199.098567198929,199.176318112552,
199.254069026176,199.331586577794,199.409016797214,199.486375340109,199.563677810696,
199.640939772647,199.718186998429,199.795428509637,199.872678359869,199.949950604782,
200.027303562753,200.104697955062,200.182206282731,200.253822637546,200.331340006742,
200.408770074193,200.486128495463,200.563430874678,200.640692775441,200.717939986132,
200.79518151035,200.872431401696,200.94970371584,201.027056787066,201.104451316817,
201.181959821779,201.253576248915,201.330402679678,201.407138747595,201.483800708564,
201.560404758837,201.636968776588,201.713512055413,201.790049175251,201.866594709989,
201.943198542006,202.019832748578,202.096558624748,202.15629239339),
 .UNSPECIFIED.);
#228=B_SPLINE_CURVE_WITH_KNOTS('',3,(#23765,#23766,#23767,#23768,#23769,
#23770,#23771,#23772,#23773,#23774,#23775,#23776,#23777,#23778,#23779,#23780,
#23781,#23782,#23783,#23784,#23785,#23786,#23787,#23788,#23789,#23790,#23791,
#23792,#23793,#23794,#23795,#23796,#23797,#23798,#23799,#23800,#23801,#23802,
#23803,#23804,#23805,#23806,#23807,#23808,#23809,#23810,#23811,#23812,#23813,
#23814,#23815,#23816,#23817,#23818,#23819,#23820,#23821,#23822,#23823,#23824,
#23825,#23826,#23827,#23828,#23829,#23830,#23831,#23832,#23833,#23834,#23835,
#23836,#23837,#23838,#23839,#23840),.UNSPECIFIED.,.F.,.F.,(4,3,3,3,3,3,
3,3,3,3,3,3,3,3,3,3,3,3,3,3,3,3,3,3,3,4),(195.873815125342,195.956276729196,
196.038737667166,196.121197966652,196.203657655049,196.286116759751,196.36857530815,
196.451033327636,196.533490845598,196.620168741258,196.702635527094,196.785100640437,
196.867564190943,196.95002628824,197.032487041942,197.114946561639,197.197404956906,
197.279862337303,197.36232872357,197.444791925584,197.527252381864,197.609710530775,
197.692176135654,197.774636014869,197.857100128233,197.920337176158),
 .UNSPECIFIED.);
#229=B_SPLINE_CURVE_WITH_KNOTS('',3,(#23842,#23843,#23844,#23845,#23846,
#23847,#23848,#23849,#23850,#23851,#23852,#23853,#23854,#23855,#23856,#23857,
#23858,#23859,#23860,#23861,#23862,#23863,#23864,#23865,#23866,#23867,#23868,
#23869,#23870,#23871,#23872,#23873,#23874,#23875,#23876,#23877,#23878,#23879,
#23880,#23881,#23882,#23883,#23884,#23885,#23886,#23887,#23888,#23889,#23890,
#23891,#23892,#23893,#23894,#23895,#23896,#23897,#23898,#23899,#23900,#23901,
#23902,#23903,#23904,#23905,#23906,#23907,#23908,#23909,#23910,#23911,#23912,
#23913,#23914,#23915,#23916,#23917),.UNSPECIFIED.,.F.,.F.,(4,3,3,3,3,3,
3,3,3,3,3,3,3,3,3,3,3,3,3,3,3,3,3,3,3,4),(195.873815125342,195.956276729196,
196.038737667166,196.121197966652,196.203657655049,196.286116759751,196.36857530815,
196.451033327637,196.533490845598,196.620168741258,196.702635527094,196.785100640437,
196.867564190943,196.95002628824,197.032487041942,197.114946561639,197.197404956906,
197.279862337304,197.36232872357,197.444791925584,197.527252381865,197.609710530775,
197.692176135654,197.774636014869,197.857100128233,197.920337176158),
 .UNSPECIFIED.);
#230=B_SPLINE_CURVE_WITH_KNOTS('',3,(#23918,#23919,#23920,#23921,#23922,
#23923,#23924,#23925,#23926,#23927,#23928,#23929,#23930,#23931,#23932,#23933,
#23934,#23935,#23936,#23937,#23938,#23939,#23940,#23941,#23942,#23943,#23944,
#23945,#23946,#23947,#23948,#23949,#23950,#23951,#23952,#23953,#23954,#23955,
#23956,#23957,#23958,#23959,#23960,#23961,#23962,#23963,#23964,#23965,#23966,
#23967,#23968,#23969,#23970,#23971,#23972,#23973,#23974,#23975,#23976,#23977,
#23978,#23979,#23980,#23981,#23982,#23983,#23984,#23985,#23986,#23987,#23988,
#23989,#23990,#23991,#23992,#23993,#23994,#23995,#23996,#23997,#23998,#23999,
#24000,#24001,#24002,#24003,#24004,#24005,#24006,#24007,#24008,#24009,#24010,
#24011,#24012,#24013,#24014,#24015,#24016,#24017,#24018,#24019,#24020,#24021,
#24022,#24023,#24024,#24025,#24026,#24027,#24028,#24029,#24030,#24031,#24032,
#24033,#24034,#24035,#24036,#24037,#24038,#24039,#24040,#24041,#24042,#24043,
#24044,#24045,#24046,#24047,#24048,#24049,#24050,#24051,#24052,#24053,#24054,
#24055,#24056,#24057,#24058,#24059,#24060,#24061,#24062,#24063,#24064,#24065,
#24066,#24067,#24068,#24069,#24070,#24071,#24072,#24073,#24074,#24075,#24076,
#24077,#24078,#24079,#24080,#24081,#24082,#24083,#24084,#24085,#24086),
 .UNSPECIFIED.,.F.,.F.,(4,3,3,3,3,3,3,3,3,3,3,3,3,3,3,3,3,3,3,3,3,3,3,3,
3,3,3,3,3,3,3,3,3,3,3,3,3,3,3,3,3,3,3,3,3,3,3,3,3,3,3,3,3,3,3,3,4),(197.920337176158,
198.004940290032,198.089996506174,198.175284949322,198.260912878968,198.317330353341,
198.394925022775,198.472427288885,198.549852773956,198.627217045333,198.704535626423,
198.781831330895,198.859116375551,198.936404767484,199.013710513009,199.091088552997,
199.168503624741,199.246024239012,199.315738361392,199.397224675825,199.478606758184,
199.562690659992,199.643847978845,199.7249287626,199.805918754634,199.814942365417,
199.895955471707,199.97704416598,200.061319716846,200.142629183236,200.224016084447,
200.305523223211,200.314146369443,200.391674522652,200.469121397614,200.546502576321,
200.623833593782,200.701129948612,200.778420248948,200.855710156687,200.933013678685,
201.010344826812,201.087764316633,201.165229675055,201.242815061353,201.312554377494,
201.389426875665,201.466204023589,201.542902086867,201.619583820612,201.696169755043,
201.77272997862,201.849279064318,201.926048287445,202.002641694228,202.079498825528,
202.156355956828),.UNSPECIFIED.);
#231=B_SPLINE_CURVE_WITH_KNOTS('',3,(#24092,#24093,#24094,#24095,#24096,
#24097,#24098,#24099,#24100,#24101,#24102,#24103,#24104,#24105,#24106,#24107,
#24108,#24109,#24110,#24111,#24112,#24113,#24114,#24115,#24116,#24117,#24118,
#24119,#24120,#24121,#24122,#24123,#24124,#24125,#24126,#24127,#24128,#24129,
#24130,#24131,#24132,#24133,#24134,#24135,#24136,#24137,#24138,#24139,#24140,
#24141,#24142,#24143,#24144,#24145,#24146,#24147,#24148,#24149,#24150,#24151,
#24152,#24153,#24154,#24155,#24156,#24157,#24158,#24159,#24160,#24161,#24162,
#24163,#24164,#24165,#24166,#24167,#24168,#24169,#24170,#24171,#24172,#24173,
#24174,#24175,#24176,#24177,#24178,#24179,#24180,#24181,#24182,#24183,#24184,
#24185,#24186,#24187,#24188,#24189,#24190,#24191,#24192,#24193,#24194,#24195,
#24196,#24197,#24198,#24199,#24200,#24201,#24202,#24203,#24204,#24205,#24206,
#24207,#24208,#24209,#24210,#24211,#24212,#24213,#24214,#24215,#24216,#24217,
#24218,#24219,#24220,#24221,#24222,#24223,#24224,#24225,#24226,#24227,#24228,
#24229,#24230,#24231,#24232,#24233,#24234,#24235,#24236,#24237,#24238,#24239,
#24240,#24241,#24242,#24243,#24244,#24245,#24246,#24247,#24248,#24249,#24250,
#24251,#24252,#24253,#24254,#24255,#24256,#24257,#24258,#24259,#24260),
 .UNSPECIFIED.,.F.,.F.,(4,3,3,3,3,3,3,3,3,3,3,3,3,3,3,3,3,3,3,3,3,3,3,3,
3,3,3,3,3,3,3,3,3,3,3,3,3,3,3,3,3,3,3,3,3,3,3,3,3,3,3,3,3,3,3,3,4),(204.203522483338,
204.252837083023,204.330352861286,204.407787161697,204.485155580124,204.562473665274,
204.639756929319,204.71703401363,204.794310594118,204.871600689515,204.94891832352,
205.026324529844,205.103776539158,205.18134934748,205.252590694393,205.32943931758,
205.406194163977,205.482871503382,205.559487543157,205.636058441782,205.713094174779,
205.789636593485,205.866184930047,205.942753761495,206.020151397562,206.096842478515,
206.174593392138,206.252344305762,206.32986185738,206.4072920768,206.484650619695,
206.561953090282,206.639215052232,206.716462278015,206.793703789222,206.870953639455,
206.948225884368,207.025578842339,207.102973234648,207.180481562316,207.252097917131,
207.329615286327,207.407045353779,207.484403775048,207.561706154263,207.638968055026,
207.716215265717,207.793456789936,207.870706681282,207.947978995425,208.025332066651,
208.102726596403,208.180235101365,208.251851528501,208.328686636382,208.405419630659,
208.44084770076),.UNSPECIFIED.);
#232=B_SPLINE_CURVE_WITH_KNOTS('',3,(#24261,#24262,#24263,#24264,#24265,
#24266,#24267,#24268,#24269,#24270,#24271,#24272,#24273,#24274,#24275,#24276,
#24277,#24278,#24279,#24280,#24281,#24282,#24283,#24284,#24285,#24286,#24287,
#24288,#24289,#24290,#24291,#24292,#24293,#24294,#24295,#24296,#24297,#24298,
#24299,#24300,#24301,#24302,#24303,#24304,#24305,#24306,#24307,#24308,#24309,
#24310,#24311,#24312,#24313,#24314,#24315,#24316,#24317,#24318,#24319,#24320,
#24321,#24322,#24323,#24324,#24325,#24326,#24327,#24328,#24329,#24330,#24331,
#24332,#24333,#24334,#24335,#24336,#24337,#24338,#24339,#24340,#24341,#24342,
#24343,#24344,#24345),.UNSPECIFIED.,.F.,.F.,(4,3,3,3,3,3,3,3,3,3,3,3,3,
3,3,3,3,3,3,3,3,3,3,3,3,3,3,3,4),(202.15629239339,202.233154548504,202.253329860284,
202.330912483898,202.408402466107,202.485815443332,202.563166996833,202.640472663745,
202.717755256789,202.795027043733,202.87230204359,202.949594274528,203.026958946893,
203.104360555325,203.181868369934,203.253083471654,203.334567444609,203.415946808749,
203.500200175897,203.581353671069,203.662430349028,203.743415776818,203.752960277339,
203.832117663368,203.911324253774,203.990640924028,204.070016779426,204.149517729411,
204.203522483196),.UNSPECIFIED.);
#233=B_SPLINE_CURVE_WITH_KNOTS('',3,(#24347,#24348,#24349,#24350,#24351,
#24352,#24353,#24354,#24355,#24356,#24357,#24358,#24359,#24360,#24361,#24362,
#24363,#24364,#24365,#24366,#24367,#24368,#24369,#24370,#24371,#24372,#24373,
#24374,#24375,#24376,#24377,#24378,#24379,#24380,#24381,#24382,#24383,#24384,
#24385,#24386,#24387,#24388,#24389,#24390,#24391,#24392,#24393,#24394,#24395,
#24396,#24397,#24398,#24399,#24400,#24401,#24402,#24403,#24404,#24405,#24406,
#24407,#24408,#24409,#24410,#24411,#24412,#24413,#24414,#24415,#24416,#24417,
#24418,#24419,#24420,#24421,#24422,#24423,#24424,#24425,#24426,#24427,#24428),
 .UNSPECIFIED.,.F.,.F.,(4,3,3,3,3,3,3,3,3,3,3,3,3,3,3,3,3,3,3,3,3,3,3,3,
3,3,3,4),(202.156355956828,202.233659171187,202.310962385545,202.388492582005,
202.46593567661,202.543307310666,202.620623074235,202.697898517013,202.775159399432,
202.852414705077,202.929678475371,203.006964753856,203.084331566648,203.161739901355,
203.239261457917,203.309370393596,203.385852975525,203.462249014357,203.538575024898,
203.614847459918,203.691087020697,203.767310391095,203.843532386166,203.919767818159,
203.996069078579,204.072405451451,204.148839305911,204.203522483193),
 .UNSPECIFIED.);
#234=B_SPLINE_CURVE_WITH_KNOTS('',3,(#24429,#24430,#24431,#24432,#24433,
#24434,#24435,#24436,#24437,#24438,#24439,#24440,#24441,#24442,#24443,#24444,
#24445,#24446,#24447,#24448,#24449,#24450,#24451,#24452,#24453,#24454,#24455,
#24456,#24457,#24458,#24459,#24460,#24461,#24462,#24463,#24464,#24465,#24466,
#24467,#24468,#24469,#24470,#24471,#24472,#24473,#24474,#24475,#24476,#24477,
#24478,#24479,#24480,#24481,#24482,#24483,#24484,#24485,#24486,#24487,#24488,
#24489,#24490,#24491,#24492,#24493,#24494,#24495,#24496,#24497,#24498,#24499,
#24500,#24501,#24502,#24503,#24504,#24505,#24506,#24507,#24508,#24509,#24510,
#24511,#24512,#24513,#24514,#24515,#24516,#24517,#24518,#24519,#24520,#24521,
#24522,#24523,#24524,#24525,#24526,#24527,#24528,#24529,#24530,#24531,#24532,
#24533,#24534,#24535,#24536,#24537,#24538,#24539,#24540,#24541,#24542,#24543,
#24544,#24545,#24546,#24547,#24548,#24549,#24550,#24551,#24552,#24553,#24554,
#24555,#24556,#24557,#24558,#24559,#24560,#24561,#24562,#24563,#24564,#24565,
#24566,#24567,#24568,#24569,#24570,#24571,#24572,#24573,#24574,#24575,#24576,
#24577,#24578,#24579,#24580,#24581,#24582,#24583,#24584,#24585,#24586,#24587,
#24588,#24589,#24590,#24591,#24592,#24593,#24594,#24595,#24596,#24597),
 .UNSPECIFIED.,.F.,.F.,(4,3,3,3,3,3,3,3,3,3,3,3,3,3,3,3,3,3,3,3,3,3,3,3,
3,3,3,3,3,3,3,3,3,3,3,3,3,3,3,3,3,3,3,3,3,3,3,3,3,3,3,3,3,3,3,3,4),(204.203522483337,
204.307778401646,204.384614433769,204.461361449496,204.538035687059,204.614653326581,
204.691230503207,204.768099991519,204.844660094041,204.921230391189,204.997825452211,
205.074915691583,205.151642888164,205.228914648931,205.306186409697,205.383781079131,
205.461283345242,205.538708830312,205.616073101689,205.69339168278,205.770687387251,
205.847972431907,205.92526082384,206.002566569366,206.079944609354,206.157359681098,
206.234880295369,206.304594417748,206.386080732181,206.46746281454,206.551546716348,
206.632704035201,206.713784818956,206.79477481099,206.803798421774,206.884811528064,
206.965900222338,207.050175773203,207.131485239593,207.212872140803,207.294379279568,
207.303002425799,207.380530579008,207.457977453969,207.535358632677,207.612689650137,
207.689986004968,207.767276305304,207.844566213042,207.92186973504,207.999200883167,
208.076620372988,208.15408573141,208.231671117708,208.30141043385,208.378267534226,
208.440996940824),.UNSPECIFIED.);
#235=B_SPLINE_CURVE_WITH_KNOTS('',3,(#24603,#24604,#24605,#24606,#24607,
#24608,#24609,#24610,#24611,#24612,#24613,#24614,#24615,#24616,#24617,#24618,
#24619,#24620,#24621,#24622,#24623,#24624,#24625,#24626,#24627,#24628,#24629,
#24630,#24631,#24632,#24633,#24634,#24635,#24636,#24637,#24638,#24639,#24640,
#24641,#24642,#24643,#24644,#24645,#24646,#24647,#24648,#24649,#24650,#24651,
#24652,#24653,#24654,#24655,#24656,#24657,#24658,#24659,#24660,#24661,#24662,
#24663,#24664,#24665,#24666,#24667,#24668,#24669,#24670,#24671,#24672,#24673,
#24674,#24675,#24676,#24677,#24678,#24679,#24680,#24681,#24682,#24683,#24684,
#24685,#24686,#24687,#24688,#24689,#24690,#24691,#24692,#24693,#24694,#24695,
#24696,#24697,#24698,#24699,#24700,#24701,#24702,#24703,#24704,#24705,#24706,
#24707,#24708,#24709,#24710,#24711,#24712,#24713,#24714,#24715,#24716,#24717,
#24718,#24719,#24720,#24721,#24722,#24723,#24724,#24725,#24726,#24727,#24728,
#24729,#24730,#24731,#24732,#24733,#24734,#24735,#24736,#24737,#24738,#24739,
#24740,#24741,#24742,#24743,#24744,#24745,#24746,#24747,#24748,#24749,#24750,
#24751,#24752,#24753,#24754,#24755,#24756,#24757,#24758,#24759,#24760,#24761,
#24762,#24763,#24764,#24765,#24766,#24767,#24768,#24769,#24770,#24771),
 .UNSPECIFIED.,.F.,.F.,(4,3,3,3,3,3,3,3,3,3,3,3,3,3,3,3,3,3,3,3,3,3,3,3,
3,3,3,3,3,3,3,3,3,3,3,3,3,3,3,3,3,3,3,3,3,3,3,3,3,3,3,3,3,3,3,3,4),(210.486707790621,
210.561737282258,210.636722085166,210.711678368504,210.751235556924,210.832243952828,
210.91332820966,210.997774247897,211.079080329604,211.160464119372,211.2419687804,
211.251112362609,211.328628140872,211.406062441283,211.48343085971,211.56074894486,
211.638032208904,211.715309293216,211.792585873703,211.869875969101,211.947193603105,
212.02459980943,212.102051818743,212.179624627065,212.250865973978,212.327714597165,
212.404469443562,212.481146782966,212.557762822741,212.634333721366,212.711369454364,
212.787911873069,212.864460209632,212.94102904108,213.018426677146,213.095117758099,
213.172868671723,213.250619585347,213.328137136965,213.405567356384,213.48292589928,
213.560228369867,213.637490331817,213.7147375576,213.791979068807,213.86922891904,
213.946501163953,214.023854121924,214.101248514233,214.178756841901,214.250373196717,
214.327893335513,214.405328948147,214.48487533695,214.562173789417,214.642844146388,
214.723514503359),.UNSPECIFIED.);
#236=B_SPLINE_CURVE_WITH_KNOTS('',3,(#24772,#24773,#24774,#24775,#24776,
#24777,#24778,#24779,#24780,#24781,#24782,#24783,#24784,#24785,#24786,#24787,
#24788,#24789,#24790,#24791,#24792,#24793,#24794,#24795,#24796,#24797,#24798,
#24799,#24800,#24801,#24802,#24803,#24804,#24805,#24806,#24807,#24808,#24809,
#24810,#24811,#24812,#24813,#24814,#24815,#24816,#24817,#24818,#24819,#24820,
#24821,#24822,#24823,#24824,#24825,#24826,#24827,#24828,#24829,#24830,#24831,
#24832,#24833,#24834,#24835,#24836,#24837,#24838,#24839,#24840,#24841,#24842,
#24843,#24844,#24845,#24846,#24847,#24848,#24849,#24850,#24851,#24852,#24853),
 .UNSPECIFIED.,.F.,.F.,(4,3,3,3,3,3,3,3,3,3,3,3,3,3,3,3,3,3,3,3,3,3,3,3,
3,3,3,4),(208.44084770076,208.517478417994,208.594059812263,208.670608013932,
208.747152814121,208.823699785788,208.900263505226,208.976858556687,209.053543828347,
209.130279301935,209.207129569358,209.25160513987,209.329187763484,209.406677745693,
209.484090722918,209.561442276419,209.63874794333,209.716030536375,209.793302323319,
209.870577323175,209.947869554113,210.025234226478,210.102635834911,210.180143649519,
210.251358751239,210.349353062697,210.44622784609,210.486707790517),
 .UNSPECIFIED.);
#237=B_SPLINE_CURVE_WITH_KNOTS('',3,(#24855,#24856,#24857,#24858,#24859,
#24860,#24861,#24862,#24863,#24864,#24865,#24866,#24867,#24868,#24869,#24870,
#24871,#24872,#24873,#24874,#24875,#24876,#24877,#24878,#24879,#24880,#24881,
#24882,#24883,#24884,#24885,#24886,#24887,#24888,#24889,#24890,#24891,#24892,
#24893,#24894,#24895,#24896,#24897,#24898,#24899,#24900,#24901,#24902,#24903,
#24904,#24905,#24906,#24907,#24908,#24909,#24910,#24911,#24912,#24913,#24914,
#24915,#24916,#24917,#24918,#24919,#24920,#24921,#24922,#24923,#24924,#24925,
#24926,#24927,#24928,#24929,#24930,#24931,#24932,#24933,#24934,#24935,#24936),
 .UNSPECIFIED.,.F.,.F.,(4,3,3,3,3,3,3,3,3,3,3,3,3,3,3,3,3,3,3,3,3,3,3,3,
3,3,3,4),(208.440996940824,208.517702413484,208.594343824787,208.670937329106,
208.749547468205,208.826106181576,208.902668573492,208.979249209891,209.059391517893,
209.136092755801,209.212846284827,209.289699924151,209.299818441901,209.377348638361,
209.454791732966,209.532163367022,209.609479130591,209.686754573369,209.764015455789,
209.841270761433,209.918534531727,209.995820810212,210.073187623004,210.150595957711,
210.228117514274,210.298226449952,210.4108480197,210.486707790517),
 .UNSPECIFIED.);
#238=B_SPLINE_CURVE_WITH_KNOTS('',3,(#24937,#24938,#24939,#24940,#24941,
#24942,#24943,#24944,#24945,#24946,#24947,#24948,#24949,#24950,#24951,#24952,
#24953,#24954,#24955,#24956,#24957,#24958,#24959,#24960,#24961,#24962,#24963,
#24964,#24965,#24966,#24967,#24968,#24969,#24970,#24971,#24972,#24973,#24974,
#24975,#24976,#24977,#24978,#24979,#24980,#24981,#24982,#24983,#24984,#24985,
#24986,#24987,#24988,#24989,#24990,#24991,#24992,#24993,#24994,#24995,#24996,
#24997,#24998,#24999,#25000,#25001,#25002,#25003,#25004,#25005,#25006,#25007,
#25008,#25009,#25010,#25011,#25012,#25013,#25014,#25015,#25016,#25017,#25018,
#25019,#25020,#25021,#25022,#25023,#25024,#25025,#25026,#25027,#25028,#25029,
#25030,#25031,#25032,#25033,#25034,#25035,#25036,#25037,#25038,#25039,#25040,
#25041,#25042,#25043,#25044,#25045,#25046,#25047,#25048,#25049,#25050,#25051,
#25052,#25053,#25054,#25055,#25056,#25057,#25058,#25059,#25060,#25061,#25062,
#25063,#25064,#25065,#25066,#25067,#25068,#25069,#25070,#25071,#25072,#25073,
#25074,#25075,#25076,#25077,#25078,#25079,#25080,#25081,#25082,#25083,#25084,
#25085,#25086,#25087,#25088,#25089,#25090,#25091,#25092,#25093,#25094,#25095,
#25096,#25097,#25098,#25099,#25100,#25101,#25102,#25103,#25104,#25105,#25106,
#25107,#25108),.UNSPECIFIED.,.F.,.F.,(4,3,3,3,3,3,3,3,3,3,3,3,3,3,3,3,3,
3,3,3,3,3,3,3,3,3,3,3,3,3,3,3,3,3,3,3,3,3,3,3,3,3,3,3,3,3,3,3,3,3,3,3,3,
3,3,3,3,4),(210.486707790615,210.56305843767,210.639348328246,210.715593890765,
210.791820201114,210.868038882577,210.944264751554,211.020512627365,211.09683785511,
211.173205632822,211.249678514956,211.296634458003,211.373470490126,211.450217505853,
211.526891743416,211.603509382938,211.680086559565,211.756956047876,211.833516150399,
211.910086447546,211.986681508569,212.06377174794,212.140498944522,212.217770705288,
212.295042466054,212.372637135488,212.450139401598,212.527564886669,212.604929158045,
212.682247739136,212.759543443608,212.836828488264,212.914116880197,212.991422625723,
213.06880066571,213.146215737455,213.223736351726,213.293450474105,213.374936788538,
213.456318870897,213.540402772705,213.621560091558,213.702640875313,213.783630867346,
213.79265447813,213.873667584421,213.954756278693,214.039031829559,214.120341295949,
214.20172819716,214.283235335925,214.291858482156,214.369393170772,214.446848326865,
214.524224655243,214.601555290006,214.678852783169,214.723504023201),
 .UNSPECIFIED.);
#239=B_SPLINE_CURVE_WITH_KNOTS('',3,(#25114,#25115,#25116,#25117,#25118,
#25119,#25120,#25121,#25122,#25123,#25124,#25125,#25126,#25127,#25128,#25129,
#25130,#25131,#25132,#25133,#25134,#25135,#25136,#25137,#25138,#25139,#25140,
#25141,#25142,#25143,#25144,#25145,#25146,#25147,#25148,#25149,#25150,#25151,
#25152,#25153,#25154,#25155,#25156,#25157,#25158,#25159,#25160,#25161,#25162,
#25163,#25164,#25165,#25166,#25167,#25168,#25169,#25170,#25171,#25172,#25173,
#25174,#25175,#25176,#25177,#25178,#25179,#25180,#25181,#25182,#25183,#25184,
#25185,#25186,#25187,#25188,#25189,#25190,#25191,#25192,#25193,#25194,#25195,
#25196,#25197,#25198,#25199,#25200,#25201,#25202,#25203,#25204,#25205,#25206,
#25207,#25208,#25209,#25210,#25211,#25212,#25213,#25214,#25215,#25216,#25217,
#25218,#25219,#25220,#25221,#25222,#25223,#25224,#25225,#25226,#25227,#25228,
#25229,#25230,#25231,#25232,#25233,#25234,#25235,#25236,#25237,#25238,#25239,
#25240,#25241,#25242,#25243,#25244,#25245,#25246,#25247,#25248,#25249,#25250,
#25251,#25252,#25253,#25254,#25255,#25256,#25257,#25258,#25259,#25260,#25261,
#25262,#25263,#25264,#25265,#25266,#25267,#25268,#25269,#25270,#25271,#25272,
#25273,#25274,#25275,#25276,#25277,#25278,#25279,#25280,#25281,#25282),
 .UNSPECIFIED.,.F.,.F.,(4,3,3,3,3,3,3,3,3,3,3,3,3,3,3,3,3,3,3,3,3,3,3,3,
3,3,3,3,3,3,3,3,3,3,3,3,3,3,3,3,3,3,3,3,3,3,3,3,3,3,3,3,3,3,3,3,4),(216.769893157937,
216.850458882996,216.931110322007,217.011923257324,217.092818695108,217.173879256297,
217.249634030825,217.33111800378,217.412497367919,217.496750735067,217.577904230238,
217.658980908197,217.739966335986,217.74951083651,217.830519232414,217.911603489246,
217.996049527483,218.077355609191,218.158739398959,218.240244059988,218.249387642194,
218.326903420457,218.404337720868,218.481706139295,218.559024224445,218.636307488489,
218.713584572801,218.790861153289,218.868151248686,218.94546888269,219.022875089015,
219.100327098329,219.177899906651,219.249141253564,219.325989876751,219.402744723148,
219.479422062552,219.556038102327,219.632609000952,219.709644733949,219.786187152655,
219.862735489217,219.939304320665,220.016701956732,220.093393037685,220.171143951309,
220.248894864933,220.326425925142,220.403866965942,220.481217794065,220.558516873395,
220.635778303344,220.713016159321,220.790261594575,220.867509085248,220.944801936219,
221.00595800351),.UNSPECIFIED.);
#240=B_SPLINE_CURVE_WITH_KNOTS('',3,(#25283,#25284,#25285,#25286,#25287,
#25288,#25289,#25290,#25291,#25292,#25293,#25294,#25295,#25296,#25297,#25298,
#25299,#25300,#25301,#25302,#25303,#25304,#25305,#25306,#25307,#25308,#25309,
#25310,#25311,#25312,#25313,#25314,#25315,#25316,#25317,#25318,#25319,#25320,
#25321,#25322,#25323,#25324,#25325,#25326,#25327,#25328,#25329,#25330,#25331,
#25332,#25333,#25334,#25335,#25336,#25337,#25338,#25339,#25340,#25341,#25342,
#25343,#25344,#25345,#25346,#25347,#25348,#25349,#25350,#25351,#25352,#25353,
#25354,#25355,#25356,#25357,#25358,#25359,#25360,#25361,#25362,#25363,#25364),
 .UNSPECIFIED.,.F.,.F.,(4,3,3,3,3,3,3,3,3,3,3,3,3,3,3,3,3,3,3,3,3,3,3,3,
3,3,3,4),(214.723514503359,214.800756280101,214.878008065805,214.955283916887,
215.032641176327,215.110041371675,215.187553084504,215.250126808086,215.326948005241,
215.403679967455,215.480338945602,215.556941132064,215.633502673945,215.710549892134,
215.787094066779,215.863648346824,215.940227311803,216.017640588716,216.094352069023,
216.172116244239,216.249880419456,216.331821893514,216.413627368325,216.49530143724,
216.576798267279,216.658187206882,216.739434041545,216.769893097697),
 .UNSPECIFIED.);
#241=B_SPLINE_CURVE_WITH_KNOTS('',3,(#25366,#25367,#25368,#25369,#25370,
#25371,#25372,#25373,#25374,#25375,#25376,#25377,#25378,#25379,#25380,#25381,
#25382,#25383,#25384,#25385,#25386,#25387,#25388,#25389,#25390,#25391,#25392,
#25393,#25394,#25395,#25396,#25397,#25398,#25399,#25400,#25401,#25402,#25403,
#25404,#25405,#25406,#25407,#25408,#25409,#25410,#25411,#25412,#25413,#25414,
#25415,#25416,#25417,#25418,#25419,#25420,#25421,#25422,#25423,#25424,#25425,
#25426,#25427,#25428,#25429,#25430,#25431,#25432,#25433,#25434,#25435,#25436,
#25437,#25438,#25439,#25440,#25441,#25442,#25443,#25444,#25445,#25446,#25447),
 .UNSPECIFIED.,.F.,.F.,(4,3,3,3,3,3,3,3,3,3,3,3,3,3,3,3,3,3,3,3,3,3,3,3,
3,3,3,4),(214.723504023201,214.800792388271,214.878088454244,214.955406229928,
215.032759733642,215.110204171467,215.187701769873,215.265306891419,215.290266490207,
215.367129874859,215.443899706669,215.520592242657,215.597223677824,215.673810158607,
215.750668201063,215.827226524026,215.903790858699,215.980375771825,216.057450453433,
216.134157274302,216.21141588628,216.288674498257,216.371275620547,216.453735688925,
216.535990978226,216.618123682984,216.700074313751,216.769893097696),
 .UNSPECIFIED.);
#242=B_SPLINE_CURVE_WITH_KNOTS('',3,(#25448,#25449,#25450,#25451,#25452,
#25453,#25454,#25455,#25456,#25457,#25458,#25459,#25460,#25461,#25462,#25463,
#25464,#25465,#25466,#25467,#25468,#25469,#25470,#25471,#25472,#25473,#25474,
#25475,#25476,#25477,#25478,#25479,#25480,#25481,#25482,#25483,#25484,#25485,
#25486,#25487,#25488,#25489,#25490,#25491,#25492,#25493,#25494,#25495,#25496,
#25497,#25498,#25499,#25500,#25501,#25502,#25503,#25504,#25505,#25506,#25507,
#25508,#25509,#25510,#25511,#25512,#25513,#25514,#25515,#25516,#25517,#25518,
#25519,#25520,#25521,#25522,#25523,#25524,#25525,#25526,#25527,#25528,#25529,
#25530,#25531,#25532,#25533,#25534,#25535,#25536,#25537,#25538,#25539,#25540,
#25541,#25542,#25543,#25544,#25545,#25546,#25547,#25548,#25549,#25550,#25551,
#25552,#25553,#25554,#25555,#25556,#25557,#25558,#25559,#25560,#25561,#25562,
#25563,#25564,#25565,#25566,#25567,#25568,#25569,#25570,#25571,#25572,#25573,
#25574,#25575,#25576,#25577,#25578,#25579,#25580,#25581,#25582,#25583,#25584,
#25585,#25586,#25587,#25588,#25589,#25590,#25591,#25592,#25593,#25594,#25595,
#25596,#25597,#25598,#25599,#25600,#25601,#25602,#25603,#25604),
 .UNSPECIFIED.,.F.,.F.,(4,3,3,3,3,3,3,3,3,3,3,3,3,3,3,3,3,3,3,3,3,3,3,3,
3,3,3,3,3,3,3,3,3,3,3,3,3,3,3,3,3,3,3,3,3,3,3,3,3,3,3,3,4),(216.769893097696,
216.852355303732,216.934817161472,217.017278677766,217.099739859463,217.182200713414,
217.264661246469,217.347121465475,217.429581377283,217.512040988741,217.594500306697,
217.676959337999,217.759418089496,217.841876568034,217.924334780462,218.006792733627,
218.089250434374,218.171707889552,218.254165106007,218.340177332509,218.423501676932,
218.505968282378,218.588434043619,218.670898988072,218.753363143148,218.835826536257,
218.918289194805,219.000751146198,219.083212417837,219.165673037121,219.248133031448,
219.330592428212,219.413051254807,219.495509538624,219.577967307051,219.660424587477,
219.744557822888,219.82702382098,219.909488197335,219.991951061598,220.074412523388,
220.156872692309,220.239331677945,220.321789589862,220.407385435387,220.489850171987,
220.572311943989,220.654771189831,220.737228347808,220.819690866089,220.902148536944,
220.984607326895,221.00655635406),.UNSPECIFIED.);
#243=B_SPLINE_CURVE_WITH_KNOTS('',3,(#25610,#25611,#25612,#25613,#25614,
#25615,#25616,#25617,#25618,#25619,#25620,#25621,#25622,#25623,#25624,#25625,
#25626,#25627,#25628,#25629,#25630,#25631,#25632,#25633,#25634,#25635,#25636,
#25637,#25638,#25639,#25640,#25641,#25642,#25643,#25644,#25645,#25646,#25647,
#25648,#25649,#25650,#25651,#25652,#25653,#25654,#25655,#25656,#25657,#25658,
#25659,#25660,#25661,#25662,#25663,#25664,#25665,#25666,#25667,#25668,#25669,
#25670,#25671,#25672,#25673,#25674,#25675,#25676,#25677,#25678,#25679,#25680,
#25681,#25682,#25683,#25684,#25685,#25686,#25687,#25688,#25689,#25690,#25691,
#25692,#25693,#25694,#25695,#25696,#25697,#25698,#25699,#25700,#25701,#25702,
#25703,#25704,#25705,#25706,#25707,#25708,#25709,#25710,#25711,#25712,#25713,
#25714,#25715,#25716,#25717,#25718,#25719,#25720,#25721,#25722,#25723,#25724,
#25725,#25726,#25727,#25728,#25729,#25730,#25731,#25732,#25733,#25734,#25735,
#25736,#25737,#25738,#25739,#25740,#25741,#25742,#25743,#25744,#25745,#25746,
#25747,#25748,#25749,#25750,#25751,#25752,#25753,#25754,#25755,#25756,#25757,
#25758,#25759,#25760,#25761,#25762,#25763,#25764,#25765,#25766),
 .UNSPECIFIED.,.F.,.F.,(4,3,3,3,3,3,3,3,3,3,3,3,3,3,3,3,3,3,3,3,3,3,3,3,
3,3,3,3,3,3,3,3,3,3,3,3,3,3,3,3,3,3,3,3,3,3,3,3,3,3,3,3,4),(223.053078404876,
223.135540610912,223.218002468652,223.300463984946,223.382925166643,223.465386020594,
223.547846553649,223.630306772655,223.712766684463,223.795226295921,223.877685613877,
223.960144645179,224.042603396676,224.125061875214,224.207520087642,224.289978040806,
224.372435741554,224.454893196732,224.537350413187,224.623362639688,224.706686984112,
224.789153589557,224.871619350799,224.954084295251,225.036548450327,225.119011843436,
225.201474501985,225.283936453377,225.366397725016,225.4488583443,225.531318338627,
225.613777735392,225.696236561987,225.778694845803,225.861152614231,225.943609894656,
226.027743130068,226.110209128159,226.192673504515,226.275136368777,226.357597830568,
226.440057999489,226.522516985125,226.604974897042,226.690570742567,226.773035479167,
226.855497251169,226.937956497011,227.020413654988,227.102876173269,227.185333844124,
227.267792634075,227.28974166124),.UNSPECIFIED.);
#244=B_SPLINE_CURVE_WITH_KNOTS('',3,(#25767,#25768,#25769,#25770,#25771,
#25772,#25773,#25774,#25775,#25776,#25777,#25778,#25779,#25780,#25781,#25782,
#25783,#25784,#25785,#25786,#25787,#25788,#25789,#25790,#25791,#25792,#25793,
#25794,#25795,#25796,#25797,#25798,#25799,#25800,#25801,#25802,#25803,#25804,
#25805,#25806,#25807,#25808,#25809,#25810,#25811,#25812,#25813,#25814,#25815,
#25816,#25817,#25818,#25819,#25820,#25821,#25822,#25823,#25824,#25825,#25826,
#25827,#25828,#25829,#25830,#25831,#25832,#25833,#25834,#25835,#25836,#25837,
#25838,#25839,#25840,#25841,#25842,#25843,#25844,#25845,#25846,#25847,#25848,
#25849,#25850,#25851),.UNSPECIFIED.,.F.,.F.,(4,3,3,3,3,3,3,3,3,3,3,3,3,
3,3,3,3,3,3,3,3,3,3,3,3,3,3,3,4),(221.00595800351,221.083342689106,221.160778822706,
221.238313030152,221.248648476302,221.326165845499,221.403595912951,221.480954334221,
221.558256713437,221.6355186142,221.712765824892,221.790007349111,221.867257240458,
221.944529554602,222.021882625829,222.099277155581,222.176785660544,222.248402087672,
222.324092888759,222.39969460951,222.475224219875,222.550694126437,222.626131444521,
222.701551365929,222.776969066577,222.852428778147,222.927910739162,223.003468440949,
223.05190658296),.UNSPECIFIED.);
#245=B_SPLINE_CURVE_WITH_KNOTS('',3,(#25853,#25854,#25855,#25856,#25857,
#25858,#25859,#25860,#25861,#25862,#25863,#25864,#25865,#25866,#25867,#25868,
#25869,#25870,#25871,#25872,#25873,#25874,#25875,#25876,#25877,#25878,#25879,
#25880,#25881,#25882,#25883,#25884,#25885,#25886,#25887,#25888,#25889,#25890,
#25891,#25892,#25893,#25894,#25895,#25896,#25897,#25898,#25899,#25900,#25901,
#25902,#25903,#25904,#25905,#25906,#25907,#25908,#25909,#25910,#25911,#25912,
#25913,#25914,#25915,#25916,#25917,#25918,#25919,#25920,#25921,#25922,#25923,
#25924,#25925,#25926,#25927,#25928),.UNSPECIFIED.,.F.,.F.,(4,3,3,3,3,3,
3,3,3,3,3,3,3,3,3,3,3,3,3,3,3,3,3,3,3,4),(221.00655635406,221.089017957914,
221.171478895885,221.25393919537,221.336398883767,221.418857988469,221.501316536869,
221.583774556355,221.666232074316,221.75290996997,221.835376755805,221.917841869149,
222.000305419654,222.082767516952,222.165228270653,222.24768779035,222.330146185618,
222.412603566015,222.495069952282,222.577533154295,222.659993610576,222.742451759487,
222.824917364366,222.90737724358,222.989841356944,223.053078404766),
 .UNSPECIFIED.);
#246=B_SPLINE_CURVE_WITH_KNOTS('',3,(#25929,#25930,#25931,#25932,#25933,
#25934,#25935,#25936,#25937,#25938,#25939,#25940,#25941,#25942,#25943,#25944,
#25945,#25946,#25947,#25948,#25949,#25950,#25951,#25952,#25953,#25954,#25955,
#25956,#25957,#25958,#25959,#25960,#25961,#25962,#25963,#25964,#25965,#25966,
#25967,#25968,#25969,#25970,#25971,#25972,#25973,#25974,#25975,#25976,#25977,
#25978,#25979,#25980,#25981,#25982,#25983,#25984,#25985,#25986,#25987,#25988,
#25989,#25990,#25991,#25992,#25993,#25994,#25995,#25996,#25997,#25998,#25999,
#26000,#26001,#26002,#26003,#26004,#26005,#26006,#26007,#26008,#26009,#26010,
#26011,#26012,#26013,#26014,#26015,#26016,#26017,#26018,#26019,#26020,#26021,
#26022,#26023,#26024,#26025,#26026,#26027,#26028,#26029,#26030,#26031,#26032,
#26033,#26034,#26035,#26036,#26037,#26038,#26039,#26040,#26041,#26042,#26043,
#26044,#26045,#26046,#26047,#26048,#26049,#26050,#26051,#26052,#26053,#26054,
#26055,#26056,#26057,#26058,#26059,#26060,#26061,#26062,#26063,#26064,#26065,
#26066,#26067,#26068,#26069,#26070,#26071,#26072,#26073,#26074,#26075,#26076,
#26077,#26078,#26079,#26080,#26081,#26082,#26083,#26084,#26085),
 .UNSPECIFIED.,.F.,.F.,(4,3,3,3,3,3,3,3,3,3,3,3,3,3,3,3,3,3,3,3,3,3,3,3,
3,3,3,3,3,3,3,3,3,3,3,3,3,3,3,3,3,3,3,3,3,3,3,3,3,3,3,3,4),(223.053078404876,
223.135540610912,223.218002468652,223.300463984946,223.382925166643,223.465386020595,
223.547846553649,223.630306772655,223.712766684463,223.795226295921,223.877685613877,
223.960144645179,224.042603396676,224.125061875214,224.207520087642,224.289978040806,
224.372435741554,224.454893196732,224.537350413186,224.623362639688,224.706686984112,
224.789153589557,224.871619350799,224.954084295251,225.036548450327,225.119011843436,
225.201474501985,225.283936453377,225.366397725016,225.4488583443,225.531318338627,
225.613777735391,225.696236561987,225.778694845803,225.861152614231,225.943609894656,
226.027743130068,226.110209128159,226.192673504515,226.275136368777,226.357597830568,
226.440057999489,226.522516985124,226.604974897041,226.690570742566,226.773035479166,
226.855497251168,226.93795649701,227.020413654987,227.102876173269,227.185333844124,
227.267792634074,227.28974166124),.UNSPECIFIED.);
#247=B_SPLINE_CURVE_WITH_KNOTS('',3,(#26091,#26092,#26093,#26094,#26095,
#26096,#26097,#26098,#26099,#26100,#26101,#26102,#26103,#26104,#26105,#26106,
#26107,#26108,#26109,#26110,#26111,#26112,#26113,#26114,#26115,#26116,#26117,
#26118,#26119,#26120,#26121,#26122,#26123,#26124,#26125,#26126,#26127,#26128,
#26129,#26130,#26131,#26132,#26133,#26134,#26135,#26136,#26137,#26138,#26139,
#26140,#26141,#26142,#26143,#26144,#26145,#26146,#26147,#26148,#26149,#26150,
#26151,#26152,#26153,#26154,#26155,#26156,#26157,#26158,#26159,#26160,#26161,
#26162,#26163,#26164,#26165,#26166,#26167,#26168,#26169,#26170,#26171,#26172,
#26173,#26174,#26175,#26176,#26177,#26178,#26179,#26180,#26181,#26182,#26183,
#26184,#26185,#26186,#26187,#26188,#26189,#26190,#26191,#26192,#26193,#26194,
#26195,#26196,#26197,#26198,#26199,#26200,#26201,#26202,#26203,#26204,#26205,
#26206,#26207,#26208,#26209,#26210,#26211,#26212,#26213,#26214,#26215,#26216,
#26217,#26218,#26219,#26220,#26221,#26222,#26223,#26224,#26225,#26226,#26227,
#26228,#26229,#26230,#26231,#26232,#26233,#26234,#26235,#26236,#26237,#26238,
#26239,#26240,#26241,#26242,#26243,#26244,#26245,#26246,#26247,#26248,#26249,
#26250,#26251,#26252,#26253,#26254,#26255,#26256,#26257,#26258,#26259,#26260,
#26261,#26262),.UNSPECIFIED.,.F.,.F.,(4,3,3,3,3,3,3,3,3,3,3,3,3,3,3,3,3,
3,3,3,3,3,3,3,3,3,3,3,3,3,3,3,3,3,3,3,3,3,3,3,3,3,3,3,3,3,3,3,3,3,3,3,3,
3,3,3,3,4),(229.336901162253,229.412795891483,229.488610273219,229.56436110011,
229.640065098054,229.715860833126,229.791534894963,229.867214836791,229.942915732088,
230.018794543723,230.094620344256,230.170567362008,230.246430978627,230.324013601862,
230.401503583692,230.478916560538,230.55626811366,230.633573780193,230.710856372862,
230.788128159431,230.865403158915,230.942695389483,231.020060061483,231.097461669552,
231.174969483806,231.246184589996,231.327668566192,231.409047933538,231.493301299074,
231.57445479732,231.655531478291,231.736516908996,231.746061395681,231.827069786551,
231.908154038244,231.992600079024,232.073906155435,232.155289939871,232.236794595554,
232.245938201365,232.323453981237,232.400888283264,232.478256703313,232.55557479009,
232.632858055762,232.710135141701,232.787411723814,232.864701820835,232.942019456458,
233.019425664387,233.096877675298,233.174450485193,233.245691812735,233.322562143436,
233.399313507969,233.475996166199,233.552611946368,233.573644710383),
 .UNSPECIFIED.);
#248=B_SPLINE_CURVE_WITH_KNOTS('',3,(#26263,#26264,#26265,#26266,#26267,
#26268,#26269,#26270,#26271,#26272,#26273,#26274,#26275,#26276,#26277,#26278,
#26279,#26280,#26281,#26282,#26283,#26284,#26285,#26286,#26287,#26288,#26289,
#26290,#26291,#26292,#26293,#26294,#26295,#26296,#26297,#26298,#26299,#26300,
#26301,#26302,#26303,#26304,#26305,#26306,#26307,#26308,#26309,#26310,#26311,
#26312,#26313,#26314,#26315,#26316,#26317,#26318,#26319,#26320,#26321,#26322,
#26323,#26324,#26325,#26326,#26327,#26328,#26329,#26330,#26331,#26332,#26333,
#26334,#26335,#26336,#26337,#26338),.UNSPECIFIED.,.F.,.F.,(4,3,3,3,3,3,
3,3,3,3,3,3,3,3,3,3,3,3,3,3,3,3,3,3,3,4),(227.28974166124,227.372203265094,
227.454664203065,227.53712450255,227.619584190947,227.702043295649,227.784501844048,
227.866959863535,227.949417381496,228.036095277156,228.118562062992,228.201027176336,
228.283490726841,228.365952824138,228.44841357784,228.530873097537,228.613331492805,
228.695788873202,228.778255259468,228.860718461482,228.943178917763,229.025637066673,
229.108102671553,229.190562550767,229.273026664131,229.336263712056),
 .UNSPECIFIED.);
#249=B_SPLINE_CURVE_WITH_KNOTS('',3,(#26340,#26341,#26342,#26343,#26344,
#26345,#26346,#26347,#26348,#26349,#26350,#26351,#26352,#26353,#26354,#26355,
#26356,#26357,#26358,#26359,#26360,#26361,#26362,#26363,#26364,#26365,#26366,
#26367,#26368,#26369,#26370,#26371,#26372,#26373,#26374,#26375,#26376,#26377,
#26378,#26379,#26380,#26381,#26382,#26383,#26384,#26385,#26386,#26387,#26388,
#26389,#26390,#26391,#26392,#26393,#26394,#26395,#26396,#26397,#26398,#26399,
#26400,#26401,#26402,#26403,#26404,#26405,#26406,#26407,#26408,#26409,#26410,
#26411,#26412,#26413,#26414,#26415),.UNSPECIFIED.,.F.,.F.,(4,3,3,3,3,3,
3,3,3,3,3,3,3,3,3,3,3,3,3,3,3,3,3,3,3,4),(227.28974166124,227.372203265094,
227.454664203065,227.53712450255,227.619584190947,227.702043295649,227.784501844048,
227.866959863535,227.949417381496,228.036095277156,228.118562062992,228.201027176336,
228.283490726841,228.365952824139,228.44841357784,228.530873097537,228.613331492805,
228.695788873202,228.778255259468,228.860718461482,228.943178917763,229.025637066674,
229.108102671553,229.190562550767,229.273026664131,229.336263712056),
 .UNSPECIFIED.);
#250=B_SPLINE_CURVE_WITH_KNOTS('',3,(#26416,#26417,#26418,#26419,#26420,
#26421,#26422,#26423,#26424,#26425,#26426,#26427,#26428,#26429,#26430,#26431,
#26432,#26433,#26434,#26435,#26436,#26437,#26438,#26439,#26440,#26441,#26442,
#26443,#26444,#26445,#26446,#26447,#26448,#26449,#26450,#26451,#26452,#26453,
#26454,#26455,#26456,#26457,#26458,#26459,#26460,#26461,#26462,#26463,#26464,
#26465,#26466,#26467,#26468,#26469,#26470,#26471,#26472,#26473,#26474,#26475,
#26476,#26477,#26478,#26479,#26480,#26481,#26482,#26483,#26484,#26485,#26486,
#26487,#26488,#26489,#26490,#26491,#26492,#26493,#26494,#26495,#26496,#26497,
#26498,#26499,#26500,#26501,#26502,#26503,#26504,#26505,#26506,#26507,#26508,
#26509,#26510,#26511,#26512,#26513,#26514,#26515,#26516,#26517,#26518,#26519,
#26520,#26521,#26522,#26523,#26524,#26525,#26526,#26527,#26528,#26529,#26530,
#26531,#26532,#26533,#26534,#26535,#26536,#26537,#26538,#26539,#26540,#26541,
#26542,#26543,#26544,#26545,#26546,#26547,#26548,#26549,#26550,#26551,#26552,
#26553,#26554,#26555,#26556,#26557,#26558,#26559,#26560,#26561,#26562,#26563,
#26564,#26565,#26566,#26567,#26568,#26569,#26570,#26571,#26572,#26573,#26574,
#26575,#26576,#26577,#26578,#26579,#26580,#26581,#26582,#26583,#26584),
 .UNSPECIFIED.,.F.,.F.,(4,3,3,3,3,3,3,3,3,3,3,3,3,3,3,3,3,3,3,3,3,3,3,3,
3,3,3,3,3,3,3,3,3,3,3,3,3,3,3,3,3,3,3,3,3,3,3,3,3,3,3,3,3,3,3,3,4),(229.336929791429,
229.413011331548,229.489005470862,229.564928948207,229.640798431607,229.718996954027,
229.794819117296,229.870640824301,229.946477073216,230.022342871793,230.098291275127,
230.174289251926,230.250387401808,230.26638661097,230.343916807397,230.42135990197,
230.498731535993,230.57604729953,230.653322742275,230.730583624662,230.807838930274,
230.885102700535,230.962388978987,231.039755791747,231.117164126422,231.194685682953,
231.264794619021,231.34232473716,231.419767766552,231.497139348453,231.574455072888,
231.651730489525,231.728991365625,231.806246677046,231.883510465212,231.96079677367,
232.038163635349,232.115572029353,232.193093662296,232.263202627072,232.340038659166,
232.416785674865,232.4934599124,232.570077551894,232.646654728493,232.723524216822,
232.800084319319,232.876654616441,232.953249677439,233.03033991686,233.107067113419,
233.184338874271,233.261610635123,233.339561228579,233.417062450996,233.495237729972,
233.573413008948),.UNSPECIFIED.);
#251=B_SPLINE_CURVE_WITH_KNOTS('',3,(#26590,#26591,#26592,#26593,#26594,
#26595,#26596,#26597,#26598,#26599,#26600,#26601,#26602,#26603,#26604,#26605,
#26606,#26607,#26608,#26609,#26610,#26611,#26612,#26613,#26614,#26615,#26616,
#26617,#26618,#26619,#26620,#26621,#26622,#26623,#26624,#26625,#26626,#26627,
#26628,#26629,#26630,#26631,#26632,#26633,#26634,#26635,#26636,#26637,#26638,
#26639,#26640,#26641,#26642,#26643,#26644,#26645,#26646,#26647,#26648,#26649,
#26650,#26651,#26652,#26653,#26654,#26655,#26656,#26657,#26658,#26659,#26660,
#26661,#26662,#26663,#26664,#26665,#26666,#26667,#26668,#26669,#26670,#26671,
#26672,#26673,#26674,#26675,#26676,#26677,#26678,#26679,#26680,#26681,#26682,
#26683,#26684,#26685,#26686,#26687,#26688,#26689,#26690,#26691,#26692,#26693,
#26694,#26695,#26696,#26697,#26698,#26699,#26700,#26701,#26702,#26703,#26704,
#26705,#26706,#26707,#26708,#26709,#26710,#26711,#26712,#26713,#26714,#26715,
#26716,#26717,#26718,#26719,#26720,#26721,#26722,#26723,#26724,#26725,#26726,
#26727,#26728,#26729,#26730,#26731,#26732,#26733,#26734,#26735,#26736,#26737,
#26738,#26739,#26740,#26741,#26742,#26743,#26744,#26745,#26746,#26747,#26748,
#26749,#26750,#26751,#26752,#26753,#26754,#26755,#26756,#26757,#26758),
 .UNSPECIFIED.,.F.,.F.,(4,3,3,3,3,3,3,3,3,3,3,3,3,3,3,3,3,3,3,3,3,3,3,3,
3,3,3,3,3,3,3,3,3,3,3,3,3,3,3,3,3,3,3,3,3,3,3,3,3,3,3,3,3,3,3,3,4),(235.619449019235,
235.697636972686,235.775661087235,235.853706983637,235.931787708974,236.010078943441,
236.08830869253,236.166667592051,236.244952646843,236.321773856025,236.398505830341,
236.475164820654,236.551767019336,236.628328573482,236.705375784073,236.781919971036,
236.858474263409,236.935053240718,237.012466495091,237.089177987635,237.166942122923,
237.244706258212,237.322288813279,237.399778727044,237.477191635997,237.554543121465,
237.631848720652,237.709131246666,237.786402967016,237.863677900776,237.940970066177,
238.018334674233,238.095736218936,238.173243971391,238.244459869582,238.325944237156,
238.407323990691,238.491577161835,238.572731027894,238.653808068408,238.734793845643,
238.744336675266,238.825344565016,238.90642830662,238.990874600203,239.072180154111,
239.153563413515,239.235067544458,239.244213480951,239.321720046175,239.39914970984,
239.476516599848,239.553834805187,239.631122514021,239.708390676439,239.785671978346,
239.855757872884),.UNSPECIFIED.);
#252=B_SPLINE_CURVE_WITH_KNOTS('',3,(#26759,#26760,#26761,#26762,#26763,
#26764,#26765,#26766,#26767,#26768,#26769,#26770,#26771,#26772,#26773,#26774,
#26775,#26776,#26777,#26778,#26779,#26780,#26781,#26782,#26783,#26784,#26785,
#26786,#26787,#26788,#26789,#26790,#26791,#26792,#26793,#26794,#26795,#26796,
#26797,#26798,#26799,#26800,#26801,#26802,#26803,#26804,#26805,#26806,#26807,
#26808,#26809,#26810,#26811,#26812,#26813,#26814,#26815,#26816,#26817,#26818,
#26819,#26820,#26821,#26822,#26823,#26824,#26825,#26826,#26827,#26828,#26829,
#26830,#26831,#26832,#26833,#26834,#26835,#26836,#26837,#26838,#26839,#26840),
 .UNSPECIFIED.,.F.,.F.,(4,3,3,3,3,3,3,3,3,3,3,3,3,3,3,3,3,3,3,3,3,3,3,3,
3,3,3,4),(233.573644710383,233.650206026682,233.726753347748,233.803295926123,
233.879848336966,233.956425159158,234.033084777737,234.10978853501,234.186605455697,
234.245445424104,234.322962968516,234.400393180715,234.477751716383,234.555054179741,
234.63231613447,234.709563353064,234.786804857104,234.864054700197,234.941326938003,
235.018679888958,235.09607427429,235.173582595113,235.245199035474,235.332641113957,
235.419691044101,235.506472933431,235.592824860091,235.619449019142),
 .UNSPECIFIED.);
#253=B_SPLINE_CURVE_WITH_KNOTS('',3,(#26842,#26843,#26844,#26845,#26846,
#26847,#26848,#26849,#26850,#26851,#26852,#26853,#26854,#26855,#26856,#26857,
#26858,#26859,#26860,#26861,#26862,#26863,#26864,#26865,#26866,#26867,#26868,
#26869,#26870,#26871,#26872,#26873,#26874,#26875,#26876,#26877,#26878,#26879,
#26880,#26881,#26882,#26883,#26884,#26885,#26886,#26887,#26888,#26889,#26890,
#26891,#26892,#26893,#26894,#26895,#26896,#26897,#26898,#26899,#26900,#26901,
#26902,#26903,#26904,#26905,#26906,#26907,#26908,#26909,#26910,#26911,#26912,
#26913,#26914,#26915,#26916,#26917,#26918,#26919,#26920,#26921,#26922,#26923,
#26924,#26925,#26926),.UNSPECIFIED.,.F.,.F.,(4,3,3,3,3,3,3,3,3,3,3,3,3,
3,3,3,3,3,3,3,3,3,3,3,3,3,3,3,4),(233.573413008948,233.650730654674,233.728025925574,
233.805310883667,233.882599535934,233.959905888768,234.037284693043,234.114700841062,
234.19222204831,234.260018643174,234.341504960257,234.422887045237,234.506970945728,
234.588128267094,234.66920905331,234.750199047725,234.759222647199,234.840235749427,
234.921324439555,235.005599992472,235.086909454592,235.168296351503,235.249803485959,
235.258426651225,235.348682243228,235.435146195971,235.521372742441,235.607236547391,
235.619449019235),.UNSPECIFIED.);
#254=B_SPLINE_CURVE_WITH_KNOTS('',3,(#26927,#26928,#26929,#26930,#26931,
#26932,#26933,#26934,#26935,#26936,#26937,#26938,#26939,#26940,#26941,#26942,
#26943,#26944,#26945,#26946,#26947,#26948,#26949,#26950,#26951,#26952,#26953,
#26954,#26955,#26956,#26957,#26958,#26959,#26960,#26961,#26962,#26963,#26964,
#26965,#26966,#26967,#26968,#26969,#26970,#26971,#26972,#26973,#26974,#26975,
#26976,#26977,#26978,#26979,#26980,#26981,#26982,#26983,#26984,#26985,#26986,
#26987,#26988,#26989,#26990,#26991,#26992,#26993,#26994,#26995,#26996,#26997,
#26998,#26999,#27000,#27001,#27002,#27003,#27004,#27005,#27006,#27007,#27008,
#27009,#27010,#27011,#27012,#27013,#27014,#27015,#27016,#27017,#27018,#27019,
#27020,#27021,#27022,#27023,#27024,#27025,#27026,#27027,#27028,#27029,#27030,
#27031,#27032,#27033,#27034,#27035,#27036,#27037,#27038,#27039,#27040,#27041,
#27042,#27043,#27044,#27045,#27046,#27047,#27048,#27049,#27050,#27051,#27052,
#27053,#27054,#27055,#27056,#27057,#27058,#27059,#27060,#27061,#27062,#27063,
#27064,#27065,#27066,#27067,#27068,#27069,#27070,#27071,#27072,#27073,#27074,
#27075,#27076,#27077,#27078,#27079,#27080,#27081,#27082,#27083),
 .UNSPECIFIED.,.F.,.F.,(4,3,3,3,3,3,3,3,3,3,3,3,3,3,3,3,3,3,3,3,3,3,3,3,
3,3,3,3,3,3,3,3,3,3,3,3,3,3,3,3,3,3,3,3,3,3,3,3,3,3,3,3,4),(235.619449019235,
235.701911225271,235.784373083011,235.866834599305,235.949295781002,236.031756634953,
236.114217168008,236.196677387014,236.279137298822,236.36159691028,236.444056228236,
236.526515259538,236.608974011035,236.691432489573,236.773890702001,236.856348655165,
236.938806355913,237.021263811091,237.103721027545,237.189733254047,237.273057598471,
237.355524203916,237.437989965157,237.52045490961,237.602919064686,237.685382457795,
237.767845116343,237.850307067736,237.932768339375,238.015228958659,238.097688952986,
238.18014834975,238.262607176345,238.345065460162,238.42752322859,238.509980509015,
238.594113744427,238.676579742518,238.759044118874,238.841506983136,238.923968444927,
239.006428613848,239.088887599483,239.1713455114,239.256941356925,239.339406093525,
239.421867865527,239.50432711137,239.586784269347,239.669246787628,239.751704458483,
239.834163248434,239.856112275599),.UNSPECIFIED.);
#255=B_SPLINE_CURVE_WITH_KNOTS('',3,(#27089,#27090,#27091,#27092,#27093,
#27094,#27095,#27096,#27097,#27098,#27099,#27100,#27101,#27102,#27103,#27104,
#27105,#27106,#27107,#27108,#27109,#27110,#27111,#27112,#27113,#27114,#27115,
#27116,#27117,#27118,#27119,#27120,#27121,#27122,#27123,#27124,#27125,#27126,
#27127,#27128,#27129,#27130,#27131,#27132,#27133,#27134,#27135,#27136,#27137,
#27138,#27139,#27140,#27141,#27142,#27143,#27144,#27145,#27146,#27147,#27148,
#27149,#27150,#27151,#27152,#27153,#27154,#27155,#27156,#27157,#27158,#27159,
#27160,#27161,#27162,#27163,#27164,#27165,#27166,#27167,#27168,#27169,#27170,
#27171,#27172,#27173,#27174,#27175,#27176,#27177,#27178,#27179,#27180,#27181,
#27182,#27183,#27184,#27185,#27186,#27187,#27188,#27189,#27190,#27191,#27192,
#27193,#27194,#27195,#27196,#27197,#27198,#27199,#27200,#27201,#27202,#27203,
#27204,#27205,#27206,#27207,#27208,#27209,#27210,#27211,#27212,#27213,#27214,
#27215,#27216,#27217,#27218,#27219,#27220,#27221,#27222,#27223,#27224,#27225,
#27226,#27227,#27228,#27229,#27230,#27231,#27232,#27233,#27234,#27235,#27236,
#27237,#27238,#27239,#27240,#27241,#27242,#27243,#27244,#27245,#27246,#27247,
#27248,#27249,#27250,#27251,#27252,#27253,#27254),.UNSPECIFIED.,.F.,.F.,
(4,3,3,3,3,3,3,3,3,3,3,3,3,3,3,3,3,3,3,3,3,3,3,3,3,3,3,3,3,3,3,3,3,3,3,
3,3,3,3,3,3,3,3,3,3,3,3,3,3,3,3,3,3,3,3,4),(241.902634326508,241.991481549631,
242.08074815538,242.170566176986,242.243474315059,242.32099144496,242.398421266536,
242.47577943567,242.553081556801,242.630343193839,242.707590133178,242.784831381439,
242.862080992487,242.939353022252,243.016705804237,243.094100041666,243.171608251892,
243.243227926429,243.320052559492,243.396787962553,243.473450383891,243.550056013341,
243.626620995494,243.703666063282,243.780213655939,243.856771342673,243.933353700752,
244.010760660013,244.087475474036,244.165228505917,244.242981537798,244.320557095295,
244.398040041958,244.475446020934,244.552790620198,244.63008938361,244.707365173255,
244.784630219071,244.861898546201,244.93918417898,245.01654240536,245.093937641863,
245.171439269109,245.242735149167,245.324239347918,245.405638509028,245.489881870484,
245.571053821512,245.652148394617,245.733150864216,245.742611954852,245.823593928372,
245.904708754097,245.985890162213,246.067205728831,246.139010671909),
 .UNSPECIFIED.);
#256=B_SPLINE_CURVE_WITH_KNOTS('',3,(#27255,#27256,#27257,#27258,#27259,
#27260,#27261,#27262,#27263,#27264,#27265,#27266,#27267,#27268,#27269,#27270,
#27271,#27272,#27273,#27274,#27275,#27276,#27277,#27278,#27279,#27280,#27281,
#27282,#27283,#27284,#27285,#27286,#27287,#27288,#27289,#27290,#27291,#27292,
#27293,#27294,#27295,#27296,#27297,#27298,#27299,#27300,#27301,#27302,#27303,
#27304,#27305,#27306,#27307,#27308,#27309,#27310,#27311,#27312,#27313,#27314,
#27315,#27316,#27317,#27318,#27319,#27320,#27321,#27322,#27323,#27324,#27325,
#27326,#27327,#27328,#27329,#27330,#27331,#27332,#27333,#27334,#27335,#27336),
 .UNSPECIFIED.,.F.,.F.,(4,3,3,3,3,3,3,3,3,3,3,3,3,3,3,3,3,3,3,3,3,3,3,3,
3,3,3,4),(239.855757872884,239.93307233432,240.01079602382,240.088243427902,
240.166105260111,240.24396709232,240.320816209889,240.397571551698,240.474249387176,
240.550865923322,240.627437318259,240.704472741438,240.78101565417,240.857564483456,
240.934133806003,241.011530530425,241.088222094877,241.165971399284,241.24372070369,
241.3215239023,241.39920307501,241.476809248804,241.554356273541,241.631857962595,
241.709331190126,241.786787502144,241.864252488673,241.902634326415),
 .UNSPECIFIED.);
#257=B_SPLINE_CURVE_WITH_KNOTS('',3,(#27338,#27339,#27340,#27341,#27342,
#27343,#27344,#27345,#27346,#27347,#27348,#27349,#27350,#27351,#27352,#27353,
#27354,#27355,#27356,#27357,#27358,#27359,#27360,#27361,#27362,#27363,#27364,
#27365,#27366,#27367,#27368,#27369,#27370,#27371,#27372,#27373,#27374,#27375,
#27376,#27377,#27378,#27379,#27380,#27381,#27382,#27383,#27384,#27385,#27386,
#27387,#27388,#27389,#27390,#27391,#27392,#27393,#27394,#27395,#27396,#27397,
#27398,#27399,#27400,#27401,#27402,#27403,#27404,#27405,#27406,#27407,#27408,
#27409,#27410,#27411,#27412,#27413),.UNSPECIFIED.,.F.,.F.,(4,3,3,3,3,3,
3,3,3,3,3,3,3,3,3,3,3,3,3,3,3,3,3,3,3,4),(239.856112275599,239.938573879453,
240.021034817424,240.103495116909,240.185954805306,240.268413910008,240.350872458408,
240.433330477894,240.515787995855,240.602465891515,240.684932677351,240.767397790695,
240.8498613412,240.932323438498,241.014784192199,241.097243711896,241.179702107164,
241.262159487561,241.344625873827,241.427089075841,241.509549532122,241.592007681033,
241.674473285912,241.756933165126,241.83939727849,241.902634326415),
 .UNSPECIFIED.);
#258=B_SPLINE_CURVE_WITH_KNOTS('',3,(#27414,#27415,#27416,#27417,#27418,
#27419,#27420,#27421,#27422,#27423,#27424,#27425,#27426,#27427,#27428,#27429,
#27430,#27431,#27432,#27433,#27434,#27435,#27436,#27437,#27438,#27439,#27440,
#27441,#27442,#27443,#27444,#27445,#27446,#27447,#27448,#27449,#27450,#27451,
#27452,#27453,#27454,#27455,#27456,#27457,#27458,#27459,#27460,#27461,#27462,
#27463,#27464,#27465,#27466,#27467,#27468,#27469,#27470,#27471,#27472,#27473,
#27474,#27475,#27476,#27477,#27478,#27479,#27480,#27481,#27482,#27483,#27484,
#27485,#27486,#27487,#27488,#27489,#27490,#27491,#27492,#27493,#27494,#27495,
#27496,#27497,#27498,#27499,#27500,#27501,#27502,#27503,#27504,#27505,#27506,
#27507,#27508,#27509,#27510,#27511,#27512,#27513,#27514,#27515,#27516,#27517,
#27518,#27519,#27520,#27521,#27522,#27523,#27524,#27525,#27526,#27527,#27528,
#27529,#27530,#27531,#27532,#27533,#27534,#27535,#27536,#27537,#27538,#27539,
#27540,#27541,#27542,#27543,#27544,#27545,#27546,#27547,#27548,#27549,#27550,
#27551,#27552,#27553,#27554,#27555,#27556,#27557,#27558,#27559,#27560,#27561,
#27562,#27563,#27564,#27565,#27566,#27567,#27568,#27569,#27570,#27571,#27572,
#27573,#27574,#27575,#27576,#27577,#27578,#27579),.UNSPECIFIED.,.F.,.F.,
(4,3,3,3,3,3,3,3,3,3,3,3,3,3,3,3,3,3,3,3,3,3,3,3,3,3,3,3,3,3,3,3,3,3,3,
3,3,3,3,3,3,3,3,3,3,3,3,3,3,3,3,3,3,3,3,4),(241.902634326415,241.989992668194,
242.077614906619,242.165592798624,242.247282707581,242.324810843968,242.402257701764,
242.479638862983,242.556969862651,242.634266199403,242.711556481288,242.78884637035,
242.866149873463,242.943481002511,243.020900473052,243.098365812055,243.175951178883,
243.245690715632,243.322554508064,243.399324748456,243.476017693521,243.552649537958,
243.629236427911,243.706094214882,243.782652944994,243.859217685687,243.93580300344,
244.012876933501,244.089584152607,244.166841438145,244.244098723683,244.321628306997,
244.399070789021,244.476441811629,244.553756965454,244.63103180076,244.708292081124,
244.785546788089,244.862809963593,244.940095651694,245.017461884113,245.094869643067,
245.172390637053,245.242506731734,245.320041956006,245.397488959025,245.474863386662,
245.552180832619,245.629457522982,245.706713006305,245.78396132947,245.861216532633,
245.938523563794,246.015858858115,246.093274423267,246.138985228352),
 .UNSPECIFIED.);
#259=B_SPLINE_CURVE_WITH_KNOTS('',3,(#27585,#27586,#27587,#27588,#27589,
#27590,#27591,#27592,#27593,#27594,#27595,#27596,#27597,#27598,#27599,#27600,
#27601,#27602,#27603,#27604,#27605,#27606,#27607,#27608,#27609,#27610,#27611,
#27612,#27613,#27614,#27615,#27616,#27617,#27618,#27619,#27620,#27621,#27622,
#27623,#27624,#27625,#27626,#27627,#27628,#27629,#27630,#27631,#27632,#27633,
#27634,#27635,#27636,#27637,#27638,#27639,#27640,#27641,#27642,#27643,#27644,
#27645,#27646,#27647,#27648,#27649,#27650,#27651,#27652,#27653,#27654,#27655,
#27656,#27657,#27658,#27659,#27660,#27661,#27662,#27663,#27664,#27665,#27666,
#27667,#27668,#27669,#27670,#27671,#27672,#27673,#27674,#27675,#27676,#27677,
#27678,#27679,#27680,#27681,#27682,#27683,#27684,#27685,#27686,#27687,#27688,
#27689,#27690,#27691,#27692,#27693,#27694,#27695,#27696,#27697,#27698,#27699,
#27700,#27701,#27702,#27703,#27704,#27705,#27706,#27707,#27708,#27709,#27710,
#27711,#27712,#27713,#27714,#27715,#27716,#27717,#27718,#27719,#27720,#27721,
#27722,#27723,#27724,#27725,#27726,#27727,#27728,#27729,#27730,#27731,#27732,
#27733,#27734,#27735,#27736,#27737,#27738,#27739,#27740,#27741,#27742,#27743,
#27744,#27745,#27746,#27747,#27748,#27749,#27750,#27751,#27752,#27753),
 .UNSPECIFIED.,.F.,.F.,(4,3,3,3,3,3,3,3,3,3,3,3,3,3,3,3,3,3,3,3,3,3,3,3,
3,3,3,3,3,3,3,3,3,3,3,3,3,3,3,3,3,3,3,3,3,3,3,3,3,3,3,3,3,3,3,3,4),(248.185819633594,
248.241995983275,248.319487727223,248.396892528157,248.474226060436,248.551503947157,
248.628741771101,248.705965609896,248.783184193659,248.860411594013,248.937661884912,
249.014993781544,249.092367567984,249.16985625361,249.241749594645,249.3190756192,
249.396313467627,249.47347898075,249.550587946356,249.627656110613,249.704709720991,
249.781757743613,249.858814395049,249.935893894216,250.013055834642,250.090259859986,
250.167580736355,250.241503206014,250.318795771638,250.395999058236,250.473128942955,
250.550201248839,250.627231756401,250.704246300672,250.781254399568,250.858270298374,
250.935308244274,251.012427570257,251.089588337495,251.166865255886,251.241256817383,
251.318543779487,251.395742395434,251.472868538853,251.54993802998,251.626966647179,
251.703980715081,251.780989198166,251.858006341696,251.935046393322,252.012169177978,
252.089334144646,252.16661649259,252.241010428753,252.318356969681,252.395602472991,
252.423061447523),.UNSPECIFIED.);
#260=B_SPLINE_CURVE_WITH_KNOTS('',3,(#27754,#27755,#27756,#27757,#27758,
#27759,#27760,#27761,#27762,#27763,#27764,#27765,#27766,#27767,#27768,#27769,
#27770,#27771,#27772,#27773,#27774,#27775,#27776,#27777,#27778,#27779,#27780,
#27781,#27782,#27783,#27784,#27785,#27786,#27787,#27788,#27789,#27790,#27791,
#27792,#27793,#27794,#27795,#27796,#27797,#27798,#27799,#27800,#27801,#27802,
#27803,#27804,#27805,#27806,#27807,#27808,#27809,#27810,#27811,#27812,#27813,
#27814,#27815,#27816,#27817,#27818,#27819,#27820,#27821,#27822,#27823,#27824,
#27825,#27826,#27827,#27828,#27829,#27830,#27831,#27832,#27833,#27834,#27835,
#27836,#27837,#27838),.UNSPECIFIED.,.F.,.F.,(4,3,3,3,3,3,3,3,3,3,3,3,3,
3,3,3,3,3,3,3,3,3,3,3,3,3,3,3,4),(246.139010671909,246.22049939025,246.242488760537,
246.319972614284,246.39737478087,246.47471088857,246.55199651825,246.629247214064,
246.706491667892,246.783735582781,246.860993005942,246.938277989561,247.015651755802,
247.093071389889,247.17061224538,247.242242371906,247.318525712687,247.394716184162,
247.470830452629,247.54688511173,247.626751926949,247.702745016196,247.778732529846,
247.854729383306,247.930750496942,248.006848406085,248.082991117387,248.159232220467,
248.185819633476),.UNSPECIFIED.);
#261=B_SPLINE_CURVE_WITH_KNOTS('',3,(#27840,#27841,#27842,#27843,#27844,
#27845,#27846,#27847,#27848,#27849,#27850,#27851,#27852,#27853,#27854,#27855,
#27856,#27857,#27858,#27859,#27860,#27861,#27862,#27863,#27864,#27865,#27866,
#27867,#27868,#27869,#27870,#27871,#27872,#27873,#27874,#27875,#27876,#27877,
#27878,#27879,#27880,#27881,#27882,#27883,#27884,#27885,#27886,#27887,#27888,
#27889,#27890,#27891,#27892,#27893,#27894,#27895,#27896,#27897,#27898,#27899,
#27900,#27901,#27902,#27903,#27904,#27905,#27906,#27907,#27908,#27909,#27910,
#27911,#27912,#27913,#27914,#27915,#27916,#27917,#27918,#27919,#27920,#27921,
#27922,#27923,#27924),.UNSPECIFIED.,.F.,.F.,(4,3,3,3,3,3,3,3,3,3,3,3,3,
3,3,3,3,3,3,3,3,3,3,3,3,3,3,3,4),(246.138985228352,246.216525059607,246.240914739785,
246.317753603474,246.394503454466,246.471180528847,246.547801004633,246.624381014889,
246.701248731507,246.777811648328,246.854384750045,246.930982604032,247.008067639983,
247.084797579722,247.162060163779,247.239322747836,247.316388332712,247.393362019337,
247.47025992237,247.547098097972,247.626938289913,247.703711618014,247.780477476615,
247.857250311506,247.934044570009,248.010908994861,248.087815045339,248.164811091715,
248.185819633502),.UNSPECIFIED.);
#262=B_SPLINE_CURVE_WITH_KNOTS('',3,(#27925,#27926,#27927,#27928,#27929,
#27930,#27931,#27932,#27933,#27934,#27935,#27936,#27937,#27938,#27939,#27940,
#27941,#27942,#27943,#27944,#27945,#27946,#27947,#27948,#27949,#27950,#27951,
#27952,#27953,#27954,#27955,#27956,#27957,#27958,#27959,#27960,#27961,#27962,
#27963,#27964,#27965,#27966,#27967,#27968,#27969,#27970,#27971,#27972,#27973,
#27974,#27975,#27976,#27977,#27978,#27979,#27980,#27981,#27982,#27983,#27984,
#27985,#27986,#27987,#27988,#27989,#27990,#27991,#27992,#27993,#27994,#27995,
#27996,#27997,#27998,#27999,#28000,#28001,#28002,#28003,#28004,#28005,#28006,
#28007,#28008,#28009,#28010,#28011,#28012,#28013,#28014,#28015,#28016,#28017,
#28018,#28019,#28020,#28021,#28022,#28023,#28024,#28025,#28026,#28027,#28028,
#28029,#28030,#28031,#28032,#28033,#28034,#28035,#28036,#28037,#28038,#28039,
#28040,#28041,#28042,#28043,#28044,#28045,#28046,#28047,#28048,#28049,#28050,
#28051,#28052,#28053,#28054,#28055,#28056,#28057,#28058,#28059,#28060,#28061,
#28062,#28063,#28064,#28065,#28066,#28067,#28068,#28069,#28070,#28071,#28072,
#28073,#28074,#28075,#28076,#28077,#28078,#28079,#28080,#28081,#28082,#28083,
#28084,#28085,#28086,#28087,#28088,#28089,#28090,#28091,#28092,#28093,#28094,
#28095,#28096),.UNSPECIFIED.,.F.,.F.,(4,3,3,3,3,3,3,3,3,3,3,3,3,3,3,3,3,
3,3,3,3,3,3,3,3,3,3,3,3,3,3,3,3,3,3,3,3,3,3,3,3,3,3,3,3,3,3,3,3,3,3,3,3,
3,3,3,3,4),(248.185819633594,248.237730755887,248.319231491894,248.400627669662,
248.484704442224,248.565874851764,248.646968309605,248.727970345441,248.736934759912,
248.817943698033,248.899028371482,248.983305969596,249.064611849977,249.145995327554,
249.227499291205,249.236138763938,249.313639927106,249.39105963649,249.468413501639,
249.545717084913,249.622985912136,249.700248635407,249.777510938544,249.854786852635,
249.932090413791,250.009482497813,250.08692050769,250.164478904197,250.234546771989,
250.311465957294,250.388291594326,250.465039899041,250.541727026095,250.618369082065,
250.695192294312,250.771805665824,250.848424800283,250.925064228465,251.002036866359,
251.078797104637,251.155875942338,251.23295478004,251.310468016654,251.387894476587,
251.465249812563,251.542549626252,251.619809479155,251.697055364972,251.774296037089,
251.851545548233,251.928817953463,252.006171569364,252.083567057275,252.161076476131,
252.23136278809,252.308745271866,252.386027282496,252.423069114013),
 .UNSPECIFIED.);
#263=B_SPLINE_CURVE_WITH_KNOTS('',3,(#28102,#28103,#28104,#28105,#28106,
#28107,#28108,#28109,#28110,#28111,#28112,#28113,#28114,#28115,#28116,#28117,
#28118,#28119,#28120,#28121,#28122,#28123,#28124,#28125,#28126,#28127,#28128,
#28129,#28130,#28131,#28132,#28133,#28134,#28135,#28136,#28137,#28138,#28139,
#28140,#28141,#28142,#28143,#28144,#28145,#28146,#28147,#28148,#28149,#28150,
#28151,#28152,#28153,#28154,#28155,#28156,#28157,#28158,#28159,#28160,#28161,
#28162,#28163,#28164,#28165,#28166,#28167,#28168,#28169,#28170,#28171,#28172,
#28173,#28174,#28175,#28176,#28177,#28178,#28179,#28180,#28181,#28182,#28183,
#28184,#28185,#28186,#28187,#28188,#28189,#28190,#28191,#28192,#28193,#28194,
#28195,#28196,#28197,#28198,#28199,#28200,#28201,#28202,#28203,#28204,#28205,
#28206,#28207,#28208,#28209,#28210,#28211,#28212,#28213,#28214,#28215,#28216,
#28217,#28218,#28219,#28220,#28221,#28222,#28223,#28224,#28225,#28226,#28227,
#28228,#28229,#28230,#28231,#28232,#28233,#28234,#28235,#28236,#28237,#28238,
#28239,#28240,#28241,#28242,#28243,#28244,#28245,#28246,#28247,#28248,#28249,
#28250,#28251,#28252,#28253,#28254,#28255,#28256,#28257,#28258),
 .UNSPECIFIED.,.F.,.F.,(4,3,3,3,3,3,3,3,3,3,3,3,3,3,3,3,3,3,3,3,3,3,3,3,
3,3,3,3,3,3,3,3,3,3,3,3,3,3,3,3,3,3,3,3,3,3,3,3,3,3,3,3,4),(254.469004940774,
254.55146714681,254.63392900455,254.716390520844,254.798851702541,254.881312556492,
254.963773089547,255.046233308553,255.128693220361,255.211152831819,255.293612149775,
255.376071181077,255.458529932574,255.540988411113,255.623446623541,255.705904576705,
255.788362277453,255.87081973263,255.953276949085,256.039289175586,256.12261352001,
256.205080125455,256.287545886697,256.370010831149,256.452474986225,256.534938379334,
256.617401037883,256.699862989275,256.782324260914,256.864784880198,256.947244874525,
257.02970427129,257.112163097885,257.194621381701,257.277079150129,257.359536430554,
257.443669665966,257.526135664057,257.608600040413,257.691062904675,257.773524366466,
257.855984535387,257.938443521023,258.02090143294,258.106497278465,258.188962015065,
258.271423787067,258.353883032909,258.436340190886,258.518802709167,258.601260380022,
258.683719169973,258.705668197138),.UNSPECIFIED.);
#264=B_SPLINE_CURVE_WITH_KNOTS('',3,(#28259,#28260,#28261,#28262,#28263,
#28264,#28265,#28266,#28267,#28268,#28269,#28270,#28271,#28272,#28273,#28274,
#28275,#28276,#28277,#28278,#28279,#28280,#28281,#28282,#28283,#28284,#28285,
#28286,#28287,#28288,#28289,#28290,#28291,#28292,#28293,#28294,#28295,#28296,
#28297,#28298,#28299,#28300,#28301,#28302,#28303,#28304,#28305,#28306,#28307,
#28308,#28309,#28310,#28311,#28312,#28313,#28314,#28315,#28316,#28317,#28318,
#28319,#28320,#28321,#28322,#28323,#28324,#28325,#28326,#28327,#28328,#28329,
#28330,#28331,#28332,#28333,#28334,#28335,#28336,#28337,#28338,#28339,#28340),
 .UNSPECIFIED.,.F.,.F.,(4,3,3,3,3,3,3,3,3,3,3,3,3,3,3,3,3,3,3,3,3,3,3,3,
3,3,3,4),(252.423061447523,252.500207989694,252.577302788264,252.654361578884,
252.731411716478,252.808460577922,252.885522379586,252.962611342577,253.039783546726,
253.117001743405,253.194328265335,253.240764040122,253.318261963832,253.395671913165,
253.47300956625,253.550290549208,253.62753044714,253.704754798586,253.781972943272,
253.859198952847,253.936446900755,254.013774962946,254.0911440958,254.168626777181,
254.240517651492,254.344578896921,254.445902077886,254.469004940774),
 .UNSPECIFIED.);
#265=B_SPLINE_CURVE_WITH_KNOTS('',3,(#28342,#28343,#28344,#28345,#28346,
#28347,#28348,#28349,#28350,#28351,#28352,#28353,#28354,#28355,#28356,#28357,
#28358,#28359,#28360,#28361,#28362,#28363,#28364,#28365,#28366,#28367,#28368,
#28369,#28370,#28371,#28372,#28373,#28374,#28375,#28376,#28377,#28378,#28379,
#28380,#28381,#28382,#28383,#28384,#28385,#28386,#28387,#28388,#28389,#28390,
#28391,#28392,#28393,#28394,#28395,#28396,#28397,#28398,#28399,#28400,#28401,
#28402,#28403,#28404,#28405,#28406,#28407,#28408,#28409,#28410,#28411,#28412,
#28413,#28414,#28415,#28416,#28417,#28418,#28419,#28420,#28421,#28422,#28423),
 .UNSPECIFIED.,.F.,.F.,(4,3,3,3,3,3,3,3,3,3,3,3,3,3,3,3,3,3,3,3,3,3,3,3,
3,3,3,4),(252.423069114013,252.500249935134,252.57738204784,252.654481140577,
252.731575367837,252.808670952456,252.885782074225,252.962922919092,253.040148347162,
253.117421991369,253.1948013524,253.229770796141,253.306987152008,253.384114373385,
253.46116840088,253.538165120588,253.615120375872,253.69206034023,253.768994302006,
253.845936563417,253.922901428936,253.999948640481,254.077037871748,254.154244171017,
254.228178804192,254.331935348037,254.433147614106,254.469004940774),
 .UNSPECIFIED.);
#266=B_SPLINE_CURVE_WITH_KNOTS('',3,(#28424,#28425,#28426,#28427,#28428,
#28429,#28430,#28431,#28432,#28433,#28434,#28435,#28436,#28437,#28438,#28439,
#28440,#28441,#28442,#28443,#28444,#28445,#28446,#28447,#28448,#28449,#28450,
#28451,#28452,#28453,#28454,#28455,#28456,#28457,#28458,#28459,#28460,#28461,
#28462,#28463,#28464,#28465,#28466,#28467,#28468,#28469,#28470,#28471,#28472,
#28473,#28474,#28475,#28476,#28477,#28478,#28479,#28480,#28481,#28482,#28483,
#28484,#28485,#28486,#28487,#28488,#28489,#28490,#28491,#28492,#28493,#28494,
#28495,#28496,#28497,#28498,#28499,#28500,#28501,#28502,#28503,#28504,#28505,
#28506,#28507,#28508,#28509,#28510,#28511,#28512,#28513,#28514,#28515,#28516,
#28517,#28518,#28519,#28520,#28521,#28522,#28523,#28524,#28525,#28526,#28527,
#28528,#28529,#28530,#28531,#28532,#28533,#28534,#28535,#28536,#28537,#28538,
#28539,#28540,#28541,#28542,#28543,#28544,#28545,#28546,#28547,#28548,#28549,
#28550,#28551,#28552,#28553,#28554,#28555,#28556,#28557,#28558,#28559,#28560,
#28561,#28562,#28563,#28564,#28565,#28566,#28567,#28568,#28569,#28570,#28571,
#28572,#28573,#28574,#28575,#28576,#28577,#28578,#28579,#28580),
 .UNSPECIFIED.,.F.,.F.,(4,3,3,3,3,3,3,3,3,3,3,3,3,3,3,3,3,3,3,3,3,3,3,3,
3,3,3,3,3,3,3,3,3,3,3,3,3,3,3,3,3,3,3,3,3,3,3,3,3,3,3,3,4),(254.469004940774,
254.55146714681,254.63392900455,254.716390520844,254.798851702541,254.881312556492,
254.963773089547,255.046233308553,255.128693220361,255.211152831819,255.293612149775,
255.376071181077,255.458529932574,255.540988411112,255.62344662354,255.705904576704,
255.788362277452,255.87081973263,255.953276949084,256.039289175586,256.122613520009,
256.205080125455,256.287545886696,256.370010831148,256.452474986224,256.534938379333,
256.617401037882,256.699862989275,256.782324260913,256.864784880198,256.947244874524,
257.029704271289,257.112163097884,257.194621381701,257.277079150128,257.359536430553,
257.443669665965,257.526135664057,257.608600040412,257.691062904674,257.773524366465,
257.855984535386,257.938443521022,258.020901432939,258.106497278464,258.188962015064,
258.271423787066,258.353883032908,258.436340190885,258.518802709166,258.601260380021,
258.683719169972,258.705668197138),.UNSPECIFIED.);
#267=B_SPLINE_CURVE_WITH_KNOTS('',3,(#28586,#28587,#28588,#28589,#28590,
#28591,#28592,#28593,#28594,#28595,#28596,#28597,#28598,#28599,#28600,#28601,
#28602,#28603,#28604,#28605,#28606,#28607,#28608,#28609,#28610,#28611,#28612,
#28613,#28614,#28615,#28616,#28617,#28618,#28619,#28620,#28621,#28622,#28623,
#28624,#28625,#28626,#28627,#28628,#28629,#28630,#28631,#28632,#28633,#28634,
#28635,#28636,#28637,#28638,#28639,#28640,#28641,#28642,#28643,#28644,#28645,
#28646,#28647,#28648,#28649,#28650,#28651,#28652,#28653,#28654,#28655,#28656,
#28657,#28658,#28659,#28660,#28661,#28662,#28663,#28664,#28665,#28666,#28667,
#28668,#28669,#28670,#28671,#28672,#28673,#28674,#28675,#28676,#28677,#28678,
#28679,#28680,#28681,#28682,#28683,#28684,#28685,#28686,#28687,#28688,#28689,
#28690,#28691,#28692,#28693,#28694,#28695,#28696,#28697,#28698,#28699,#28700,
#28701,#28702,#28703,#28704,#28705,#28706,#28707,#28708,#28709,#28710,#28711,
#28712,#28713,#28714,#28715,#28716,#28717,#28718,#28719,#28720,#28721,#28722,
#28723,#28724,#28725,#28726,#28727,#28728,#28729,#28730,#28731,#28732,#28733,
#28734,#28735,#28736,#28737,#28738,#28739,#28740,#28741,#28742,#28743,#28744,
#28745,#28746,#28747,#28748,#28749,#28750,#28751,#28752,#28753,#28754),
 .UNSPECIFIED.,.F.,.F.,(4,3,3,3,3,3,3,3,3,3,3,3,3,3,3,3,3,3,3,3,3,3,3,3,
3,3,3,3,3,3,3,3,3,3,3,3,3,3,3,3,3,3,3,3,3,3,3,3,3,3,3,3,3,3,3,3,4),(260.752190247954,
260.833924659858,260.915784801191,260.997857630573,261.080038110251,261.162414601535,
261.238792931077,261.315614602842,261.392347043997,261.469006505033,261.54560917796,
261.622171209519,261.699218126134,261.775762796189,261.852317573389,261.928897036949,
262.006309413323,262.083021391968,262.160783967207,262.238546542446,262.316129158385,
262.393619133169,262.471032103223,262.548383649812,262.625689310076,262.702971896898,
262.780243677878,262.857518672036,262.934810897546,263.012175564937,263.089577168637,
263.167084978965,263.238300153816,263.319783597925,263.401162433877,263.485416065282,
263.566569041431,263.64764520618,263.728630130979,263.7381769595,263.819185708317,
263.900270329473,263.984716188401,264.066022655456,264.147406836517,264.228911894201,
264.238053765185,264.315582157019,264.393026319221,264.470388847433,264.547704869653,
264.624988440364,264.702253593051,264.779533264968,264.856819399072,264.934155284713,
264.988317180418),.UNSPECIFIED.);
#268=B_SPLINE_CURVE_WITH_KNOTS('',3,(#28755,#28756,#28757,#28758,#28759,
#28760,#28761,#28762,#28763,#28764,#28765,#28766,#28767,#28768,#28769,#28770,
#28771,#28772,#28773,#28774,#28775,#28776,#28777,#28778,#28779,#28780,#28781,
#28782,#28783,#28784,#28785,#28786,#28787,#28788,#28789,#28790,#28791,#28792,
#28793,#28794,#28795,#28796,#28797,#28798,#28799,#28800,#28801,#28802,#28803,
#28804,#28805,#28806,#28807,#28808,#28809,#28810,#28811,#28812,#28813,#28814,
#28815,#28816,#28817,#28818,#28819,#28820,#28821,#28822,#28823,#28824,#28825,
#28826,#28827,#28828,#28829,#28830),.UNSPECIFIED.,.F.,.F.,(4,3,3,3,3,3,
3,3,3,3,3,3,3,3,3,3,3,3,3,3,3,3,3,3,3,4),(258.705668197138,258.788129800992,
258.870590738963,258.953051038448,259.035510726845,259.117969831547,259.200428379947,
259.282886399433,259.365343917394,259.452021813054,259.53448859889,259.616953712234,
259.699417262739,259.781879360037,259.864340113738,259.946799633435,260.029258028703,
260.1117154091,260.194181795366,260.27664499738,260.359105453661,260.441563602571,
260.524029207451,260.606489086665,260.688953200029,260.752190247954),
 .UNSPECIFIED.);
#269=B_SPLINE_CURVE_WITH_KNOTS('',3,(#28832,#28833,#28834,#28835,#28836,
#28837,#28838,#28839,#28840,#28841,#28842,#28843,#28844,#28845,#28846,#28847,
#28848,#28849,#28850,#28851,#28852,#28853,#28854,#28855,#28856,#28857,#28858,
#28859,#28860,#28861,#28862,#28863,#28864,#28865,#28866,#28867,#28868,#28869,
#28870,#28871,#28872,#28873,#28874,#28875,#28876,#28877,#28878,#28879,#28880,
#28881,#28882,#28883,#28884,#28885,#28886,#28887,#28888,#28889,#28890,#28891,
#28892,#28893,#28894,#28895,#28896,#28897,#28898,#28899,#28900,#28901,#28902,
#28903,#28904,#28905,#28906,#28907),.UNSPECIFIED.,.F.,.F.,(4,3,3,3,3,3,
3,3,3,3,3,3,3,3,3,3,3,3,3,3,3,3,3,3,3,4),(258.705668197138,258.788129800991,
258.870590738962,258.953051038448,259.035510726845,259.117969831547,259.200428379946,
259.282886399432,259.365343917394,259.452021813054,259.534488598889,259.616953712233,
259.699417262738,259.781879360036,259.864340113737,259.946799633435,260.029258028702,
260.111715409099,260.194181795366,260.276644997379,260.35910545366,260.441563602571,
260.52402920745,260.606489086665,260.688953200028,260.752190247953),
 .UNSPECIFIED.);
#270=B_SPLINE_CURVE_WITH_KNOTS('',3,(#28908,#28909,#28910,#28911,#28912,
#28913,#28914,#28915,#28916,#28917,#28918,#28919,#28920,#28921,#28922,#28923,
#28924,#28925,#28926,#28927,#28928,#28929,#28930,#28931,#28932,#28933,#28934,
#28935,#28936,#28937,#28938,#28939,#28940,#28941,#28942,#28943,#28944,#28945,
#28946,#28947,#28948,#28949,#28950,#28951,#28952,#28953,#28954,#28955,#28956,
#28957,#28958,#28959,#28960,#28961,#28962,#28963,#28964,#28965,#28966,#28967,
#28968,#28969,#28970,#28971,#28972,#28973,#28974,#28975,#28976,#28977,#28978,
#28979,#28980,#28981,#28982,#28983,#28984,#28985,#28986,#28987,#28988,#28989,
#28990,#28991,#28992,#28993,#28994,#28995,#28996,#28997,#28998,#28999,#29000,
#29001,#29002,#29003,#29004,#29005,#29006,#29007,#29008,#29009,#29010,#29011,
#29012,#29013,#29014,#29015,#29016,#29017,#29018,#29019,#29020,#29021,#29022,
#29023,#29024,#29025,#29026,#29027,#29028,#29029,#29030,#29031,#29032,#29033,
#29034,#29035,#29036,#29037,#29038,#29039,#29040,#29041,#29042,#29043,#29044,
#29045,#29046,#29047,#29048,#29049,#29050,#29051,#29052,#29053,#29054,#29055,
#29056,#29057,#29058,#29059,#29060,#29061,#29062,#29063,#29064,#29065,#29066,
#29067,#29068,#29069,#29070,#29071,#29072,#29073),.UNSPECIFIED.,.F.,.F.,
(4,3,3,3,3,3,3,3,3,3,3,3,3,3,3,3,3,3,3,3,3,3,3,3,3,3,3,3,3,3,3,3,3,3,3,
3,3,3,3,3,3,3,3,3,3,3,3,3,3,3,3,3,3,3,3,4),(260.752190247953,260.833508676024,
260.914959009631,260.996629128698,261.07841550255,261.160402427617,261.217034860549,
261.294564756422,261.372007551726,261.449378888063,261.526694355795,261.603969504918,
261.681230098028,261.758485117062,261.835748603716,261.913034601805,261.990401140851,
262.067809205046,262.145330499162,262.2154428686,262.29297242758,262.370414889339,
262.447785895736,262.525101037391,262.60237586456,262.679636142938,262.756890851673,
262.834154032701,262.911439730082,262.988805977652,263.066213754988,263.14373477266,
263.213850876651,263.290687299622,263.367434709828,263.444109345184,263.520727385502,
263.59730496563,263.674174205513,263.750734716384,263.827305423362,263.903900895436,
263.980990392753,264.057718000293,264.134988442497,264.212258884701,264.289866799726,
264.367379857018,264.444995213602,264.522354264186,264.599671172362,264.676959973276,
264.754795657381,264.832085034435,264.910193872066,264.988302709697),
 .UNSPECIFIED.);
#271=B_SPLINE_CURVE_WITH_KNOTS('',3,(#29079,#29080,#29081,#29082,#29083,
#29084,#29085,#29086,#29087,#29088,#29089,#29090,#29091,#29092,#29093,#29094,
#29095,#29096,#29097,#29098,#29099,#29100,#29101,#29102,#29103,#29104,#29105,
#29106,#29107,#29108,#29109,#29110,#29111,#29112,#29113,#29114,#29115,#29116,
#29117,#29118,#29119,#29120,#29121,#29122,#29123,#29124,#29125,#29126,#29127,
#29128,#29129,#29130,#29131,#29132,#29133,#29134,#29135,#29136,#29137,#29138,
#29139,#29140,#29141,#29142,#29143,#29144,#29145,#29146,#29147,#29148,#29149,
#29150,#29151,#29152,#29153,#29154,#29155,#29156,#29157,#29158,#29159,#29160,
#29161,#29162,#29163,#29164,#29165,#29166,#29167,#29168,#29169,#29170,#29171,
#29172,#29173,#29174,#29175,#29176,#29177,#29178,#29179,#29180,#29181,#29182,
#29183,#29184,#29185,#29186,#29187,#29188,#29189,#29190,#29191,#29192,#29193,
#29194,#29195,#29196,#29197,#29198,#29199,#29200,#29201,#29202,#29203,#29204,
#29205,#29206,#29207,#29208,#29209,#29210,#29211,#29212,#29213,#29214,#29215,
#29216,#29217,#29218,#29219,#29220,#29221,#29222,#29223,#29224,#29225,#29226,
#29227,#29228,#29229,#29230,#29231,#29232,#29233,#29234,#29235,#29236,#29237,
#29238,#29239,#29240,#29241,#29242,#29243,#29244,#29245,#29246,#29247),
 .UNSPECIFIED.,.F.,.F.,(4,3,3,3,3,3,3,3,3,3,3,3,3,3,3,3,3,3,3,3,3,3,3,3,
3,3,3,3,3,3,3,3,3,3,3,3,3,3,3,3,3,3,3,3,3,3,3,3,3,3,3,3,3,3,3,3,4),(267.035375555133,
267.144452834569,267.237314599293,267.314831961683,267.392262022246,267.469620436555,
267.546922808741,267.624184702416,267.701431905952,267.778673422974,267.855923307091,
267.933195613976,268.010548677938,268.087943200411,268.16545169814,268.237068210663,
268.313889409591,268.390621373587,268.467280353525,268.543882541783,268.620444085465,
268.697491302536,268.774035478986,268.850589760838,268.927168727623,269.004582001225,
269.081293483321,269.159057652676,269.236821822032,269.31440444721,269.391894430998,
269.469307409814,269.546658964918,269.623964633442,269.701247228109,269.77851901668,
269.855794018169,269.933086250741,270.010450924736,270.087852534799,270.165360351022,
270.236575433401,270.318059401026,270.399438759856,270.483692129663,270.564845619648,
270.64592229249,270.726907715281,270.736452239086,270.817460637931,270.89854489779,
270.982990934535,271.064297019422,271.145680812412,271.227185476696,271.236329044771,
271.272326787262),.UNSPECIFIED.);
#272=B_SPLINE_CURVE_WITH_KNOTS('',3,(#29248,#29249,#29250,#29251,#29252,
#29253,#29254,#29255,#29256,#29257,#29258,#29259,#29260,#29261,#29262,#29263,
#29264,#29265,#29266,#29267,#29268,#29269,#29270,#29271,#29272,#29273,#29274,
#29275,#29276,#29277,#29278,#29279,#29280,#29281,#29282,#29283,#29284,#29285,
#29286,#29287,#29288,#29289,#29290,#29291,#29292,#29293,#29294,#29295,#29296,
#29297,#29298,#29299,#29300,#29301,#29302,#29303,#29304,#29305,#29306,#29307,
#29308,#29309,#29310,#29311,#29312,#29313,#29314,#29315,#29316,#29317,#29318,
#29319,#29320,#29321,#29322,#29323,#29324,#29325,#29326,#29327,#29328,#29329,
#29330,#29331,#29332),.UNSPECIFIED.,.F.,.F.,(4,3,3,3,3,3,3,3,3,3,3,3,3,
3,3,3,3,3,3,3,3,3,3,3,3,3,3,3,4),(264.988317180418,265.065754055233,265.143245580455,
265.220842788067,265.237807376555,265.31465601182,265.391410870359,265.468088221961,
265.544704273979,265.621275184883,265.698310910263,265.774853341281,265.851401690157,
265.92797053391,266.005368147414,266.082059240563,266.159810114243,266.237560987924,
266.314064343492,266.390479740073,266.46682368928,266.543107292491,266.619357978181,
266.695590567042,266.771819865679,266.848086066066,266.924373142649,267.000726718474,
267.035375555007),.UNSPECIFIED.);
#273=B_SPLINE_CURVE_WITH_KNOTS('',3,(#29334,#29335,#29336,#29337,#29338,
#29339,#29340,#29341,#29342,#29343,#29344,#29345,#29346,#29347,#29348,#29349,
#29350,#29351,#29352,#29353,#29354,#29355,#29356,#29357,#29358,#29359,#29360,
#29361,#29362,#29363,#29364,#29365,#29366,#29367,#29368,#29369,#29370,#29371,
#29372,#29373,#29374,#29375,#29376,#29377,#29378,#29379,#29380,#29381,#29382,
#29383,#29384,#29385,#29386,#29387,#29388,#29389,#29390,#29391,#29392,#29393,
#29394,#29395,#29396,#29397,#29398,#29399,#29400,#29401,#29402,#29403,#29404,
#29405,#29406,#29407,#29408,#29409,#29410,#29411,#29412,#29413,#29414,#29415,
#29416,#29417,#29418),.UNSPECIFIED.,.F.,.F.,(4,3,3,3,3,3,3,3,3,3,3,3,3,
3,3,3,3,3,3,3,3,3,3,3,3,3,3,3,4),(264.988302709697,265.065719049362,265.143240355639,
265.210666892752,265.292152799803,265.373534475164,265.457618580567,265.53877549918,
265.619855887071,265.700845490964,265.709870896778,265.790884280144,265.871973260509,
265.956248670583,266.037558439693,266.118945648338,266.200453098809,266.209074900803,
266.285179233415,266.361201935431,266.437159715668,266.513068483997,266.588951011644,
266.664822302395,266.740697350382,266.816626102046,266.892581841232,266.968628479594,
267.034597505135),.UNSPECIFIED.);
#274=B_SPLINE_CURVE_WITH_KNOTS('',3,(#29419,#29420,#29421,#29422,#29423,
#29424,#29425,#29426,#29427,#29428,#29429,#29430,#29431,#29432,#29433,#29434,
#29435,#29436,#29437,#29438,#29439,#29440,#29441,#29442,#29443,#29444,#29445,
#29446,#29447,#29448,#29449,#29450,#29451,#29452,#29453,#29454,#29455,#29456,
#29457,#29458,#29459,#29460,#29461,#29462,#29463,#29464,#29465,#29466,#29467,
#29468,#29469,#29470,#29471,#29472,#29473,#29474,#29475,#29476,#29477,#29478,
#29479,#29480,#29481,#29482,#29483,#29484,#29485,#29486,#29487,#29488,#29489,
#29490,#29491,#29492,#29493,#29494,#29495,#29496,#29497,#29498,#29499,#29500,
#29501,#29502,#29503,#29504,#29505,#29506,#29507,#29508,#29509,#29510,#29511,
#29512,#29513,#29514,#29515,#29516,#29517,#29518,#29519,#29520,#29521,#29522,
#29523,#29524,#29525,#29526,#29527,#29528,#29529,#29530,#29531,#29532,#29533,
#29534,#29535,#29536,#29537,#29538,#29539,#29540,#29541,#29542,#29543,#29544,
#29545,#29546,#29547,#29548,#29549,#29550,#29551,#29552,#29553,#29554,#29555,
#29556,#29557,#29558,#29559,#29560,#29561,#29562,#29563,#29564,#29565,#29566,
#29567,#29568,#29569,#29570,#29571,#29572,#29573,#29574,#29575),
 .UNSPECIFIED.,.F.,.F.,(4,3,3,3,3,3,3,3,3,3,3,3,3,3,3,3,3,3,3,3,3,3,3,3,
3,3,3,3,3,3,3,3,3,3,3,3,3,3,3,3,3,3,3,3,3,3,3,3,3,3,3,3,4),(267.035375555133,
267.117837761169,267.200299618909,267.282761135203,267.3652223169,267.447683170851,
267.530143703906,267.612603922912,267.69506383472,267.777523446178,267.859982764134,
267.942441795436,268.024900546933,268.107359025471,268.189817237899,268.272275191063,
268.354732891811,268.437190346989,268.519647563443,268.605659789945,268.688984134369,
268.771450739814,268.853916501055,268.936381445508,269.018845600584,269.101308993693,
269.183771652241,269.266233603634,269.348694875273,269.431155494557,269.513615488884,
269.596074885648,269.678533712244,269.76099199606,269.843449764488,269.925907044913,
270.010040280324,270.092506278416,270.174970654772,270.257433519034,270.339894980824,
270.422355149746,270.504814135381,270.587272047298,270.672867892823,270.755332629423,
270.837794401425,270.920253647267,271.002710805245,271.085173323526,271.167630994381,
271.250089784331,271.272038811497),.UNSPECIFIED.);
#275=B_SPLINE_CURVE_WITH_KNOTS('',3,(#29581,#29582,#29583,#29584,#29585,
#29586,#29587,#29588,#29589,#29590,#29591,#29592,#29593,#29594,#29595,#29596,
#29597,#29598,#29599,#29600,#29601,#29602,#29603,#29604,#29605,#29606,#29607,
#29608,#29609,#29610,#29611,#29612,#29613,#29614,#29615,#29616,#29617,#29618,
#29619,#29620,#29621,#29622,#29623,#29624,#29625,#29626,#29627,#29628,#29629,
#29630,#29631,#29632,#29633,#29634,#29635,#29636,#29637,#29638,#29639,#29640,
#29641,#29642,#29643,#29644,#29645,#29646,#29647,#29648,#29649,#29650,#29651,
#29652,#29653,#29654,#29655,#29656,#29657,#29658,#29659,#29660,#29661,#29662,
#29663,#29664,#29665,#29666,#29667,#29668,#29669,#29670,#29671,#29672,#29673,
#29674,#29675,#29676,#29677,#29678,#29679,#29680,#29681,#29682,#29683,#29684,
#29685,#29686,#29687,#29688,#29689,#29690,#29691,#29692,#29693,#29694,#29695,
#29696,#29697,#29698,#29699,#29700,#29701,#29702,#29703,#29704,#29705,#29706,
#29707,#29708,#29709,#29710,#29711,#29712,#29713,#29714,#29715,#29716,#29717,
#29718,#29719,#29720,#29721,#29722,#29723,#29724,#29725,#29726,#29727,#29728,
#29729,#29730,#29731,#29732,#29733,#29734,#29735,#29736,#29737,#29738,#29739,
#29740,#29741,#29742,#29743,#29744,#29745,#29746),.UNSPECIFIED.,.F.,.F.,
(4,3,3,3,3,3,3,3,3,3,3,3,3,3,3,3,3,3,3,3,3,3,3,3,3,3,3,3,3,3,3,3,3,3,3,
3,3,3,3,3,3,3,3,3,3,3,3,3,3,3,3,3,3,3,3,4),(273.318560862452,273.395142880457,
273.471642911441,273.548077363806,273.624462590287,273.700853501361,273.777200930976,
273.853550909225,273.929918174114,274.006361413199,274.082842797132,274.15943777032,
274.235589878879,274.313107248038,274.390537315452,274.467895736685,274.545198115862,
274.622460016587,274.69970722724,274.77694875142,274.854198642728,274.931470956833,
275.008824028021,275.086218557734,275.163727062659,275.235343490248,275.312164687398,
275.388896649607,275.465555627749,275.542157814205,275.61871935608,275.695766574272,
275.77231074891,275.84886502895,275.925443993923,276.002857270847,276.079568751148,
276.157332926383,276.235097101618,276.31267972525,276.390169707476,276.467582684719,
276.544934238238,276.622239905168,276.699522498231,276.776794285192,276.854069285067,
276.931361516023,277.008726188406,277.086127796857,277.163635611483,277.234850712987,
277.316315177658,277.397686217241,277.478930272538,277.55569081987),
 .UNSPECIFIED.);
#276=B_SPLINE_CURVE_WITH_KNOTS('',3,(#29747,#29748,#29749,#29750,#29751,
#29752,#29753,#29754,#29755,#29756,#29757,#29758,#29759,#29760,#29761,#29762,
#29763,#29764,#29765,#29766,#29767,#29768,#29769,#29770,#29771,#29772,#29773,
#29774,#29775,#29776,#29777,#29778,#29779,#29780,#29781,#29782,#29783,#29784,
#29785,#29786,#29787,#29788,#29789,#29790,#29791,#29792,#29793,#29794,#29795,
#29796,#29797,#29798,#29799,#29800,#29801,#29802,#29803,#29804,#29805,#29806,
#29807,#29808,#29809,#29810,#29811,#29812,#29813,#29814,#29815,#29816,#29817,
#29818,#29819,#29820,#29821,#29822,#29823,#29824,#29825,#29826,#29827,#29828),
 .UNSPECIFIED.,.F.,.F.,(4,3,3,3,3,3,3,3,3,3,3,3,3,3,3,3,3,3,3,3,3,3,3,3,
3,3,3,4),(271.272326787262,271.349802796202,271.427204574214,271.504547693917,
271.581847685763,271.659120048451,271.736395155182,271.813676265128,271.890977398363,
271.968312583541,272.045738465872,272.123216012992,272.200804181388,272.23608265614,
272.31293127929,272.389686125647,272.466363465012,272.542979504746,272.619550403329,
272.696586136352,272.773128555014,272.849676891532,272.926245722935,273.003643359079,
273.080334439985,273.158085353747,273.23583626751,273.318560862313),
 .UNSPECIFIED.);
#277=B_SPLINE_CURVE_WITH_KNOTS('',3,(#29830,#29831,#29832,#29833,#29834,
#29835,#29836,#29837,#29838,#29839,#29840,#29841,#29842,#29843,#29844,#29845,
#29846,#29847,#29848,#29849,#29850,#29851,#29852,#29853,#29854,#29855,#29856,
#29857,#29858,#29859,#29860,#29861,#29862,#29863,#29864,#29865,#29866,#29867,
#29868,#29869,#29870,#29871,#29872,#29873,#29874,#29875,#29876,#29877,#29878,
#29879,#29880,#29881,#29882,#29883,#29884,#29885,#29886,#29887,#29888,#29889,
#29890,#29891,#29892,#29893,#29894,#29895,#29896,#29897,#29898,#29899,#29900,
#29901,#29902,#29903,#29904,#29905),.UNSPECIFIED.,.F.,.F.,(4,3,3,3,3,3,
3,3,3,3,3,3,3,3,3,3,3,3,3,3,3,3,3,3,3,4),(271.272038811497,271.354500415351,
271.436961353322,271.519421652807,271.601881341204,271.684340445906,271.766798994306,
271.849257013792,271.931714531753,272.018392427413,272.100859213249,272.183324326593,
272.265787877098,272.348249974396,272.430710728097,272.513170247794,272.595628643062,
272.678086023459,272.760552409725,272.843015611739,272.92547606802,273.007934216931,
273.09039982181,273.172859701024,273.255323814388,273.318560862313),
 .UNSPECIFIED.);
#278=B_SPLINE_CURVE_WITH_KNOTS('',3,(#29906,#29907,#29908,#29909,#29910,
#29911,#29912,#29913,#29914,#29915,#29916,#29917,#29918,#29919,#29920,#29921,
#29922,#29923,#29924,#29925,#29926,#29927,#29928,#29929,#29930,#29931,#29932,
#29933,#29934,#29935,#29936,#29937,#29938,#29939,#29940,#29941,#29942,#29943,
#29944,#29945,#29946,#29947,#29948,#29949,#29950,#29951,#29952,#29953,#29954,
#29955,#29956,#29957,#29958,#29959,#29960,#29961,#29962,#29963,#29964,#29965,
#29966,#29967,#29968,#29969,#29970,#29971,#29972,#29973,#29974,#29975,#29976,
#29977,#29978,#29979,#29980,#29981,#29982,#29983,#29984,#29985,#29986,#29987,
#29988,#29989,#29990,#29991,#29992,#29993,#29994,#29995,#29996,#29997,#29998,
#29999,#30000,#30001,#30002,#30003,#30004,#30005,#30006,#30007,#30008,#30009,
#30010,#30011,#30012,#30013,#30014,#30015,#30016,#30017,#30018,#30019,#30020,
#30021,#30022,#30023,#30024,#30025,#30026,#30027,#30028,#30029,#30030,#30031,
#30032,#30033,#30034,#30035,#30036,#30037,#30038,#30039,#30040,#30041,#30042,
#30043,#30044,#30045,#30046,#30047,#30048,#30049,#30050,#30051,#30052,#30053,
#30054,#30055,#30056,#30057,#30058,#30059,#30060,#30061,#30062,#30063,#30064,
#30065,#30066,#30067,#30068,#30069,#30070,#30071,#30072,#30073,#30074),
 .UNSPECIFIED.,.F.,.F.,(4,3,3,3,3,3,3,3,3,3,3,3,3,3,3,3,3,3,3,3,3,3,3,3,
3,3,3,3,3,3,3,3,3,3,3,3,3,3,3,3,3,3,3,3,3,3,3,3,3,3,3,3,3,3,3,3,4),(273.319207559223,
273.395811164144,273.472346602566,273.548830171782,273.62527812616,273.701718887028,
273.778159754071,273.854615409225,273.931100541588,274.007671395534,274.084291096307,
274.161018943372,274.196338965211,274.273202349841,274.349972181628,274.426664717593,
274.503296152736,274.579882633495,274.656740675966,274.733298998903,274.809863333548,
274.886448246649,274.963522928302,275.040229749143,275.117488361202,275.194746973262,
275.272277169792,275.349720264468,275.427091898596,275.504407662237,275.581683105089,
275.658943987583,275.736199293302,275.813463063672,275.890749342232,275.9681161551,
276.045524489883,276.123046046522,276.193154981312,276.270685099344,276.348128128628,
276.425499710421,276.502815434749,276.580090851278,276.657351727271,276.734607038584,
276.811870826643,276.889157134995,276.966523996568,277.043932390467,277.121454023307,
277.191562989363,277.268414568166,277.345153547054,277.421827869475,277.498442284338,
277.555563663649),.UNSPECIFIED.);
#279=B_SPLINE_CURVE_WITH_KNOTS('',3,(#30080,#30081,#30082,#30083,#30084,
#30085,#30086,#30087,#30088,#30089,#30090,#30091,#30092,#30093,#30094,#30095,
#30096,#30097,#30098,#30099,#30100,#30101,#30102,#30103,#30104,#30105,#30106,
#30107,#30108,#30109,#30110,#30111,#30112,#30113,#30114,#30115,#30116,#30117,
#30118,#30119,#30120,#30121,#30122,#30123,#30124,#30125,#30126,#30127,#30128,
#30129,#30130,#30131,#30132,#30133,#30134,#30135,#30136,#30137,#30138,#30139,
#30140,#30141,#30142,#30143,#30144,#30145,#30146,#30147,#30148,#30149,#30150,
#30151,#30152,#30153,#30154,#30155,#30156,#30157,#30158,#30159,#30160,#30161,
#30162,#30163,#30164,#30165,#30166,#30167,#30168,#30169,#30170,#30171,#30172,
#30173,#30174,#30175,#30176,#30177,#30178,#30179,#30180,#30181,#30182,#30183,
#30184,#30185,#30186,#30187,#30188,#30189,#30190,#30191,#30192,#30193,#30194,
#30195,#30196,#30197,#30198,#30199,#30200,#30201,#30202,#30203,#30204,#30205,
#30206,#30207,#30208,#30209,#30210,#30211,#30212,#30213,#30214,#30215,#30216,
#30217,#30218,#30219,#30220,#30221,#30222,#30223,#30224,#30225,#30226,#30227,
#30228,#30229,#30230,#30231,#30232,#30233,#30234,#30235,#30236),
 .UNSPECIFIED.,.F.,.F.,(4,3,3,3,3,3,3,3,3,3,3,3,3,3,3,3,3,3,3,3,3,3,3,3,
3,3,3,3,3,3,3,3,3,3,3,3,3,3,3,3,3,3,3,3,3,3,3,3,3,3,3,3,4),(279.601746169492,
279.684208375528,279.766670233268,279.849131749562,279.931592931259,280.01405378521,
280.096514318265,280.178974537271,280.261434449079,280.343894060537,280.426353378493,
280.508812409795,280.591271161292,280.67372963983,280.756187852258,280.838645805422,
280.92110350617,281.003560961348,281.086018177803,281.172030404304,281.255354748728,
281.337821354173,281.420287115415,281.502752059867,281.585216214943,281.667679608052,
281.750142266601,281.832604217993,281.915065489632,281.997526108916,282.079986103243,
282.162445500008,282.244904326603,282.32736261042,282.409820378847,282.492277659272,
282.576410894684,282.658876892776,282.741341269131,282.823804133393,282.906265595184,
282.988725764105,283.071184749741,283.153642661658,283.239238507183,283.321703243783,
283.404165015785,283.486624261627,283.569081419604,283.651543937885,283.73400160874,
283.816460398691,283.838409425857),.UNSPECIFIED.);
#280=B_SPLINE_CURVE_WITH_KNOTS('',3,(#30237,#30238,#30239,#30240,#30241,
#30242,#30243,#30244,#30245,#30246,#30247,#30248,#30249,#30250,#30251,#30252,
#30253,#30254,#30255,#30256,#30257,#30258,#30259,#30260,#30261,#30262,#30263,
#30264,#30265,#30266,#30267,#30268,#30269,#30270,#30271,#30272,#30273,#30274,
#30275,#30276,#30277,#30278,#30279,#30280,#30281,#30282,#30283,#30284,#30285,
#30286,#30287,#30288,#30289,#30290,#30291,#30292,#30293,#30294,#30295,#30296,
#30297,#30298,#30299,#30300,#30301,#30302,#30303,#30304,#30305,#30306,#30307,
#30308,#30309,#30310,#30311,#30312,#30313,#30314,#30315,#30316,#30317,#30318,
#30319,#30320,#30321),.UNSPECIFIED.,.F.,.F.,(4,3,3,3,3,3,3,3,3,3,3,3,3,
3,3,3,3,3,3,3,3,3,3,3,3,3,3,3,4),(277.55569081987,277.636774286884,277.717764514931,
277.734727518672,277.81573591459,277.896820171437,277.981266209667,278.062572291388,
278.143956081171,278.225460742215,278.234604324356,278.312120102618,278.389554403028,
278.466922821455,278.544240906604,278.621524170649,278.69880125496,278.776077835447,
278.853367930843,278.930685564847,279.008091771171,279.085543780483,279.163116588805,
279.234357935726,279.326204994167,279.413442625825,279.500358458254,279.586782436634,
279.601746169492),.UNSPECIFIED.);
#281=B_SPLINE_CURVE_WITH_KNOTS('',3,(#30323,#30324,#30325,#30326,#30327,
#30328,#30329,#30330,#30331,#30332,#30333,#30334,#30335,#30336,#30337,#30338,
#30339,#30340,#30341,#30342,#30343,#30344,#30345,#30346,#30347,#30348,#30349,
#30350,#30351,#30352,#30353,#30354,#30355,#30356,#30357,#30358,#30359,#30360,
#30361,#30362,#30363,#30364,#30365,#30366,#30367,#30368,#30369,#30370,#30371,
#30372,#30373,#30374,#30375,#30376,#30377,#30378,#30379,#30380,#30381,#30382,
#30383,#30384,#30385,#30386,#30387,#30388,#30389,#30390,#30391,#30392,#30393,
#30394,#30395,#30396,#30397,#30398,#30399,#30400,#30401,#30402,#30403,#30404),
 .UNSPECIFIED.,.F.,.F.,(4,3,3,3,3,3,3,3,3,3,3,3,3,3,3,3,3,3,3,3,3,3,3,3,
3,3,3,4),(277.555563663649,277.63486458037,277.711424395415,277.787991167071,
277.864579462952,277.941203861465,278.017919785118,278.094690191056,278.171567907073,
278.189970997414,278.267565666862,278.345067932986,278.422493418071,278.499857689461,
278.577176270567,278.654471975053,278.731757019723,278.80904541167,278.88635115721,
278.963729197212,279.041144268971,279.118664883257,279.188379005465,279.272860664689,
279.357122338694,279.441244749164,279.525133664988,279.601746169492),
 .UNSPECIFIED.);
#282=B_SPLINE_CURVE_WITH_KNOTS('',3,(#30405,#30406,#30407,#30408,#30409,
#30410,#30411,#30412,#30413,#30414,#30415,#30416,#30417,#30418,#30419,#30420,
#30421,#30422,#30423,#30424,#30425,#30426,#30427,#30428,#30429,#30430,#30431,
#30432,#30433,#30434,#30435,#30436,#30437,#30438,#30439,#30440,#30441,#30442,
#30443,#30444,#30445,#30446,#30447,#30448,#30449,#30450,#30451,#30452,#30453,
#30454,#30455,#30456,#30457,#30458,#30459,#30460,#30461,#30462,#30463,#30464,
#30465,#30466,#30467,#30468,#30469,#30470,#30471,#30472,#30473,#30474,#30475,
#30476,#30477,#30478,#30479,#30480,#30481,#30482,#30483,#30484,#30485,#30486,
#30487,#30488,#30489,#30490,#30491,#30492,#30493,#30494,#30495,#30496,#30497,
#30498,#30499,#30500,#30501,#30502,#30503,#30504,#30505,#30506,#30507,#30508,
#30509,#30510,#30511,#30512,#30513,#30514,#30515,#30516,#30517,#30518,#30519,
#30520,#30521,#30522,#30523,#30524,#30525,#30526,#30527,#30528,#30529,#30530,
#30531,#30532,#30533,#30534,#30535,#30536,#30537,#30538,#30539,#30540,#30541,
#30542,#30543,#30544,#30545,#30546,#30547,#30548,#30549,#30550,#30551,#30552,
#30553,#30554,#30555,#30556,#30557,#30558,#30559,#30560,#30561),
 .UNSPECIFIED.,.F.,.F.,(4,3,3,3,3,3,3,3,3,3,3,3,3,3,3,3,3,3,3,3,3,3,3,3,
3,3,3,3,3,3,3,3,3,3,3,3,3,3,3,3,3,3,3,3,3,3,3,3,3,3,3,3,4),(279.601746169492,
279.684208375528,279.766670233268,279.849131749562,279.931592931259,280.01405378521,
280.096514318265,280.178974537271,280.261434449079,280.343894060537,280.426353378493,
280.508812409795,280.591271161292,280.67372963983,280.756187852258,280.838645805422,
280.92110350617,281.003560961348,281.086018177803,281.172030404304,281.255354748728,
281.337821354173,281.420287115415,281.502752059867,281.585216214943,281.667679608052,
281.750142266601,281.832604217993,281.915065489632,281.997526108916,282.079986103243,
282.162445500008,282.244904326603,282.32736261042,282.409820378847,282.492277659272,
282.576410894684,282.658876892775,282.741341269131,282.823804133393,282.906265595184,
282.988725764105,283.071184749741,283.153642661658,283.239238507183,283.321703243783,
283.404165015785,283.486624261627,283.569081419604,283.651543937885,283.73400160874,
283.816460398691,283.838409425856),.UNSPECIFIED.);
#283=B_SPLINE_CURVE_WITH_KNOTS('',3,(#30567,#30568,#30569,#30570,#30571,
#30572,#30573,#30574,#30575,#30576,#30577,#30578,#30579,#30580,#30581,#30582,
#30583,#30584,#30585,#30586,#30587,#30588,#30589,#30590,#30591,#30592,#30593,
#30594,#30595,#30596,#30597,#30598,#30599,#30600,#30601,#30602,#30603,#30604,
#30605,#30606,#30607,#30608,#30609,#30610,#30611,#30612,#30613,#30614,#30615,
#30616,#30617,#30618,#30619,#30620,#30621,#30622,#30623,#30624,#30625,#30626,
#30627,#30628,#30629,#30630,#30631,#30632,#30633,#30634,#30635,#30636,#30637,
#30638,#30639,#30640,#30641,#30642,#30643,#30644,#30645,#30646,#30647,#30648,
#30649,#30650,#30651,#30652,#30653,#30654,#30655,#30656,#30657,#30658,#30659,
#30660,#30661,#30662,#30663,#30664,#30665,#30666,#30667,#30668,#30669,#30670,
#30671,#30672,#30673,#30674,#30675,#30676,#30677,#30678,#30679,#30680,#30681,
#30682,#30683,#30684,#30685,#30686,#30687,#30688,#30689,#30690,#30691,#30692,
#30693,#30694,#30695,#30696,#30697,#30698,#30699,#30700,#30701,#30702,#30703,
#30704,#30705,#30706,#30707,#30708,#30709,#30710,#30711,#30712,#30713,#30714,
#30715,#30716,#30717,#30718,#30719,#30720,#30721,#30722,#30723,#30724,#30725,
#30726,#30727,#30728,#30729,#30730,#30731,#30732),.UNSPECIFIED.,.F.,.F.,
(4,3,3,3,3,3,3,3,3,3,3,3,3,3,3,3,3,3,3,3,3,3,3,3,3,3,3,3,3,3,3,3,3,3,3,
3,3,3,3,3,3,3,3,3,3,3,3,3,3,3,3,3,3,3,3,4),(285.884931476672,285.975939179837,
286.067542544567,286.159888532299,286.232633215311,286.309481838498,286.386236684895,
286.462914024299,286.539530064074,286.616100962699,286.693136695697,286.769679114403,
286.846227450965,286.922796282413,287.00019391848,287.076884999432,287.154635913057,
287.232386826681,287.309904378299,287.387334597719,287.464693140614,287.541995611201,
287.619257573152,287.696504798934,287.773746310141,287.850996160374,287.928268405287,
288.005621363258,288.083015755567,288.160524083235,288.23214043805,288.309657807246,
288.387087874697,288.464446295967,288.541748675182,288.619010575945,288.696257786636,
288.773499310854,288.8507492022,288.928021516344,289.00537458757,289.082769117321,
289.160277622283,289.231894049419,289.308721255141,289.385457937991,289.462120354592,
289.538724701759,289.615288304219,289.691830941501,289.768367193544,289.844911634042,
289.92151149413,289.998141634467,290.074856761555,290.120845093709),
 .UNSPECIFIED.);
#284=B_SPLINE_CURVE_WITH_KNOTS('',3,(#30733,#30734,#30735,#30736,#30737,
#30738,#30739,#30740,#30741,#30742,#30743,#30744,#30745,#30746,#30747,#30748,
#30749,#30750,#30751,#30752,#30753,#30754,#30755,#30756,#30757,#30758,#30759,
#30760,#30761,#30762,#30763,#30764,#30765,#30766,#30767,#30768,#30769,#30770,
#30771,#30772,#30773,#30774,#30775,#30776,#30777,#30778,#30779,#30780,#30781,
#30782,#30783,#30784,#30785,#30786,#30787,#30788,#30789,#30790,#30791,#30792,
#30793,#30794,#30795,#30796,#30797,#30798,#30799,#30800,#30801,#30802,#30803,
#30804,#30805,#30806,#30807,#30808),.UNSPECIFIED.,.F.,.F.,(4,3,3,3,3,3,
3,3,3,3,3,3,3,3,3,3,3,3,3,3,3,3,3,3,3,4),(283.838409425857,283.92087102971,
284.003331967681,284.085792267167,284.168251955563,284.250711060266,284.333169608665,
284.415627628151,284.498085146113,284.584763041773,284.667229827608,284.749694940952,
284.832158491457,284.914620588755,284.997081342456,285.079540862153,285.161999257421,
285.244456637818,285.326923024085,285.409386226098,285.491846682379,285.57430483129,
285.656770436169,285.739230315383,285.821694428747,285.884931476672),
 .UNSPECIFIED.);
#285=B_SPLINE_CURVE_WITH_KNOTS('',3,(#30810,#30811,#30812,#30813,#30814,
#30815,#30816,#30817,#30818,#30819,#30820,#30821,#30822,#30823,#30824,#30825,
#30826,#30827,#30828,#30829,#30830,#30831,#30832,#30833,#30834,#30835,#30836,
#30837,#30838,#30839,#30840,#30841,#30842,#30843,#30844,#30845,#30846,#30847,
#30848,#30849,#30850,#30851,#30852,#30853,#30854,#30855,#30856,#30857,#30858,
#30859,#30860,#30861,#30862,#30863,#30864,#30865,#30866,#30867,#30868,#30869,
#30870,#30871,#30872,#30873,#30874,#30875,#30876,#30877,#30878,#30879,#30880,
#30881,#30882,#30883,#30884,#30885),.UNSPECIFIED.,.F.,.F.,(4,3,3,3,3,3,
3,3,3,3,3,3,3,3,3,3,3,3,3,3,3,3,3,3,3,4),(283.838409425856,283.92087102971,
284.003331967681,284.085792267167,284.168251955563,284.250711060265,284.333169608665,
284.415627628151,284.498085146112,284.584763041772,284.667229827608,284.749694940952,
284.832158491457,284.914620588755,284.997081342456,285.079540862153,285.161999257421,
285.244456637818,285.326923024085,285.409386226098,285.491846682379,285.574304831289,
285.656770436169,285.739230315383,285.821694428747,285.884931476672),
 .UNSPECIFIED.);
#286=B_SPLINE_CURVE_WITH_KNOTS('',3,(#30886,#30887,#30888,#30889,#30890,
#30891,#30892,#30893,#30894),.UNSPECIFIED.,.F.,.F.,(4,1,1,1,1,1,4),(285.884931476672,
286.177235061822,286.676439065847,287.175643069873,288.174051077923,289.172459085974,
290.121294042707),.UNSPECIFIED.);
#287=B_SPLINE_CURVE_WITH_KNOTS('',3,(#30900,#30901,#30902,#30903,#30904,
#30905,#30906,#30907,#30908,#30909,#30910,#30911,#30912,#30913,#30914,#30915,
#30916,#30917,#30918,#30919,#30920,#30921,#30922,#30923,#30924,#30925,#30926,
#30927,#30928,#30929,#30930,#30931,#30932,#30933,#30934,#30935,#30936,#30937,
#30938,#30939,#30940,#30941,#30942,#30943,#30944,#30945,#30946,#30947,#30948,
#30949,#30950,#30951,#30952,#30953,#30954,#30955,#30956,#30957,#30958,#30959,
#30960,#30961,#30962,#30963,#30964,#30965,#30966,#30967,#30968,#30969,#30970,
#30971,#30972,#30973,#30974,#30975,#30976,#30977,#30978,#30979,#30980,#30981,
#30982,#30983,#30984,#30985,#30986,#30987,#30988,#30989,#30990,#30991,#30992,
#30993,#30994,#30995,#30996,#30997,#30998,#30999,#31000,#31001,#31002,#31003,
#31004,#31005,#31006,#31007,#31008,#31009,#31010,#31011,#31012,#31013,#31014,
#31015,#31016,#31017,#31018,#31019,#31020,#31021,#31022,#31023,#31024,#31025,
#31026,#31027,#31028,#31029,#31030,#31031,#31032,#31033,#31034,#31035,#31036,
#31037,#31038,#31039,#31040,#31041,#31042,#31043,#31044,#31045,#31046,#31047,
#31048,#31049,#31050,#31051,#31052,#31053,#31054,#31055,#31056,#31057,#31058,
#31059,#31060,#31061,#31062,#31063,#31064,#31065,#31066,#31067,#31068),
 .UNSPECIFIED.,.F.,.F.,(4,3,3,3,3,3,3,3,3,3,3,3,3,3,3,3,3,3,3,3,3,3,3,3,
3,3,3,3,3,3,3,3,3,3,3,3,3,3,3,3,3,3,3,3,3,3,3,3,3,3,3,3,3,3,3,3,4),(292.168116783851,
292.231154883527,292.30867066179,292.386104962201,292.463473380628,292.540791465778,
292.618074729823,292.695351814134,292.772628394622,292.849918490019,292.927236124024,
293.004642330348,293.082094339661,293.159667147983,293.230908494897,293.307757118085,
293.384511964481,293.461189303886,293.537805343661,293.614376242286,293.691411975283,
293.767954393989,293.844502730552,293.921071561999,293.998469198066,294.075160279019,
294.152911192642,294.230662106266,294.308179657884,294.385609877304,294.462968420199,
294.540270890786,294.617532852736,294.694780078519,294.772021589726,294.849271439959,
294.926543684872,295.003896642843,295.081291035152,295.15879936282,295.230415717636,
295.307933086832,295.385363154283,295.462721575553,295.540023954768,295.617285855531,
295.694533066222,295.77177459044,295.849024481786,295.92629679593,296.003649867156,
296.081044396907,296.158552901869,296.230169329005,296.307007919613,296.383745713197,
296.405440486054),.UNSPECIFIED.);
#288=B_SPLINE_CURVE_WITH_KNOTS('',3,(#31069,#31070,#31071,#31072,#31073,
#31074,#31075,#31076,#31077,#31078,#31079,#31080,#31081,#31082,#31083,#31084,
#31085,#31086,#31087,#31088,#31089,#31090,#31091,#31092,#31093,#31094,#31095,
#31096,#31097,#31098,#31099,#31100,#31101,#31102,#31103,#31104,#31105,#31106,
#31107,#31108,#31109,#31110,#31111,#31112,#31113,#31114,#31115,#31116,#31117,
#31118,#31119,#31120,#31121,#31122,#31123,#31124,#31125,#31126,#31127,#31128,
#31129,#31130,#31131,#31132,#31133,#31134,#31135,#31136,#31137,#31138,#31139,
#31140,#31141,#31142,#31143,#31144,#31145,#31146,#31147,#31148,#31149,#31150,
#31151,#31152,#31153),.UNSPECIFIED.,.F.,.F.,(4,3,3,3,3,3,3,3,3,3,3,3,3,
3,3,3,3,3,3,3,3,3,3,3,3,3,3,3,4),(290.120845093709,290.197700313849,290.231647660789,
290.309230284403,290.386720266612,290.464133243837,290.541484797339,290.61879046425,
290.696073057295,290.773344844239,290.850619844096,290.927912075034,291.005276747399,
291.082678355831,291.160186170439,291.231401272158,291.312885245113,291.394264609253,
291.4785179764,291.559671471572,291.640748149531,291.721733577321,291.731278077843,
291.809987718527,291.888741433474,291.967597102425,292.046509246341,292.125538329813,
292.16811678375),.UNSPECIFIED.);
#289=B_SPLINE_CURVE_WITH_KNOTS('',3,(#31155,#31156,#31157,#31158,#31159,
#31160),.UNSPECIFIED.,.F.,.F.,(4,1,1,4),(290.121294042707,290.170867094025,
291.169275102076,292.168116783851),.UNSPECIFIED.);
#290=B_SPLINE_CURVE_WITH_KNOTS('',3,(#31161,#31162,#31163,#31164,#31165,
#31166,#31167,#31168,#31169,#31170,#31171,#31172,#31173,#31174,#31175,#31176,
#31177,#31178,#31179,#31180,#31181,#31182,#31183,#31184,#31185,#31186,#31187,
#31188,#31189,#31190,#31191,#31192,#31193,#31194,#31195,#31196,#31197,#31198,
#31199,#31200,#31201,#31202,#31203,#31204,#31205,#31206,#31207,#31208,#31209,
#31210,#31211,#31212,#31213,#31214,#31215,#31216,#31217,#31218,#31219,#31220,
#31221,#31222,#31223,#31224,#31225,#31226,#31227,#31228,#31229,#31230,#31231,
#31232,#31233,#31234,#31235,#31236,#31237,#31238,#31239,#31240,#31241,#31242,
#31243,#31244,#31245,#31246,#31247,#31248,#31249,#31250,#31251,#31252,#31253,
#31254,#31255,#31256,#31257,#31258,#31259,#31260,#31261,#31262,#31263,#31264,
#31265,#31266,#31267,#31268,#31269,#31270,#31271,#31272,#31273,#31274,#31275,
#31276,#31277,#31278,#31279,#31280,#31281,#31282,#31283,#31284,#31285,#31286,
#31287,#31288,#31289,#31290,#31291,#31292,#31293,#31294,#31295,#31296,#31297,
#31298,#31299,#31300,#31301,#31302,#31303,#31304,#31305,#31306,#31307,#31308,
#31309,#31310,#31311,#31312,#31313,#31314,#31315,#31316,#31317,#31318,#31319,
#31320,#31321,#31322,#31323,#31324,#31325,#31326,#31327,#31328,#31329,#31330,
#31331,#31332),.UNSPECIFIED.,.F.,.F.,(4,3,3,3,3,3,3,3,3,3,3,3,3,3,3,3,3,
3,3,3,3,3,3,3,3,3,3,3,3,3,3,3,3,3,3,3,3,3,3,3,3,3,3,3,3,3,3,3,3,3,3,3,3,
3,3,3,3,4),(292.168116807891,292.245704681638,292.32320014403,292.40061882437,
292.477976296989,292.555288092261,292.632577034805,292.709855342602,292.787137029005,
292.864436106611,292.941807486204,293.019215943154,293.09672985486,293.166091118178,
293.247577432611,293.32895951497,293.413043416778,293.494200735631,293.575281519386,
293.65627151142,293.665295122204,293.746308228494,293.827396922767,293.911672473633,
293.992981940022,294.074368841233,294.155875979998,294.164499126229,294.242027279438,
294.319474154399,294.396855333107,294.474186350567,294.551482705398,294.628773005734,
294.706062913472,294.78336643547,294.860697583597,294.938117073418,295.01558243184,
295.093167818138,295.16290713428,295.239770518932,295.316540350742,295.39323288673,
295.469864321897,295.546450802681,295.623308845137,295.6998671681,295.776431502773,
295.8530164159,295.930091097508,296.006797918377,296.084056530354,296.161315142331,
296.238846498326,296.316301020837,296.393676769827,296.405239013614),
 .UNSPECIFIED.);
#291=B_SPLINE_CURVE_WITH_KNOTS('',3,(#31338,#31339,#31340,#31341,#31342,
#31343,#31344,#31345,#31346,#31347,#31348,#31349,#31350,#31351,#31352,#31353,
#31354,#31355,#31356,#31357,#31358,#31359,#31360,#31361,#31362,#31363,#31364,
#31365,#31366,#31367,#31368,#31369,#31370,#31371,#31372,#31373,#31374,#31375,
#31376,#31377,#31378,#31379,#31380,#31381,#31382,#31383,#31384,#31385,#31386,
#31387,#31388,#31389,#31390,#31391,#31392,#31393,#31394,#31395,#31396,#31397,
#31398,#31399,#31400,#31401,#31402,#31403,#31404,#31405,#31406,#31407,#31408,
#31409,#31410,#31411,#31412,#31413,#31414,#31415,#31416,#31417,#31418,#31419,
#31420,#31421,#31422,#31423,#31424,#31425,#31426,#31427,#31428,#31429,#31430,
#31431,#31432,#31433,#31434,#31435,#31436,#31437,#31438,#31439,#31440,#31441,
#31442,#31443,#31444,#31445,#31446,#31447,#31448,#31449,#31450,#31451,#31452,
#31453,#31454,#31455,#31456,#31457,#31458,#31459,#31460,#31461,#31462,#31463,
#31464,#31465,#31466,#31467,#31468,#31469,#31470,#31471,#31472,#31473,#31474,
#31475,#31476,#31477,#31478,#31479,#31480,#31481,#31482,#31483,#31484,#31485,
#31486,#31487,#31488,#31489,#31490,#31491,#31492,#31493,#31494,#31495,#31496,
#31497,#31498,#31499,#31500,#31501,#31502,#31503,#31504,#31505,#31506),
 .UNSPECIFIED.,.F.,.F.,(4,3,3,3,3,3,3,3,3,3,3,3,3,3,3,3,3,3,3,3,3,3,3,3,
3,3,3,3,3,3,3,3,3,3,3,3,3,3,3,3,3,3,3,3,3,3,3,3,3,3,3,3,3,3,3,3,4),(298.451302091176,
298.526537089347,298.601724537959,298.676880845604,298.729553357428,298.810561753332,
298.891646010163,298.976092048401,299.057398130108,299.138781919876,299.220286580905,
299.229430163113,299.306945941376,299.384380241787,299.461748660214,299.539066745364,
299.616350009409,299.693627093721,299.770903674209,299.848193769606,299.925511403611,
300.002917609935,300.080369619249,300.157942427571,300.229183774482,300.306032397669,
300.382787244066,300.459464583471,300.536080623246,300.612651521871,300.689687254868,
300.766229673574,300.842778010136,300.919346841584,300.996744477651,301.073435558604,
301.151186472228,301.228937385852,301.30645493747,301.38388515689,301.461243699785,
301.538546170373,301.615808132323,301.693055358106,301.770296869313,301.847546719545,
301.924818964458,302.002171922429,302.079566314738,302.157074642406,302.228690997221,
302.306212598582,302.383649456979,302.460999992763,302.538300277288,302.615564024868,
302.688147330401),.UNSPECIFIED.);
#292=B_SPLINE_CURVE_WITH_KNOTS('',3,(#31507,#31508,#31509,#31510,#31511,
#31512,#31513,#31514,#31515,#31516,#31517,#31518,#31519,#31520,#31521,#31522,
#31523,#31524,#31525,#31526,#31527,#31528,#31529,#31530,#31531,#31532,#31533,
#31534,#31535,#31536,#31537,#31538,#31539,#31540,#31541,#31542,#31543,#31544,
#31545,#31546,#31547,#31548,#31549,#31550,#31551,#31552,#31553,#31554,#31555,
#31556,#31557,#31558,#31559,#31560,#31561,#31562,#31563,#31564,#31565,#31566,
#31567,#31568,#31569,#31570,#31571,#31572,#31573,#31574,#31575,#31576,#31577,
#31578,#31579,#31580,#31581,#31582,#31583,#31584,#31585,#31586,#31587,#31588),
 .UNSPECIFIED.,.F.,.F.,(4,3,3,3,3,3,3,3,3,3,3,3,3,3,3,3,3,3,3,3,3,3,3,3,
3,3,3,4),(296.405440486054,296.482081738333,296.558670776144,296.635223736031,
296.711769685511,296.788315197546,296.864874847928,296.941463218834,297.018140894284,
297.094866423305,297.171710683336,297.229922940374,297.307505563988,297.384995546197,
297.462408523422,297.539760076923,297.617065743835,297.694348336879,297.771620123823,
297.84889512368,297.926187354618,298.003552026983,298.080953635415,298.158461450023,
298.229676551744,298.329594899379,298.428201754546,298.451302091031),
 .UNSPECIFIED.);
#293=B_SPLINE_CURVE_WITH_KNOTS('',3,(#31590,#31591,#31592,#31593,#31594,
#31595,#31596,#31597,#31598,#31599,#31600,#31601,#31602,#31603,#31604,#31605,
#31606,#31607,#31608,#31609,#31610,#31611,#31612,#31613,#31614,#31615,#31616,
#31617,#31618,#31619,#31620,#31621,#31622,#31623,#31624,#31625,#31626,#31627,
#31628,#31629,#31630,#31631,#31632,#31633,#31634,#31635,#31636,#31637,#31638,
#31639,#31640,#31641,#31642,#31643,#31644,#31645,#31646,#31647,#31648,#31649,
#31650,#31651,#31652,#31653,#31654,#31655,#31656,#31657,#31658,#31659,#31660,
#31661,#31662,#31663,#31664,#31665,#31666,#31667,#31668,#31669,#31670,#31671),
 .UNSPECIFIED.,.F.,.F.,(4,3,3,3,3,3,3,3,3,3,3,3,3,3,3,3,3,3,3,3,3,3,3,3,
3,3,3,4),(296.405239013614,296.4825477514,296.559818493679,296.637077647407,
296.714333326596,296.791599572495,296.868890429628,296.946262650532,297.023678284972,
297.101204017291,297.159723150382,297.237253268445,297.314696297761,297.392067879587,
297.469383603947,297.546659020508,297.623919896534,297.70117520788,297.778438995972,
297.855725304356,297.933092165962,298.010500559894,298.088022192766,298.158131158433,
298.252011547859,298.345286298481,298.437505102726,298.451302091031),
 .UNSPECIFIED.);
#294=B_SPLINE_CURVE_WITH_KNOTS('',3,(#31672,#31673,#31674,#31675,#31676,
#31677,#31678,#31679,#31680,#31681,#31682,#31683,#31684,#31685,#31686,#31687,
#31688,#31689,#31690,#31691,#31692,#31693,#31694,#31695,#31696,#31697,#31698,
#31699,#31700,#31701,#31702,#31703,#31704,#31705,#31706,#31707,#31708,#31709,
#31710,#31711,#31712,#31713,#31714,#31715,#31716,#31717,#31718,#31719,#31720,
#31721,#31722,#31723,#31724,#31725,#31726,#31727,#31728,#31729,#31730,#31731,
#31732,#31733,#31734,#31735,#31736,#31737,#31738,#31739,#31740,#31741,#31742,
#31743,#31744,#31745,#31746,#31747,#31748,#31749,#31750,#31751,#31752,#31753,
#31754,#31755,#31756,#31757,#31758,#31759,#31760,#31761,#31762,#31763,#31764,
#31765,#31766,#31767,#31768,#31769,#31770,#31771,#31772,#31773,#31774,#31775,
#31776,#31777,#31778,#31779,#31780,#31781,#31782,#31783,#31784,#31785,#31786,
#31787,#31788,#31789,#31790,#31791,#31792,#31793,#31794,#31795,#31796,#31797,
#31798,#31799,#31800,#31801,#31802,#31803,#31804,#31805,#31806,#31807,#31808,
#31809,#31810,#31811,#31812,#31813,#31814,#31815,#31816,#31817,#31818,#31819,
#31820,#31821,#31822,#31823,#31824,#31825,#31826,#31827,#31828),
 .UNSPECIFIED.,.F.,.F.,(4,3,3,3,3,3,3,3,3,3,3,3,3,3,3,3,3,3,3,3,3,3,3,3,
3,3,3,3,3,3,3,3,3,3,3,3,3,3,3,3,3,3,3,3,3,3,3,3,3,3,3,3,4),(298.451302091031,
298.533764297067,298.616226154807,298.698687671101,298.781148852798,298.86360970675,
298.946070239804,299.02853045881,299.110990370618,299.193449982076,299.275909300032,
299.358368331334,299.440827082831,299.52328556137,299.605743773797,299.688201726962,
299.770659427709,299.853116882887,299.935574099342,300.021586325843,300.104910670267,
300.187377275712,300.269843036954,300.352307981406,300.434772136482,300.517235529591,
300.59969818814,300.682160139532,300.764621411171,300.847082030455,300.929542024782,
301.012001421547,301.094460248142,301.176918531959,301.259376300386,301.341833580811,
301.425966816223,301.508432814314,301.59089719067,301.673360054932,301.755821516723,
301.838281685644,301.920740671279,302.003198583197,302.088794428721,302.171259165321,
302.253720937323,302.336180183165,302.418637341143,302.501099859424,302.583557530279,
302.66601632023,302.687965347395),.UNSPECIFIED.);
#295=B_SPLINE_CURVE_WITH_KNOTS('',3,(#31834,#31835,#31836,#31837,#31838,
#31839,#31840,#31841,#31842,#31843,#31844,#31845,#31846,#31847,#31848,#31849,
#31850,#31851,#31852,#31853,#31854,#31855,#31856,#31857,#31858,#31859,#31860,
#31861,#31862,#31863,#31864,#31865,#31866,#31867,#31868,#31869,#31870,#31871,
#31872,#31873,#31874,#31875,#31876,#31877,#31878,#31879,#31880,#31881,#31882,
#31883,#31884,#31885,#31886,#31887,#31888,#31889,#31890,#31891,#31892,#31893,
#31894,#31895,#31896,#31897,#31898,#31899,#31900,#31901,#31902,#31903,#31904,
#31905,#31906,#31907,#31908,#31909,#31910,#31911,#31912,#31913,#31914,#31915,
#31916,#31917,#31918,#31919,#31920,#31921,#31922,#31923,#31924,#31925,#31926,
#31927,#31928,#31929,#31930,#31931,#31932,#31933,#31934,#31935,#31936,#31937,
#31938,#31939,#31940,#31941,#31942,#31943,#31944,#31945,#31946,#31947,#31948,
#31949,#31950,#31951,#31952,#31953,#31954,#31955,#31956,#31957,#31958,#31959,
#31960,#31961,#31962,#31963,#31964,#31965,#31966,#31967,#31968,#31969,#31970,
#31971,#31972,#31973,#31974,#31975,#31976,#31977,#31978,#31979,#31980,#31981,
#31982,#31983,#31984,#31985,#31986,#31987,#31988,#31989,#31990,#31991,#31992,
#31993,#31994,#31995,#31996,#31997,#31998,#31999,#32000,#32001,#32002),
 .UNSPECIFIED.,.F.,.F.,(4,3,3,3,3,3,3,3,3,3,3,3,3,3,3,3,3,3,3,3,3,3,3,3,
3,3,3,3,3,3,3,3,3,3,3,3,3,3,3,3,3,3,3,3,3,3,3,3,3,3,3,3,3,3,3,3,4),(304.734487420068,
304.814617174688,304.894819206556,304.978102362749,305.058528818975,305.143240325152,
305.227951831329,305.309435804284,305.390815168424,305.475068535572,305.556222030744,
305.637298708704,305.718284136494,305.727828637014,305.808837032918,305.889921289749,
305.974367327987,306.055673409694,306.137057199462,306.218561860491,306.227705442699,
306.305221220962,306.382655521373,306.4600239398,306.53734202495,306.614625288994,
306.691902373306,306.769178953793,306.84646904919,306.923786683195,307.001192889519,
307.078644898833,307.156217707154,307.227459054068,307.304307677255,307.381062523652,
307.457739863057,307.534355902832,307.610926801457,307.687962534454,307.76450495316,
307.841053289722,307.91762212117,307.995019757237,308.07171083819,308.149461751813,
308.227212665437,308.3047445604,308.382186284033,308.459537513191,308.536836778233,
308.614098178985,308.691335791111,308.768579033392,308.845824246208,308.923110025222,
308.970560612253),.UNSPECIFIED.);
#296=B_SPLINE_CURVE_WITH_KNOTS('',3,(#32003,#32004,#32005,#32006,#32007,
#32008,#32009,#32010,#32011,#32012,#32013,#32014,#32015,#32016,#32017,#32018,
#32019,#32020,#32021,#32022,#32023,#32024,#32025,#32026,#32027,#32028,#32029,
#32030,#32031,#32032,#32033,#32034,#32035,#32036,#32037,#32038,#32039,#32040,
#32041,#32042,#32043,#32044,#32045,#32046,#32047,#32048,#32049,#32050,#32051,
#32052,#32053,#32054,#32055,#32056,#32057,#32058,#32059,#32060,#32061,#32062,
#32063,#32064,#32065,#32066,#32067,#32068,#32069,#32070,#32071,#32072,#32073,
#32074,#32075,#32076,#32077,#32078,#32079,#32080,#32081,#32082,#32083,#32084),
 .UNSPECIFIED.,.F.,.F.,(4,3,3,3,3,3,3,3,3,3,3,3,3,3,3,3,3,3,3,3,3,3,3,3,
3,3,3,4),(302.688147330401,302.765388799308,302.842637787327,302.919908349782,
302.997259325273,303.074650996299,303.152157927652,303.228444608591,303.305265805746,
303.38199776796,303.458656746108,303.53525893257,303.611820474451,303.68886769264,
303.765411867284,303.841966147329,303.918545112309,303.995958389222,304.072669869529,
304.150434044744,304.22819821996,304.310669468899,304.392996678695,304.478369358574,
304.560356137155,304.642222416059,304.723932153712,304.73448739821),
 .UNSPECIFIED.);
#297=B_SPLINE_CURVE_WITH_KNOTS('',3,(#32086,#32087,#32088,#32089,#32090,
#32091,#32092,#32093,#32094,#32095,#32096,#32097,#32098,#32099,#32100,#32101,
#32102,#32103,#32104,#32105,#32106,#32107,#32108,#32109,#32110,#32111,#32112,
#32113,#32114,#32115,#32116,#32117,#32118,#32119,#32120,#32121,#32122,#32123,
#32124,#32125,#32126,#32127,#32128,#32129,#32130,#32131,#32132,#32133,#32134,
#32135,#32136,#32137,#32138,#32139,#32140,#32141,#32142,#32143,#32144,#32145,
#32146,#32147,#32148,#32149,#32150,#32151,#32152,#32153,#32154,#32155,#32156,
#32157,#32158,#32159,#32160,#32161),.UNSPECIFIED.,.F.,.F.,(4,3,3,3,3,3,
3,3,3,3,3,3,3,3,3,3,3,3,3,3,3,3,3,3,3,4),(302.687965347395,302.770426951249,
302.852887889219,302.935348188705,303.017807877102,303.100266981804,303.182725530203,
303.265183549689,303.347641067651,303.434318963311,303.516785749146,303.59925086249,
303.681714412995,303.764176510293,303.846637263994,303.929096783691,304.011555178959,
304.094012559356,304.176478945622,304.258942147636,304.341402603916,304.423860752827,
304.506326357706,304.588786236921,304.671250350285,304.73448739821),
 .UNSPECIFIED.);
#298=B_SPLINE_CURVE_WITH_KNOTS('',3,(#32162,#32163,#32164,#32165,#32166,
#32167,#32168,#32169,#32170,#32171,#32172,#32173,#32174,#32175,#32176,#32177,
#32178,#32179,#32180,#32181,#32182,#32183,#32184,#32185,#32186,#32187,#32188,
#32189,#32190,#32191,#32192,#32193,#32194,#32195,#32196,#32197,#32198,#32199,
#32200,#32201,#32202,#32203,#32204,#32205,#32206,#32207,#32208,#32209,#32210,
#32211,#32212,#32213,#32214,#32215,#32216,#32217,#32218,#32219,#32220,#32221,
#32222,#32223,#32224,#32225,#32226,#32227,#32228,#32229,#32230,#32231,#32232,
#32233,#32234,#32235,#32236,#32237,#32238,#32239,#32240,#32241,#32242,#32243,
#32244,#32245,#32246,#32247,#32248,#32249,#32250,#32251,#32252,#32253,#32254,
#32255,#32256,#32257,#32258,#32259,#32260,#32261,#32262,#32263,#32264,#32265,
#32266,#32267,#32268,#32269,#32270,#32271,#32272,#32273,#32274,#32275,#32276,
#32277,#32278,#32279,#32280,#32281,#32282,#32283,#32284,#32285,#32286,#32287,
#32288,#32289,#32290,#32291,#32292,#32293,#32294,#32295,#32296,#32297,#32298,
#32299,#32300,#32301,#32302,#32303,#32304,#32305,#32306,#32307,#32308,#32309,
#32310,#32311,#32312,#32313,#32314,#32315,#32316,#32317,#32318,#32319,#32320,
#32321,#32322,#32323,#32324,#32325,#32326,#32327,#32328,#32329,#32330),
 .UNSPECIFIED.,.F.,.F.,(4,3,3,3,3,3,3,3,3,3,3,3,3,3,3,3,3,3,3,3,3,3,3,3,
3,3,3,3,3,3,3,3,3,3,3,3,3,3,3,3,3,3,3,3,3,3,3,3,3,3,3,3,3,3,3,3,4),(304.73448739821,
304.819534618296,304.905005814465,304.990685396803,305.076670221159,305.146987214789,
305.223823246912,305.300570262639,305.377244500202,305.453862139724,305.530439316351,
305.607308804662,305.683868907185,305.760439204332,305.837034265354,305.914124504726,
305.990851701307,306.068123462074,306.14539522284,306.222989892274,306.300492158384,
306.377917643455,306.455281914832,306.532600495923,306.609896200394,306.68718124505,
306.764469636983,306.841775382509,306.919153422496,306.996568494241,307.074089108512,
307.143803230891,307.225289545324,307.306671627683,307.390755529491,307.471912848344,
307.552993632099,307.633983624133,307.643007234916,307.724020341206,307.80510903548,
307.889384586345,307.970694052735,308.052080953946,308.13358809271,308.142211238942,
308.219747731918,308.297201075221,308.37458685742,308.451916100716,308.529214275392,
308.606495402004,308.683773488848,308.761089684787,308.838425502775,308.915831968875,
308.970671977892),.UNSPECIFIED.);
#299=B_SPLINE_CURVE_WITH_KNOTS('',3,(#32336,#32337,#32338,#32339,#32340,
#32341,#32342,#32343,#32344,#32345,#32346,#32347,#32348,#32349,#32350,#32351,
#32352,#32353,#32354,#32355,#32356,#32357,#32358,#32359,#32360,#32361,#32362,
#32363,#32364,#32365,#32366,#32367,#32368,#32369,#32370,#32371,#32372,#32373,
#32374,#32375,#32376,#32377,#32378,#32379,#32380,#32381,#32382,#32383,#32384,
#32385,#32386,#32387,#32388,#32389,#32390,#32391,#32392,#32393,#32394,#32395,
#32396,#32397,#32398,#32399,#32400,#32401,#32402,#32403,#32404,#32405,#32406,
#32407,#32408,#32409,#32410,#32411,#32412,#32413,#32414,#32415,#32416,#32417,
#32418,#32419,#32420,#32421,#32422,#32423,#32424,#32425,#32426,#32427,#32428,
#32429,#32430,#32431,#32432,#32433,#32434,#32435,#32436,#32437,#32438,#32439,
#32440,#32441,#32442,#32443,#32444,#32445,#32446,#32447,#32448,#32449,#32450,
#32451,#32452,#32453,#32454,#32455,#32456,#32457,#32458,#32459,#32460,#32461,
#32462,#32463,#32464,#32465,#32466,#32467,#32468,#32469,#32470,#32471,#32472,
#32473,#32474,#32475,#32476,#32477,#32478,#32479,#32480,#32481,#32482,#32483,
#32484,#32485,#32486,#32487,#32488,#32489,#32490,#32491,#32492),
 .UNSPECIFIED.,.F.,.F.,(4,3,3,3,3,3,3,3,3,3,3,3,3,3,3,3,3,3,3,3,3,3,3,3,
3,3,3,3,3,3,3,3,3,3,3,3,3,3,3,3,3,3,3,3,3,3,3,3,3,3,3,3,4),(311.01767270539,
311.100134911426,311.182596769166,311.26505828546,311.347519467157,311.429980321108,
311.512440854162,311.594901073169,311.677360984977,311.759820596435,311.842279914391,
311.924738945693,312.007197697189,312.089656175728,312.172114388156,312.25457234132,
312.337030042068,312.419487497245,312.5019447137,312.587956940202,312.671281284625,
312.753747890071,312.836213651312,312.918678595765,313.001142750841,313.08360614395,
313.166068802498,313.248530753891,313.33099202553,313.413452644814,313.495912639141,
313.578372035905,313.6608308625,313.743289146317,313.825746914745,313.90820419517,
313.992337430581,314.074803428673,314.157267805029,314.239730669291,314.322192131081,
314.404652300003,314.487111285638,314.569569197555,314.65516504308,314.73762977968,
314.820091551682,314.902550797524,314.985007955501,315.067470473783,315.149928144638,
315.232386934588,315.254335961755),.UNSPECIFIED.);
#300=B_SPLINE_CURVE_WITH_KNOTS('',3,(#32493,#32494,#32495,#32496,#32497,
#32498,#32499,#32500,#32501,#32502,#32503,#32504,#32505,#32506,#32507,#32508,
#32509,#32510,#32511,#32512,#32513,#32514,#32515,#32516,#32517,#32518,#32519,
#32520,#32521,#32522,#32523,#32524,#32525,#32526,#32527,#32528,#32529,#32530,
#32531,#32532,#32533,#32534,#32535,#32536,#32537,#32538,#32539,#32540,#32541,
#32542,#32543,#32544,#32545,#32546,#32547,#32548,#32549,#32550,#32551,#32552,
#32553,#32554,#32555,#32556,#32557,#32558,#32559,#32560,#32561,#32562,#32563,
#32564,#32565,#32566,#32567,#32568,#32569,#32570,#32571,#32572,#32573,#32574,
#32575,#32576,#32577),.UNSPECIFIED.,.F.,.F.,(4,3,3,3,3,3,3,3,3,3,3,3,3,
3,3,3,3,3,3,3,3,3,3,3,3,3,3,3,4),(308.970560612253,309.047937498109,309.125363586437,
309.20289114427,309.226966276807,309.304483646003,309.381913713454,309.459272134724,
309.536574513939,309.613836414702,309.691083625393,309.768325149612,309.845575040958,
309.922847355101,310.000200426327,310.077594956079,310.155103461041,310.226719888176,
310.302445972709,310.37808266474,310.453646918017,310.529150574392,310.604621220853,
310.680074035677,310.755524180882,310.831013238727,310.906524250404,310.982104336895,
311.016482328777),.UNSPECIFIED.);
#301=B_SPLINE_CURVE_WITH_KNOTS('',3,(#32579,#32580,#32581,#32582,#32583,
#32584,#32585,#32586,#32587,#32588,#32589,#32590,#32591,#32592,#32593,#32594,
#32595,#32596,#32597,#32598,#32599,#32600,#32601,#32602,#32603,#32604,#32605,
#32606,#32607,#32608,#32609,#32610,#32611,#32612,#32613,#32614,#32615,#32616,
#32617,#32618,#32619,#32620,#32621,#32622,#32623,#32624,#32625,#32626,#32627,
#32628,#32629,#32630,#32631,#32632,#32633,#32634,#32635,#32636,#32637,#32638,
#32639,#32640,#32641,#32642,#32643,#32644,#32645,#32646,#32647,#32648,#32649,
#32650,#32651,#32652,#32653,#32654,#32655,#32656,#32657,#32658,#32659,#32660,
#32661,#32662,#32663),.UNSPECIFIED.,.F.,.F.,(4,3,3,3,3,3,3,3,3,3,3,3,3,
3,3,3,3,3,3,3,3,3,3,3,3,3,3,3,4),(308.970671977892,309.048177449884,309.125787753225,
309.140619246993,309.217482631645,309.294252463455,309.370944999443,309.44757643461,
309.524162915393,309.60102095785,309.677579280813,309.754143615486,309.830728528613,
309.90780321022,309.984510031089,310.061768643067,310.139027255044,310.215551403013,
310.29198879418,310.368355917333,310.444669199715,310.520948512192,310.597211241812,
310.673472180531,310.749746117098,310.826082051884,310.902452802341,310.978912686717,
311.017672705276),.UNSPECIFIED.);
#302=B_SPLINE_CURVE_WITH_KNOTS('',3,(#32664,#32665,#32666,#32667,#32668,
#32669,#32670,#32671,#32672,#32673,#32674,#32675,#32676,#32677,#32678,#32679,
#32680,#32681,#32682,#32683,#32684,#32685,#32686,#32687,#32688,#32689,#32690,
#32691,#32692,#32693,#32694,#32695,#32696,#32697,#32698,#32699,#32700,#32701,
#32702,#32703,#32704,#32705,#32706,#32707,#32708,#32709,#32710,#32711,#32712,
#32713,#32714,#32715,#32716,#32717,#32718,#32719,#32720,#32721,#32722,#32723,
#32724,#32725,#32726,#32727,#32728,#32729,#32730,#32731,#32732,#32733,#32734,
#32735,#32736,#32737,#32738,#32739,#32740,#32741,#32742,#32743,#32744,#32745,
#32746,#32747,#32748,#32749,#32750,#32751,#32752,#32753,#32754,#32755,#32756,
#32757,#32758,#32759,#32760,#32761,#32762,#32763,#32764,#32765,#32766,#32767,
#32768,#32769,#32770,#32771,#32772,#32773,#32774,#32775,#32776,#32777,#32778,
#32779,#32780,#32781,#32782,#32783,#32784,#32785,#32786,#32787,#32788,#32789,
#32790,#32791,#32792,#32793,#32794,#32795,#32796,#32797,#32798,#32799,#32800,
#32801,#32802,#32803,#32804,#32805,#32806,#32807,#32808,#32809,#32810,#32811,
#32812,#32813,#32814,#32815,#32816,#32817,#32818,#32819,#32820,#32821,#32822,
#32823,#32824,#32825,#32826,#32827,#32828,#32829,#32830,#32831,#32832),
 .UNSPECIFIED.,.F.,.F.,(4,3,3,3,3,3,3,3,3,3,3,3,3,3,3,3,3,3,3,3,3,3,3,3,
3,3,3,3,3,3,3,3,3,3,3,3,3,3,3,3,3,3,3,3,3,3,3,3,3,3,3,3,3,3,3,3,4),(311.01767270539,
311.137435263095,311.214965381158,311.292408410474,311.3697799923,311.44709571666,
311.524371133221,311.601632009246,311.678887320593,311.756151108684,311.833437417069,
311.910804278675,311.988212672607,312.065734305479,312.135843271145,312.212679303268,
312.289426318995,312.366100556558,312.442718196079,312.519295372706,312.596164861018,
312.67272496354,312.749295260688,312.82589032171,312.902980561082,312.979707757663,
313.056979518429,313.134251279196,313.21184594863,313.289348214741,313.366773699811,
313.444137971188,313.521456552279,313.598752256751,313.676037301407,313.75332569334,
313.830631438866,313.908009478853,313.985424550598,314.062945164869,314.132659287247,
314.21414560168,314.295527684039,314.379611585847,314.460768904701,314.541849688455,
314.622839680489,314.631863291273,314.712876397564,314.793965091837,314.878240642702,
314.959550109092,315.040937010302,315.122444149067,315.131067295298,315.20859582047,
315.254853130802),.UNSPECIFIED.);
#303=B_SPLINE_CURVE_WITH_KNOTS('',3,(#32838,#32839,#32840,#32841,#32842,
#32843,#32844,#32845,#32846,#32847,#32848,#32849,#32850,#32851,#32852,#32853,
#32854,#32855,#32856,#32857,#32858,#32859,#32860,#32861,#32862,#32863,#32864,
#32865,#32866,#32867,#32868,#32869,#32870,#32871,#32872,#32873,#32874,#32875,
#32876,#32877,#32878,#32879,#32880,#32881,#32882,#32883,#32884,#32885,#32886,
#32887,#32888,#32889,#32890,#32891,#32892,#32893,#32894,#32895,#32896,#32897,
#32898,#32899,#32900,#32901,#32902,#32903,#32904,#32905,#32906,#32907,#32908,
#32909,#32910,#32911,#32912,#32913,#32914,#32915,#32916,#32917,#32918,#32919,
#32920,#32921,#32922,#32923,#32924,#32925,#32926,#32927,#32928,#32929,#32930,
#32931,#32932,#32933,#32934,#32935,#32936,#32937,#32938,#32939,#32940,#32941,
#32942,#32943,#32944,#32945,#32946,#32947,#32948,#32949,#32950,#32951,#32952,
#32953,#32954,#32955,#32956,#32957,#32958,#32959,#32960,#32961,#32962,#32963,
#32964,#32965,#32966,#32967,#32968,#32969,#32970,#32971,#32972,#32973,#32974,
#32975,#32976,#32977,#32978,#32979,#32980,#32981,#32982,#32983,#32984,#32985,
#32986,#32987,#32988,#32989,#32990,#32991,#32992,#32993,#32994,#32995,#32996,
#32997,#32998,#32999,#33000,#33001,#33002,#33003,#33004,#33005,#33006,#33007,
#33008,#33009),.UNSPECIFIED.,.F.,.F.,(4,3,3,3,3,3,3,3,3,3,3,3,3,3,3,3,3,
3,3,3,3,3,3,3,3,3,3,3,3,3,3,3,3,3,3,3,3,3,3,3,3,3,3,3,3,3,3,3,3,3,3,3,3,
3,3,3,3,4),(317.301428870433,317.377425349235,317.453339462372,317.52918796026,
317.604987526603,317.682457683169,317.758222508873,317.833991512175,317.909779722749,
317.988521986845,318.064434773949,318.140401796158,318.216471684351,318.224748779131,
318.302331402745,318.379821384954,318.457234362179,318.53458591568,318.611891582591,
318.689174175636,318.76644596258,318.843720962437,318.921013193375,318.998377865739,
319.075779474172,319.15328728878,319.2245023905,319.305986363455,319.387365727595,
319.471619094743,319.552772589915,319.633849267873,319.714834695664,319.724379196185,
319.805387592089,319.886471848921,319.970917887158,320.052223968865,320.133607758634,
320.215112419662,320.22425600187,320.301771780133,320.379206080543,320.456574498971,
320.533892584121,320.611175848165,320.688452932477,320.765729512964,320.843019608362,
320.920337242366,320.99774344869,321.075195458004,321.152768266326,321.224009613239,
321.302574934875,321.379326931844,321.458798915814,321.538270899783),
 .UNSPECIFIED.);
#304=B_SPLINE_CURVE_WITH_KNOTS('',3,(#33010,#33011,#33012,#33013,#33014,
#33015,#33016,#33017,#33018,#33019,#33020,#33021,#33022,#33023,#33024,#33025,
#33026,#33027,#33028,#33029,#33030,#33031,#33032,#33033,#33034,#33035,#33036,
#33037,#33038,#33039,#33040,#33041,#33042,#33043,#33044,#33045,#33046,#33047,
#33048,#33049,#33050,#33051,#33052,#33053,#33054,#33055,#33056,#33057,#33058,
#33059,#33060,#33061,#33062,#33063,#33064,#33065,#33066,#33067,#33068,#33069,
#33070,#33071,#33072,#33073,#33074,#33075,#33076,#33077,#33078,#33079,#33080,
#33081,#33082,#33083,#33084,#33085),.UNSPECIFIED.,.F.,.F.,(4,3,3,3,3,3,
3,3,3,3,3,3,3,3,3,3,3,3,3,3,3,3,3,3,3,4),(315.254335961755,315.336797565608,
315.419258503579,315.501718803065,315.584178491462,315.666637596164,315.749096144563,
315.831554164049,315.914011682011,316.000689577671,316.083156363506,316.16562147685,
316.248085027355,316.330547124653,316.413007878354,316.495467398051,316.577925793319,
316.660383173716,316.742849559983,316.825312761996,316.907773218277,316.990231367188,
317.072696972067,317.155156851281,317.237620964645,317.30085801257),
 .UNSPECIFIED.);
#305=B_SPLINE_CURVE_WITH_KNOTS('',3,(#33087,#33088,#33089,#33090,#33091,
#33092,#33093,#33094,#33095,#33096,#33097,#33098,#33099,#33100,#33101,#33102,
#33103,#33104,#33105,#33106,#33107,#33108,#33109,#33110,#33111,#33112,#33113,
#33114,#33115,#33116,#33117,#33118,#33119,#33120,#33121,#33122,#33123,#33124,
#33125,#33126,#33127,#33128,#33129,#33130,#33131,#33132,#33133,#33134,#33135,
#33136,#33137,#33138,#33139,#33140,#33141,#33142,#33143,#33144,#33145,#33146,
#33147,#33148,#33149,#33150,#33151,#33152,#33153,#33154,#33155,#33156,#33157,
#33158,#33159,#33160,#33161,#33162,#33163,#33164,#33165,#33166,#33167,#33168),
 .UNSPECIFIED.,.F.,.F.,(4,3,3,3,3,3,3,3,3,3,3,3,3,3,3,3,3,3,3,3,3,3,3,3,
3,3,3,4),(315.254853130802,315.332258903035,315.409608261007,315.486916716749,
315.567236540074,315.644524969973,315.721821920583,315.799141401053,315.876497430504,
315.953944630171,316.031445729455,316.109053139725,316.129475303349,316.206338688001,
316.283108519811,316.3598010558,316.436432490966,316.51301897175,316.589877014206,
316.66643533717,316.742999671842,316.819584584969,316.896659266577,316.973366087446,
317.050624699423,317.1278833114,317.252579983701,317.300858012569),
 .UNSPECIFIED.);
#306=B_SPLINE_CURVE_WITH_KNOTS('',3,(#33169,#33170,#33171,#33172,#33173,
#33174,#33175,#33176,#33177,#33178,#33179,#33180,#33181,#33182,#33183,#33184,
#33185,#33186,#33187,#33188,#33189,#33190,#33191,#33192,#33193,#33194,#33195,
#33196,#33197,#33198,#33199,#33200,#33201,#33202,#33203,#33204,#33205,#33206,
#33207,#33208,#33209,#33210,#33211,#33212,#33213,#33214,#33215,#33216,#33217,
#33218,#33219,#33220,#33221,#33222,#33223,#33224,#33225,#33226,#33227,#33228,
#33229,#33230,#33231,#33232,#33233,#33234,#33235,#33236,#33237,#33238,#33239,
#33240,#33241,#33242,#33243,#33244,#33245,#33246,#33247,#33248,#33249,#33250,
#33251,#33252,#33253,#33254,#33255,#33256,#33257,#33258,#33259,#33260,#33261,
#33262,#33263,#33264,#33265,#33266,#33267,#33268,#33269,#33270,#33271,#33272,
#33273,#33274,#33275,#33276,#33277,#33278,#33279,#33280,#33281,#33282,#33283,
#33284,#33285,#33286,#33287,#33288,#33289,#33290,#33291,#33292,#33293,#33294,
#33295,#33296,#33297,#33298,#33299,#33300,#33301,#33302,#33303,#33304,#33305,
#33306,#33307,#33308,#33309,#33310,#33311,#33312,#33313,#33314,#33315,#33316,
#33317,#33318,#33319,#33320,#33321,#33322,#33323,#33324,#33325,#33326,#33327,
#33328,#33329,#33330,#33331,#33332,#33333,#33334),.UNSPECIFIED.,.F.,.F.,
(4,3,3,3,3,3,3,3,3,3,3,3,3,3,3,3,3,3,3,3,3,3,3,3,3,3,3,3,3,3,3,3,3,3,3,
3,3,3,3,3,3,3,3,3,3,3,3,3,3,3,3,3,3,3,3,4),(317.300858012671,317.377039648526,
317.453155161215,317.529221117743,317.605261090874,317.681288920083,317.757319530207,
317.833367846566,317.909490964028,317.985652971468,318.06192404716,318.126291319451,
318.203821437514,318.281264466831,318.358636048656,318.435951773016,318.513227189577,
318.590488065603,318.667743376949,318.745007165041,318.822293473425,318.899660335031,
318.977068728963,319.054590361835,319.124699327502,319.201535359625,319.278282375352,
319.354956612915,319.431574252437,319.508151429064,319.585020917376,319.661581019898,
319.738151317046,319.814746378068,319.891836617439,319.968563814021,320.045835574787,
320.123107335553,320.200702004987,320.278204271098,320.355629756168,320.432994027545,
320.510312608635,320.587608313107,320.664893357763,320.742181749696,320.819487495222,
320.896865535209,320.974280606954,321.051801221225,321.121515343604,321.203013892014,
321.28671011981,321.367969374234,321.452884088717,321.537798803201),
 .UNSPECIFIED.);
#307=B_SPLINE_CURVE_WITH_KNOTS('',3,(#33340,#33341,#33342,#33343,#33344,
#33345,#33346,#33347,#33348,#33349,#33350,#33351,#33352,#33353,#33354,#33355,
#33356,#33357,#33358,#33359,#33360,#33361,#33362,#33363,#33364,#33365,#33366,
#33367,#33368,#33369,#33370,#33371,#33372,#33373,#33374,#33375,#33376,#33377,
#33378,#33379,#33380,#33381,#33382,#33383,#33384,#33385,#33386,#33387,#33388,
#33389,#33390,#33391,#33392,#33393,#33394,#33395,#33396,#33397,#33398,#33399,
#33400,#33401,#33402,#33403,#33404,#33405,#33406,#33407,#33408,#33409,#33410,
#33411,#33412,#33413,#33414,#33415,#33416,#33417,#33418,#33419,#33420,#33421,
#33422,#33423,#33424,#33425,#33426,#33427,#33428,#33429,#33430,#33431,#33432,
#33433,#33434,#33435,#33436,#33437,#33438,#33439,#33440,#33441,#33442,#33443,
#33444,#33445,#33446,#33447,#33448,#33449,#33450,#33451,#33452,#33453,#33454,
#33455,#33456,#33457,#33458,#33459,#33460,#33461,#33462,#33463,#33464,#33465,
#33466,#33467,#33468,#33469,#33470,#33471,#33472,#33473,#33474,#33475,#33476,
#33477,#33478,#33479,#33480,#33481,#33482,#33483,#33484,#33485,#33486,#33487,
#33488,#33489,#33490,#33491,#33492,#33493,#33494,#33495,#33496,#33497,#33498,
#33499,#33500,#33501,#33502,#33503,#33504,#33505,#33506,#33507,#33508,#33509,
#33510,#33511),.UNSPECIFIED.,.F.,.F.,(4,3,3,3,3,3,3,3,3,3,3,3,3,3,3,3,3,
3,3,3,3,3,3,3,3,3,3,3,3,3,3,3,3,3,3,3,3,3,3,3,3,3,3,3,3,3,3,3,3,3,3,3,3,
3,3,3,3,4),(323.584043319749,323.663946710699,323.741728431509,323.819526019224,
323.897352847792,323.978832247681,324.056801261427,324.134828908685,324.212963354016,
324.223270447347,324.300091644502,324.376823606716,324.453482584864,324.530084771325,
324.606646313206,324.683693531395,324.76023770604,324.836791986085,324.913370951065,
324.990784227978,325.067495708285,325.145259883501,325.223024058717,325.300606682331,
325.37809666454,325.455509641765,325.532861195267,325.610166862178,325.687449455223,
325.764721242167,325.841996242024,325.919288472962,325.996653145327,326.074054753759,
326.151562568367,326.222777670086,326.304261643041,326.385641007181,326.469894374328,
326.5510478695,326.632124547458,326.713109975248,326.722654475771,326.803662871675,
326.884747128507,326.969193166744,327.050499248452,327.13188303822,327.213387699248,
327.222531281455,327.300038871417,327.377469344525,327.454836829461,327.532155415822,
327.609442145055,327.686709244247,327.763985749949,327.820383538779),
 .UNSPECIFIED.);
#308=B_SPLINE_CURVE_WITH_KNOTS('',3,(#33512,#33513,#33514,#33515,#33516,
#33517,#33518,#33519,#33520,#33521,#33522,#33523,#33524,#33525,#33526,#33527,
#33528,#33529,#33530,#33531,#33532,#33533,#33534,#33535,#33536,#33537,#33538,
#33539,#33540,#33541,#33542,#33543,#33544,#33545,#33546,#33547,#33548,#33549,
#33550,#33551,#33552,#33553,#33554,#33555,#33556,#33557,#33558,#33559,#33560,
#33561,#33562,#33563,#33564,#33565,#33566,#33567,#33568,#33569,#33570,#33571,
#33572,#33573,#33574,#33575,#33576,#33577,#33578,#33579,#33580,#33581,#33582,
#33583,#33584,#33585,#33586,#33587,#33588,#33589,#33590),.UNSPECIFIED.,
 .F.,.F.,(4,3,3,3,3,3,3,3,3,3,3,3,3,3,3,3,3,3,3,3,3,3,3,3,3,3,4),(321.538270899783,
321.614838307952,321.691388010917,321.767930365409,321.844479946831,321.921051332763,
321.997704444672,322.074399352265,322.151211241319,322.223763224608,322.301280776226,
322.378710995646,322.456069538541,322.533372009128,322.610633971078,322.68788119686,
322.765122708068,322.8423725583,322.919644803214,322.996997761185,323.074392153494,
323.151900481162,323.223516835978,323.313648456897,323.401631282329,323.492837300992,
323.584043319654),.UNSPECIFIED.);
#309=B_SPLINE_CURVE_WITH_KNOTS('',3,(#33592,#33593,#33594,#33595,#33596,
#33597,#33598,#33599,#33600,#33601,#33602,#33603,#33604,#33605,#33606,#33607,
#33608,#33609,#33610,#33611,#33612,#33613,#33614,#33615,#33616,#33617,#33618,
#33619,#33620,#33621,#33622,#33623,#33624,#33625,#33626,#33627,#33628,#33629,
#33630,#33631,#33632,#33633,#33634,#33635,#33636,#33637,#33638,#33639,#33640,
#33641,#33642,#33643,#33644,#33645,#33646,#33647,#33648,#33649,#33650,#33651,
#33652,#33653,#33654,#33655,#33656,#33657,#33658,#33659,#33660,#33661,#33662,
#33663,#33664,#33665,#33666,#33667,#33668,#33669,#33670,#33671,#33672,#33673),
 .UNSPECIFIED.,.F.,.F.,(4,3,3,3,3,3,3,3,3,3,3,3,3,3,3,3,3,3,3,3,3,3,3,3,
3,3,3,4),(321.537798803201,321.620719347629,321.701732453919,321.782821148193,
321.867096699058,321.948406165448,322.029793066659,322.111300205424,322.119923351655,
322.197451504864,322.274898379826,322.352279558533,322.429610575994,322.506906930824,
322.584197231161,322.661487138899,322.738790660897,322.816121809025,322.893541298846,
322.971006657268,323.048592043566,323.118331359706,323.200496339367,323.28250033732,
323.364275949166,323.44591614499,323.527362179731,323.584043319749),
 .UNSPECIFIED.);
#310=B_SPLINE_CURVE_WITH_KNOTS('',3,(#33674,#33675,#33676,#33677,#33678,
#33679,#33680,#33681,#33682,#33683,#33684,#33685,#33686,#33687,#33688,#33689,
#33690,#33691,#33692,#33693,#33694,#33695,#33696,#33697,#33698,#33699,#33700,
#33701,#33702,#33703,#33704,#33705,#33706,#33707,#33708,#33709,#33710,#33711,
#33712,#33713,#33714,#33715,#33716,#33717,#33718,#33719,#33720,#33721,#33722,
#33723,#33724,#33725,#33726,#33727,#33728,#33729,#33730,#33731,#33732,#33733,
#33734,#33735,#33736,#33737,#33738,#33739,#33740,#33741,#33742,#33743,#33744,
#33745,#33746,#33747,#33748,#33749,#33750,#33751,#33752,#33753,#33754,#33755,
#33756,#33757,#33758,#33759,#33760,#33761,#33762,#33763,#33764,#33765,#33766,
#33767,#33768,#33769,#33770,#33771,#33772,#33773,#33774,#33775,#33776,#33777,
#33778,#33779,#33780,#33781,#33782,#33783,#33784,#33785,#33786,#33787,#33788,
#33789,#33790,#33791,#33792,#33793,#33794,#33795,#33796,#33797,#33798,#33799,
#33800,#33801,#33802,#33803,#33804,#33805,#33806,#33807,#33808,#33809,#33810,
#33811,#33812,#33813,#33814,#33815,#33816,#33817,#33818,#33819,#33820,#33821,
#33822,#33823,#33824,#33825,#33826,#33827,#33828,#33829,#33830),
 .UNSPECIFIED.,.F.,.F.,(4,3,3,3,3,3,3,3,3,3,3,3,3,3,3,3,3,3,3,3,3,3,3,3,
3,3,3,3,3,3,3,3,3,3,3,3,3,3,3,3,3,3,3,3,3,3,3,3,3,3,3,3,4),(323.584043319749,
323.666505525785,323.748967383525,323.831428899819,323.913890081516,323.996350935467,
324.078811468522,324.161271687528,324.243731599336,324.326191210794,324.40865052875,
324.491109560052,324.573568311549,324.656026790088,324.738485002515,324.82094295568,
324.903400656427,324.985858111605,325.06831532806,325.154327554562,325.237651898985,
325.320118504431,325.402584265672,325.485049210125,325.567513365201,325.649976758309,
325.732439416858,325.814901368251,325.89736263989,325.979823259174,326.062283253501,
326.144742650265,326.22720147686,326.309659760677,326.392117529104,326.47457480953,
326.558708044941,326.641174043033,326.723638419388,326.80610128365,326.888562745441,
326.971022914362,327.053481899998,327.135939811915,327.22153565744,327.30400039404,
327.386462166042,327.468921411884,327.551378569861,327.633841088142,327.716298758997,
327.798757548948,327.820706576114),.UNSPECIFIED.);
#311=B_SPLINE_CURVE_WITH_KNOTS('',3,(#33836,#33837,#33838,#33839,#33840,
#33841,#33842,#33843,#33844,#33845,#33846,#33847,#33848,#33849,#33850,#33851,
#33852,#33853,#33854,#33855,#33856,#33857,#33858,#33859,#33860,#33861,#33862,
#33863,#33864,#33865,#33866,#33867,#33868,#33869,#33870,#33871,#33872,#33873,
#33874,#33875,#33876,#33877,#33878,#33879,#33880,#33881,#33882,#33883,#33884,
#33885,#33886,#33887,#33888,#33889,#33890,#33891,#33892,#33893,#33894,#33895,
#33896,#33897,#33898,#33899,#33900,#33901,#33902,#33903,#33904,#33905,#33906,
#33907,#33908,#33909,#33910,#33911,#33912,#33913,#33914,#33915,#33916,#33917,
#33918,#33919,#33920,#33921,#33922,#33923,#33924,#33925,#33926,#33927,#33928,
#33929,#33930,#33931,#33932,#33933,#33934,#33935,#33936,#33937,#33938,#33939,
#33940,#33941,#33942,#33943,#33944,#33945,#33946,#33947,#33948,#33949,#33950,
#33951,#33952,#33953,#33954,#33955,#33956,#33957,#33958,#33959,#33960,#33961,
#33962,#33963,#33964,#33965,#33966,#33967,#33968,#33969,#33970,#33971,#33972,
#33973,#33974,#33975,#33976,#33977,#33978,#33979,#33980,#33981,#33982,#33983,
#33984,#33985,#33986,#33987,#33988,#33989,#33990,#33991,#33992,#33993,#33994,
#33995,#33996,#33997,#33998,#33999,#34000,#34001),.UNSPECIFIED.,.F.,.F.,
(4,3,3,3,3,3,3,3,3,3,3,3,3,3,3,3,3,3,3,3,3,3,3,3,3,3,3,3,3,3,3,3,3,3,3,
3,3,3,3,3,3,3,3,3,3,3,3,3,3,3,3,3,3,3,3,4),(329.867228627023,329.955869499158,
330.044072983203,330.132932549383,330.221792115563,330.299309484759,330.37673955221,
330.45409797348,330.531400352695,330.608662253457,330.685909464148,330.763150988367,
330.840400879713,330.917673193857,330.995026265082,331.072420794834,331.149929299796,
331.221545726933,331.298366924088,331.375098886302,331.45175786445,331.528360050912,
331.604921592793,331.681968810981,331.758512985626,331.835067265671,331.911646230651,
331.989059507564,332.065770987871,332.143535163086,332.221299338302,332.298881961916,
332.376371944125,332.45378492135,332.531136474851,332.608442141762,332.685724734807,
332.762996521751,332.840271521607,332.917563752545,332.99492842491,333.072330033342,
333.149837847951,333.221052949672,333.302536922627,333.383916286767,333.468169653915,
333.549323149086,333.630399827046,333.711385254836,333.720929755356,333.801918491159,
333.883036778197,333.964221658522,334.045533951161,334.10356649952),
 .UNSPECIFIED.);
#312=B_SPLINE_CURVE_WITH_KNOTS('',3,(#34002,#34003,#34004,#34005,#34006,
#34007,#34008,#34009,#34010,#34011,#34012,#34013,#34014,#34015,#34016,#34017,
#34018,#34019,#34020,#34021,#34022,#34023,#34024,#34025,#34026,#34027,#34028,
#34029,#34030,#34031,#34032,#34033,#34034,#34035,#34036,#34037,#34038,#34039,
#34040,#34041,#34042,#34043,#34044,#34045,#34046,#34047,#34048,#34049,#34050,
#34051,#34052,#34053,#34054,#34055,#34056,#34057,#34058,#34059,#34060,#34061,
#34062,#34063,#34064,#34065,#34066,#34067,#34068,#34069,#34070,#34071,#34072,
#34073,#34074,#34075,#34076,#34077,#34078,#34079,#34080,#34081,#34082,#34083,
#34084,#34085,#34086),.UNSPECIFIED.,.F.,.F.,(4,3,3,3,3,3,3,3,3,3,3,3,3,
3,3,3,3,3,3,3,3,3,3,3,3,3,3,3,4),(327.820383538779,327.897692338465,327.978840477055,
328.056281233109,328.13377762746,328.211378106877,328.222284892825,328.299133516012,
328.375888362409,328.452565701814,328.529181741589,328.605752640213,328.682788373211,
328.759330791917,328.835879128479,328.912447959927,328.989845595994,329.066536676947,
329.14428759057,329.222038504194,329.302687269536,329.380591352408,329.458420870289,
329.536189422896,329.613910572277,329.691598450072,329.769267328952,329.846937730223,
329.867228626929),.UNSPECIFIED.);
#313=B_SPLINE_CURVE_WITH_KNOTS('',3,(#34088,#34089,#34090,#34091,#34092,
#34093,#34094,#34095,#34096,#34097,#34098,#34099,#34100,#34101,#34102,#34103,
#34104,#34105,#34106,#34107,#34108,#34109,#34110,#34111,#34112,#34113,#34114,
#34115,#34116,#34117,#34118,#34119,#34120,#34121,#34122,#34123,#34124,#34125,
#34126,#34127,#34128,#34129,#34130,#34131,#34132,#34133,#34134,#34135,#34136,
#34137,#34138,#34139,#34140,#34141,#34142,#34143,#34144,#34145,#34146,#34147,
#34148,#34149,#34150,#34151,#34152,#34153,#34154,#34155,#34156,#34157,#34158,
#34159,#34160,#34161,#34162,#34163),.UNSPECIFIED.,.F.,.F.,(4,3,3,3,3,3,
3,3,3,3,3,3,3,3,3,3,3,3,3,3,3,3,3,3,3,4),(327.820706576114,327.903168179967,
327.985629117938,328.068089417424,328.15054910582,328.233008210523,328.315466758922,
328.397924778408,328.48038229637,328.56706019203,328.649526977865,328.731992091209,
328.814455641714,328.896917739012,328.979378492713,329.06183801241,329.144296407678,
329.226753788075,329.309220174342,329.391683376355,329.474143832636,329.556601981547,
329.639067586426,329.72152746564,329.803991579004,329.867228626929),
 .UNSPECIFIED.);
#314=B_SPLINE_CURVE_WITH_KNOTS('',3,(#34164,#34165,#34166,#34167,#34168,
#34169,#34170,#34171,#34172,#34173,#34174,#34175,#34176,#34177,#34178,#34179,
#34180,#34181,#34182,#34183,#34184,#34185,#34186,#34187,#34188,#34189,#34190,
#34191,#34192,#34193,#34194,#34195,#34196,#34197,#34198,#34199,#34200,#34201,
#34202,#34203,#34204,#34205,#34206,#34207,#34208,#34209,#34210,#34211,#34212,
#34213,#34214,#34215,#34216,#34217,#34218,#34219,#34220,#34221,#34222,#34223,
#34224,#34225,#34226,#34227,#34228,#34229,#34230,#34231,#34232,#34233,#34234,
#34235,#34236,#34237,#34238,#34239,#34240,#34241,#34242,#34243,#34244,#34245,
#34246,#34247,#34248,#34249,#34250,#34251,#34252,#34253,#34254,#34255,#34256,
#34257,#34258,#34259,#34260,#34261,#34262,#34263,#34264,#34265,#34266,#34267,
#34268,#34269,#34270,#34271,#34272,#34273,#34274,#34275,#34276,#34277,#34278,
#34279,#34280,#34281,#34282,#34283,#34284,#34285,#34286,#34287,#34288,#34289,
#34290,#34291,#34292,#34293,#34294,#34295,#34296,#34297,#34298,#34299,#34300,
#34301,#34302,#34303,#34304,#34305,#34306,#34307,#34308,#34309,#34310,#34311,
#34312,#34313,#34314,#34315,#34316,#34317,#34318,#34319,#34320,#34321,#34322,
#34323,#34324,#34325,#34326,#34327,#34328,#34329,#34330,#34331,#34332),
 .UNSPECIFIED.,.F.,.F.,(4,3,3,3,3,3,3,3,3,3,3,3,3,3,3,3,3,3,3,3,3,3,3,3,
3,3,3,3,3,3,3,3,3,3,3,3,3,3,3,3,3,3,3,3,3,3,3,3,3,3,3,3,3,3,3,3,4),(329.867228626929,
329.972215293944,330.081178832984,330.107187416062,330.184050800714,330.260820632524,
330.337513168512,330.414144603679,330.490731084463,330.567589126919,330.644147449882,
330.720711784555,330.797296697682,330.87437137929,330.951078200159,331.028336812136,
331.105595424113,331.183125620573,331.260568715178,331.337940349234,331.415256112803,
331.492531555581,331.569792438001,331.647047743645,331.724311513939,331.801597792424,
331.878964605216,331.956372939923,332.033894496486,332.104003432164,332.181533550227,
332.258976579543,332.336348161369,332.413663885729,332.49093930229,332.568200178315,
332.645455489662,332.722719277753,332.800005586137,332.877372447744,332.954780841676,
333.032302474548,333.102411440215,333.179247472338,333.255994488065,333.332668725628,
333.40928636515,333.485863541777,333.562733030088,333.639293132611,333.715863429758,
333.79245849078,333.869548730152,333.946275926733,334.0235476875,334.100819448266,
334.103694651294),.UNSPECIFIED.);
#315=B_SPLINE_CURVE_WITH_KNOTS('',3,(#34338,#34339,#34340,#34341,#34342,
#34343,#34344,#34345,#34346,#34347,#34348,#34349,#34350,#34351,#34352,#34353,
#34354,#34355,#34356,#34357,#34358,#34359,#34360,#34361,#34362,#34363,#34364,
#34365,#34366,#34367,#34368,#34369,#34370,#34371,#34372,#34373,#34374,#34375,
#34376,#34377,#34378,#34379,#34380,#34381,#34382,#34383,#34384,#34385,#34386,
#34387,#34388,#34389,#34390,#34391,#34392,#34393,#34394,#34395,#34396,#34397,
#34398,#34399,#34400,#34401,#34402,#34403,#34404,#34405,#34406,#34407,#34408,
#34409,#34410,#34411,#34412,#34413,#34414,#34415,#34416,#34417,#34418,#34419,
#34420,#34421,#34422,#34423,#34424,#34425,#34426,#34427,#34428,#34429,#34430,
#34431,#34432,#34433,#34434,#34435,#34436,#34437,#34438,#34439,#34440,#34441,
#34442,#34443,#34444,#34445,#34446,#34447,#34448,#34449,#34450,#34451,#34452,
#34453,#34454,#34455,#34456,#34457,#34458,#34459,#34460,#34461,#34462,#34463,
#34464,#34465,#34466,#34467,#34468,#34469,#34470,#34471,#34472,#34473,#34474,
#34475,#34476,#34477,#34478,#34479,#34480,#34481,#34482,#34483,#34484,#34485,
#34486,#34487,#34488,#34489,#34490,#34491,#34492,#34493,#34494),
 .UNSPECIFIED.,.F.,.F.,(4,3,3,3,3,3,3,3,3,3,3,3,3,3,3,3,3,3,3,3,3,3,3,3,
3,3,3,3,3,3,3,3,3,3,3,3,3,3,3,3,3,3,3,3,3,3,3,3,3,3,3,3,4),(336.150413934108,
336.232876140144,336.315337997884,336.397799514178,336.480260695875,336.562721549826,
336.645182082881,336.727642301887,336.810102213695,336.892561825153,336.975021143109,
337.057480174411,337.139938925907,337.222397404446,337.304855616874,337.387313570038,
337.469771270786,337.552228725964,337.634685942418,337.72069816892,337.804022513344,
337.886489118789,337.96895488003,338.051419824483,338.133883979559,338.216347372668,
338.298810031216,338.381271982609,338.463733254248,338.546193873532,338.628653867859,
338.711113264623,338.793572091218,338.876030375035,338.958488143463,339.040945423888,
339.125078659299,339.207544657391,339.290009033747,339.372471898009,339.454933359799,
339.537393528721,339.619852514356,339.702310426273,339.787906271798,339.870371008398,
339.9528327804,340.035292026242,340.11774918422,340.200211702501,340.282669373356,
340.365128163307,340.387077190473),.UNSPECIFIED.);
#316=B_SPLINE_CURVE_WITH_KNOTS('',3,(#34495,#34496,#34497,#34498,#34499,
#34500,#34501,#34502,#34503,#34504,#34505,#34506,#34507,#34508,#34509,#34510,
#34511,#34512,#34513,#34514,#34515,#34516,#34517,#34518,#34519,#34520,#34521,
#34522,#34523,#34524,#34525,#34526,#34527,#34528,#34529,#34530,#34531,#34532,
#34533,#34534,#34535,#34536,#34537,#34538,#34539,#34540,#34541,#34542,#34543,
#34544,#34545,#34546,#34547,#34548,#34549,#34550,#34551,#34552,#34553,#34554,
#34555,#34556,#34557,#34558,#34559,#34560,#34561,#34562,#34563,#34564,#34565,
#34566,#34567,#34568,#34569,#34570,#34571,#34572,#34573,#34574,#34575,#34576,
#34577,#34578,#34579),.UNSPECIFIED.,.F.,.F.,(4,3,3,3,3,3,3,3,3,3,3,3,3,
3,3,3,3,3,3,3,3,3,3,3,3,3,3,3,4),(334.10356649952,334.185054976864,334.220806561041,
334.298322339304,334.375756639715,334.453125058142,334.530443143292,334.607726407336,
334.685003491648,334.762280072136,334.839570167533,334.916887801538,334.994294007862,
335.071746017176,335.149318825498,335.22056017241,335.29665931971,335.372665757179,
335.44859625978,335.5244675252,335.602643271341,335.678454145347,335.754259719948,
335.830074999942,335.90591499605,335.981830549012,336.057791521109,336.133846841639,
336.149873494327),.UNSPECIFIED.);
#317=B_SPLINE_CURVE_WITH_KNOTS('',3,(#34581,#34582,#34583,#34584,#34585,
#34586,#34587,#34588,#34589,#34590,#34591,#34592,#34593,#34594,#34595,#34596,
#34597,#34598,#34599,#34600,#34601,#34602,#34603,#34604,#34605,#34606,#34607,
#34608,#34609,#34610,#34611,#34612,#34613,#34614,#34615,#34616,#34617,#34618,
#34619,#34620,#34621,#34622,#34623,#34624,#34625,#34626,#34627,#34628,#34629,
#34630,#34631,#34632,#34633,#34634,#34635,#34636,#34637,#34638,#34639,#34640,
#34641,#34642,#34643,#34644,#34645,#34646,#34647,#34648,#34649,#34650,#34651,
#34652,#34653,#34654,#34655,#34656,#34657,#34658,#34659,#34660,#34661,#34662,
#34663,#34664,#34665),.UNSPECIFIED.,.F.,.F.,(4,3,3,3,3,3,3,3,3,3,3,3,3,
3,3,3,3,3,3,3,3,3,3,3,3,3,3,3,4),(334.103694651294,334.181285619702,334.258784764403,
334.33620770544,334.413570008341,334.490887195091,334.568182255047,334.645467173949,
334.722755958722,334.800062615803,334.87744180169,334.954858485744,335.032379990469,
335.099227456317,335.18071377075,335.262095853109,335.346179754917,335.42733707377,
335.508417857525,335.589407849559,335.598431460342,335.679444566632,335.760533260905,
335.84480881177,335.92611827816,336.00750517937,336.089012318135,336.097635464367,
336.150413934108),.UNSPECIFIED.);
#318=B_SPLINE_CURVE_WITH_KNOTS('',3,(#34666,#34667,#34668,#34669,#34670,
#34671,#34672,#34673,#34674,#34675,#34676,#34677,#34678,#34679,#34680,#34681,
#34682,#34683,#34684,#34685,#34686,#34687,#34688,#34689,#34690,#34691,#34692,
#34693,#34694,#34695,#34696,#34697,#34698,#34699,#34700,#34701,#34702,#34703,
#34704,#34705,#34706,#34707,#34708,#34709,#34710,#34711,#34712,#34713,#34714,
#34715,#34716,#34717,#34718,#34719,#34720,#34721,#34722,#34723,#34724,#34725,
#34726,#34727,#34728,#34729,#34730,#34731,#34732,#34733,#34734,#34735,#34736,
#34737,#34738,#34739,#34740,#34741,#34742,#34743,#34744,#34745,#34746,#34747,
#34748,#34749,#34750,#34751,#34752,#34753,#34754,#34755,#34756,#34757,#34758,
#34759,#34760,#34761,#34762,#34763,#34764,#34765,#34766,#34767,#34768,#34769,
#34770,#34771,#34772,#34773,#34774,#34775,#34776,#34777,#34778,#34779,#34780,
#34781,#34782,#34783,#34784,#34785,#34786,#34787,#34788,#34789,#34790,#34791,
#34792,#34793,#34794,#34795,#34796,#34797,#34798,#34799,#34800,#34801,#34802,
#34803,#34804,#34805,#34806,#34807,#34808,#34809,#34810,#34811,#34812,#34813,
#34814,#34815,#34816,#34817,#34818,#34819,#34820,#34821,#34822,#34823,#34824,
#34825,#34826,#34827,#34828,#34829,#34830,#34831,#34832,#34833,#34834),
 .UNSPECIFIED.,.F.,.F.,(4,3,3,3,3,3,3,3,3,3,3,3,3,3,3,3,3,3,3,3,3,3,3,3,
3,3,3,3,3,3,3,3,3,3,3,3,3,3,3,3,3,3,3,3,3,3,3,3,3,3,3,3,3,3,3,3,4),(336.150413934201,
336.227400235554,336.304308354968,336.381154357483,336.457954260505,336.537715411994,
336.61448474228,336.69125925539,336.768053400328,336.844881635197,336.921798512557,
336.998767926114,337.075842526394,337.096043472418,337.17290685707,337.24967668888,
337.326369224869,337.403000660035,337.479587140819,337.556445183275,337.633003506238,
337.709567840911,337.786152754038,337.863227435646,337.939934256515,338.017192868492,
338.094451480469,338.171981676929,338.249424771534,338.32679640559,338.404112169159,
338.481387611937,338.558648494356,338.635903800001,338.713167570295,338.790453848779,
338.867820661571,338.945228996279,339.022750552842,339.09285948852,339.170389606583,
339.247832635899,339.325204217725,339.402519942085,339.479795358647,339.557056234672,
339.634311546018,339.71157533411,339.788861642495,339.866228504101,339.943636898033,
340.021158530905,340.091267496571,340.168094604426,340.244843419813,340.321511037319,
340.387601338952),.UNSPECIFIED.);
#319=B_SPLINE_CURVE_WITH_KNOTS('',3,(#34840,#34841,#34842,#34843,#34844,
#34845,#34846,#34847,#34848,#34849,#34850,#34851,#34852,#34853,#34854,#34855,
#34856,#34857,#34858,#34859,#34860,#34861,#34862,#34863,#34864,#34865,#34866,
#34867,#34868,#34869,#34870,#34871,#34872,#34873,#34874,#34875,#34876,#34877,
#34878,#34879,#34880,#34881,#34882,#34883,#34884,#34885,#34886,#34887,#34888,
#34889,#34890,#34891,#34892,#34893,#34894,#34895,#34896,#34897,#34898,#34899,
#34900,#34901,#34902,#34903,#34904,#34905,#34906,#34907,#34908,#34909,#34910,
#34911,#34912,#34913,#34914,#34915,#34916,#34917,#34918,#34919,#34920,#34921,
#34922,#34923,#34924,#34925,#34926,#34927,#34928,#34929,#34930,#34931,#34932,
#34933,#34934,#34935,#34936,#34937,#34938,#34939,#34940,#34941,#34942,#34943,
#34944,#34945,#34946,#34947,#34948,#34949,#34950,#34951,#34952,#34953,#34954,
#34955,#34956,#34957,#34958,#34959,#34960,#34961,#34962,#34963,#34964,#34965,
#34966,#34967,#34968,#34969,#34970,#34971,#34972,#34973,#34974,#34975,#34976,
#34977,#34978,#34979,#34980,#34981,#34982,#34983,#34984,#34985,#34986,#34987,
#34988,#34989,#34990,#34991,#34992,#34993,#34994,#34995,#34996,#34997,#34998,
#34999,#35000,#35001,#35002,#35003,#35004,#35005,#35006,#35007,#35008),
 .UNSPECIFIED.,.F.,.F.,(4,3,3,3,3,3,3,3,3,3,3,3,3,3,3,3,3,3,3,3,3,3,3,3,
3,3,3,3,3,3,3,3,3,3,3,3,3,3,3,3,3,3,3,3,3,3,3,3,3,3,3,3,3,3,3,3,4),(342.434795335461,
342.510391140104,342.585928653286,342.665011204546,342.740491920252,342.815969007295,
342.891457617893,342.966972913604,343.042568927301,343.118212230254,343.193957241268,
343.218589063365,343.296106614983,343.373536834403,343.450895377298,343.528197847885,
343.605459809836,343.682707035618,343.759948546825,343.837198397058,343.914470641971,
343.991823599942,344.069217992251,344.146726319919,344.218342674735,344.295860043931,
344.373290111383,344.450648532652,344.527950911867,344.60521281263,344.682460023321,
344.75970154754,344.836951438886,344.914223753029,344.991576824255,345.068971354007,
345.146479858969,345.218096286104,345.294917483259,345.371649445473,345.448308423621,
345.524910610082,345.601472151963,345.678519370152,345.755063544796,345.831617824842,
345.908196789821,345.985610066734,346.062321547041,346.140085722257,346.217849897473,
346.295437931297,346.372936137223,346.450339998853,346.527689274207,346.604993913737,
346.67045654415),.UNSPECIFIED.);
#320=B_SPLINE_CURVE_WITH_KNOTS('',3,(#35009,#35010,#35011,#35012,#35013,
#35014,#35015,#35016,#35017,#35018,#35019,#35020,#35021,#35022,#35023,#35024,
#35025,#35026,#35027,#35028,#35029,#35030,#35031,#35032,#35033,#35034,#35035,
#35036,#35037,#35038,#35039,#35040,#35041,#35042,#35043,#35044,#35045,#35046,
#35047,#35048,#35049,#35050,#35051,#35052,#35053,#35054,#35055,#35056,#35057,
#35058,#35059,#35060,#35061,#35062,#35063,#35064,#35065,#35066,#35067,#35068,
#35069,#35070,#35071,#35072,#35073,#35074,#35075,#35076,#35077,#35078,#35079,
#35080,#35081,#35082,#35083,#35084),.UNSPECIFIED.,.F.,.F.,(4,3,3,3,3,3,
3,3,3,3,3,3,3,3,3,3,3,3,3,3,3,3,3,3,3,4),(340.387077190473,340.469538794326,
340.551999732297,340.634460031783,340.71691972018,340.799378824882,340.881837373281,
340.964295392767,341.046752910729,341.133430806389,341.215897592224,341.298362705568,
341.380826256073,341.463288353371,341.545749107072,341.628208626769,341.710667022037,
341.793124402434,341.8755907887,341.958053990714,342.040514446995,342.122972595905,
342.205438200785,342.287898079999,342.370362193363,342.433599241288),
 .UNSPECIFIED.);
#321=B_SPLINE_CURVE_WITH_KNOTS('',3,(#35086,#35087,#35088,#35089,#35090,
#35091,#35092,#35093,#35094,#35095,#35096,#35097,#35098,#35099,#35100,#35101,
#35102,#35103,#35104,#35105,#35106,#35107,#35108,#35109,#35110,#35111,#35112,
#35113,#35114,#35115,#35116,#35117,#35118,#35119,#35120,#35121,#35122,#35123,
#35124,#35125,#35126,#35127,#35128,#35129,#35130,#35131,#35132,#35133,#35134,
#35135,#35136,#35137,#35138,#35139,#35140,#35141,#35142,#35143,#35144,#35145,
#35146,#35147,#35148,#35149,#35150,#35151,#35152,#35153,#35154,#35155,#35156,
#35157,#35158,#35159,#35160,#35161,#35162,#35163,#35164),.UNSPECIFIED.,
 .F.,.F.,(4,3,3,3,3,3,3,3,3,3,3,3,3,3,3,3,3,3,3,3,3,3,3,3,3,3,4),(340.387601338952,
340.464183127824,340.542369674924,340.618929532378,340.69549783046,340.77208913748,
340.851485729266,340.92820838647,341.008941945546,341.089675504622,341.167270174056,
341.244772440167,341.322197925238,341.399562196615,341.476880777705,341.554176482177,
341.631461526833,341.708749918765,341.786055664291,341.863433704278,341.940848776023,
342.018369390294,342.088083512673,342.176003795807,342.263719859844,342.351021027598,
342.433599241288),.UNSPECIFIED.);
#322=B_SPLINE_CURVE_WITH_KNOTS('',3,(#35165,#35166,#35167,#35168,#35169,
#35170,#35171,#35172,#35173,#35174,#35175,#35176,#35177,#35178,#35179,#35180,
#35181,#35182,#35183,#35184,#35185,#35186,#35187,#35188,#35189,#35190,#35191,
#35192,#35193,#35194,#35195,#35196,#35197,#35198,#35199,#35200,#35201,#35202,
#35203,#35204,#35205,#35206,#35207,#35208,#35209,#35210,#35211,#35212,#35213,
#35214,#35215,#35216,#35217,#35218,#35219,#35220,#35221,#35222,#35223,#35224,
#35225,#35226,#35227,#35228,#35229,#35230,#35231,#35232,#35233,#35234,#35235,
#35236,#35237,#35238,#35239,#35240,#35241,#35242,#35243,#35244,#35245,#35246,
#35247,#35248,#35249,#35250,#35251,#35252,#35253,#35254,#35255,#35256,#35257,
#35258,#35259,#35260,#35261,#35262,#35263,#35264,#35265,#35266,#35267,#35268,
#35269,#35270,#35271,#35272,#35273,#35274,#35275,#35276,#35277,#35278,#35279,
#35280,#35281,#35282,#35283,#35284,#35285,#35286,#35287,#35288,#35289,#35290,
#35291,#35292,#35293,#35294,#35295,#35296,#35297,#35298,#35299,#35300,#35301,
#35302,#35303,#35304,#35305,#35306,#35307,#35308,#35309,#35310,#35311,#35312,
#35313,#35314,#35315,#35316,#35317,#35318,#35319,#35320,#35321),
 .UNSPECIFIED.,.F.,.F.,(4,3,3,3,3,3,3,3,3,3,3,3,3,3,3,3,3,3,3,3,3,3,3,3,
3,3,3,3,3,3,3,3,3,3,3,3,3,3,3,3,3,3,3,3,3,3,3,3,3,3,3,3,4),(342.433599241288,
342.516061447324,342.598523305064,342.680984821358,342.763446003055,342.845906857006,
342.928367390061,343.010827609067,343.093287520875,343.175747132333,343.258206450289,
343.340665481591,343.423124233088,343.505582711626,343.588040924054,343.670498877219,
343.752956577966,343.835414033144,343.917871249599,344.0038834761,344.087207820524,
344.169674425969,344.252140187211,344.334605131663,344.417069286739,344.499532679848,
344.581995338397,344.664457289789,344.746918561428,344.829379180712,344.911839175039,
344.994298571804,345.076757398399,345.159215682215,345.241673450643,345.324130731068,
345.40826396648,345.490729964571,345.573194340927,345.655657205189,345.73811866698,
345.820578835901,345.903037821536,345.985495733454,346.071091578978,346.153556315578,
346.23601808758,346.318477333422,346.4009344914,346.483397009681,346.565854680536,
346.648313470487,346.670262497652),.UNSPECIFIED.);
#323=B_SPLINE_CURVE_WITH_KNOTS('',3,(#35327,#35328,#35329,#35330,#35331,
#35332,#35333,#35334,#35335,#35336,#35337,#35338,#35339,#35340,#35341,#35342,
#35343,#35344,#35345,#35346,#35347,#35348,#35349,#35350,#35351,#35352,#35353,
#35354,#35355,#35356,#35357,#35358,#35359,#35360,#35361,#35362,#35363,#35364,
#35365,#35366,#35367,#35368,#35369,#35370,#35371,#35372,#35373,#35374,#35375,
#35376,#35377,#35378,#35379,#35380,#35381,#35382,#35383,#35384,#35385,#35386,
#35387,#35388,#35389,#35390,#35391,#35392,#35393,#35394,#35395,#35396,#35397,
#35398,#35399,#35400,#35401,#35402,#35403,#35404,#35405,#35406,#35407,#35408,
#35409,#35410,#35411,#35412,#35413,#35414,#35415,#35416,#35417,#35418,#35419,
#35420,#35421,#35422,#35423,#35424,#35425,#35426,#35427,#35428,#35429,#35430,
#35431,#35432,#35433,#35434,#35435,#35436,#35437,#35438,#35439,#35440,#35441,
#35442,#35443,#35444,#35445,#35446,#35447,#35448,#35449,#35450,#35451,#35452,
#35453,#35454,#35455,#35456,#35457,#35458,#35459,#35460,#35461,#35462,#35463,
#35464,#35465,#35466,#35467,#35468,#35469,#35470,#35471,#35472,#35473,#35474,
#35475,#35476,#35477,#35478,#35479,#35480,#35481,#35482,#35483,#35484,#35485,
#35486,#35487,#35488,#35489,#35490,#35491,#35492),.UNSPECIFIED.,.F.,.F.,
(4,3,3,3,3,3,3,3,3,3,3,3,3,3,3,3,3,3,3,3,3,3,3,3,3,3,3,3,3,3,3,3,3,3,3,
3,3,3,3,3,3,3,3,3,3,3,3,3,3,3,3,3,3,3,3,4),(348.71678454858,348.798749648545,
348.880854154498,348.964918298769,349.047377608491,349.132244170036,349.217110731581,
349.293959354768,349.370714201165,349.44739154057,349.524007580345,349.60057847897,
349.677614211967,349.754156630673,349.830704967236,349.907273798684,349.98467143475,
350.061362515703,350.139113429327,350.216864342951,350.294381894569,350.371812113989,
350.449170656884,350.526473127471,350.603735089421,350.680982315204,350.758223826411,
350.835473676644,350.912745921557,350.990098879528,351.067493271836,351.145001599505,
351.21661795432,351.294135323516,351.371565390967,351.448923812237,351.526226191452,
351.603488092215,351.680735302906,351.757976827124,351.83522671847,351.912499032614,
351.98985210384,352.067246633591,352.144755138553,352.216371565689,352.293207911534,
352.369951958647,352.446603917339,352.523203174201,352.599764352909,352.676302051195,
352.752847255585,352.829395570524,352.905987356481,352.952608162855),
 .UNSPECIFIED.);
#324=B_SPLINE_CURVE_WITH_KNOTS('',3,(#35493,#35494,#35495,#35496,#35497,
#35498,#35499,#35500,#35501,#35502,#35503,#35504,#35505,#35506,#35507,#35508,
#35509,#35510,#35511,#35512,#35513,#35514,#35515,#35516,#35517,#35518,#35519,
#35520,#35521,#35522,#35523,#35524,#35525,#35526,#35527,#35528,#35529,#35530,
#35531,#35532,#35533,#35534,#35535,#35536,#35537,#35538,#35539,#35540,#35541,
#35542,#35543,#35544,#35545,#35546,#35547,#35548,#35549,#35550,#35551,#35552,
#35553,#35554,#35555,#35556,#35557,#35558,#35559,#35560,#35561,#35562,#35563,
#35564,#35565,#35566,#35567,#35568,#35569,#35570,#35571,#35572,#35573,#35574,
#35575,#35576,#35577),.UNSPECIFIED.,.F.,.F.,(4,3,3,3,3,3,3,3,3,3,3,3,3,
3,3,3,3,3,3,3,3,3,3,3,3,3,3,3,4),(346.67045654415,346.747729075593,346.825002676091,
346.902291363443,346.981119399793,347.058515331763,347.138059420303,347.217603508843,
347.299087481798,347.380466845939,347.464720213086,347.545873708258,347.626950386218,
347.707935814007,347.717480314527,347.798488710431,347.879572967262,347.964019005499,
348.045325087206,348.126708876974,348.208213538003,348.217357120212,348.297778607236,
348.378089974019,348.458300350398,348.538389101135,348.618404721531,348.698337586771,
348.716784548467),.UNSPECIFIED.);
#325=B_SPLINE_CURVE_WITH_KNOTS('',3,(#35579,#35580,#35581,#35582,#35583,
#35584,#35585,#35586,#35587,#35588,#35589,#35590,#35591,#35592,#35593,#35594,
#35595,#35596,#35597,#35598,#35599,#35600,#35601,#35602,#35603,#35604,#35605,
#35606,#35607,#35608,#35609,#35610,#35611,#35612,#35613,#35614,#35615,#35616,
#35617,#35618,#35619,#35620,#35621,#35622,#35623,#35624,#35625,#35626,#35627,
#35628,#35629,#35630,#35631,#35632,#35633,#35634,#35635,#35636,#35637,#35638,
#35639,#35640,#35641,#35642,#35643,#35644,#35645,#35646,#35647,#35648,#35649,
#35650,#35651,#35652,#35653,#35654),.UNSPECIFIED.,.F.,.F.,(4,3,3,3,3,3,
3,3,3,3,3,3,3,3,3,3,3,3,3,3,3,3,3,3,3,4),(346.670262497652,346.752724101506,
346.835185039476,346.917645338962,347.000105027359,347.082564132061,347.16502268046,
347.247480699946,347.329938217908,347.416616113568,347.499082899404,347.581548012747,
347.664011563253,347.74647366055,347.828934414252,347.911393933949,347.993852329216,
348.076309709614,348.15877609588,348.241239297894,348.323699754174,348.406157903085,
348.488623507964,348.571083387179,348.653547500543,348.716784548467),
 .UNSPECIFIED.);
#326=B_SPLINE_CURVE_WITH_KNOTS('',3,(#35655,#35656,#35657,#35658,#35659,
#35660,#35661,#35662,#35663,#35664,#35665,#35666,#35667,#35668,#35669,#35670,
#35671,#35672,#35673,#35674,#35675,#35676,#35677,#35678,#35679,#35680,#35681,
#35682,#35683,#35684,#35685,#35686,#35687,#35688,#35689,#35690,#35691,#35692,
#35693,#35694,#35695,#35696,#35697,#35698,#35699,#35700,#35701,#35702,#35703,
#35704,#35705,#35706,#35707,#35708,#35709,#35710,#35711,#35712,#35713,#35714,
#35715,#35716,#35717,#35718,#35719,#35720,#35721,#35722,#35723,#35724,#35725,
#35726,#35727,#35728,#35729,#35730,#35731,#35732,#35733,#35734,#35735,#35736,
#35737,#35738,#35739,#35740,#35741,#35742,#35743,#35744,#35745,#35746,#35747,
#35748,#35749,#35750,#35751,#35752,#35753,#35754,#35755,#35756,#35757,#35758,
#35759,#35760,#35761,#35762,#35763,#35764,#35765,#35766,#35767,#35768,#35769,
#35770,#35771,#35772,#35773,#35774,#35775,#35776,#35777,#35778,#35779,#35780,
#35781,#35782,#35783,#35784,#35785,#35786,#35787,#35788,#35789,#35790,#35791,
#35792,#35793,#35794,#35795,#35796,#35797,#35798,#35799,#35800,#35801,#35802,
#35803,#35804,#35805,#35806,#35807,#35808,#35809,#35810,#35811,#35812,#35813,
#35814,#35815,#35816,#35817,#35818,#35819,#35820,#35821,#35822,#35823,#35824,
#35825,#35826),.UNSPECIFIED.,.F.,.F.,(4,3,3,3,3,3,3,3,3,3,3,3,3,3,3,3,3,
3,3,3,3,3,3,3,3,3,3,3,3,3,3,3,3,3,3,3,3,3,3,3,3,3,3,3,3,3,3,3,3,3,3,3,3,
3,3,3,3,4),(348.716784548467,348.806823303607,348.893179792152,348.979765980959,
349.06662943043,349.076939569029,349.158425883462,349.239807965821,349.323891867629,
349.405049186482,349.486129970237,349.56711996227,349.576143573055,349.657156679345,
349.738245373618,349.822520924484,349.903830390873,349.985217292084,350.066724430849,
350.07534757708,350.152875730289,350.23032260525,350.307703783958,350.385034801418,
350.462331156249,350.539621456585,350.616911364323,350.694214886321,350.771546034448,
350.848965524269,350.926430882691,351.004016268989,351.073755585131,351.150618969783,
351.227388801593,351.304081337581,351.380712772748,351.457299253532,351.534157295988,
351.610715618951,351.687279953624,351.763864866751,351.840939548359,351.917646369228,
351.994904981205,352.072163593182,352.149700020288,352.227148045033,352.304523313686,
352.385577908728,352.462853150381,352.540107610983,352.617355336625,352.694610366867,
352.771914614152,352.84924762751,352.92665352286,352.952960074025),
 .UNSPECIFIED.);
#327=B_SPLINE_CURVE_WITH_KNOTS('',3,(#35832,#35833,#35834,#35835,#35836,
#35837,#35838,#35839,#35840,#35841,#35842,#35843,#35844,#35845,#35846,#35847,
#35848,#35849,#35850,#35851,#35852,#35853,#35854,#35855,#35856,#35857,#35858,
#35859,#35860,#35861,#35862,#35863,#35864,#35865,#35866,#35867,#35868,#35869,
#35870,#35871,#35872,#35873,#35874,#35875,#35876,#35877,#35878,#35879,#35880,
#35881,#35882,#35883,#35884,#35885,#35886,#35887,#35888,#35889,#35890,#35891,
#35892,#35893,#35894,#35895,#35896,#35897,#35898,#35899,#35900,#35901,#35902,
#35903,#35904,#35905,#35906,#35907,#35908,#35909,#35910,#35911,#35912,#35913,
#35914,#35915,#35916,#35917,#35918,#35919,#35920,#35921,#35922,#35923,#35924,
#35925,#35926,#35927,#35928,#35929,#35930,#35931,#35932,#35933,#35934,#35935,
#35936,#35937,#35938,#35939,#35940,#35941,#35942,#35943,#35944,#35945,#35946,
#35947,#35948,#35949,#35950,#35951,#35952,#35953,#35954,#35955,#35956,#35957,
#35958,#35959,#35960,#35961,#35962,#35963,#35964,#35965,#35966,#35967,#35968,
#35969,#35970,#35971,#35972,#35973,#35974,#35975,#35976,#35977,#35978,#35979,
#35980,#35981,#35982,#35983,#35984,#35985,#35986,#35987,#35988,#35989,#35990,
#35991,#35992,#35993,#35994,#35995,#35996,#35997,#35998,#35999,#36000),
 .UNSPECIFIED.,.F.,.F.,(4,3,3,3,3,3,3,3,3,3,3,3,3,3,3,3,3,3,3,3,3,3,3,3,
3,3,3,3,3,3,3,3,3,3,3,3,3,3,3,3,3,3,3,3,3,3,3,3,3,3,3,3,3,3,3,3,4),(354.999969855647,
355.099329048981,355.20011625081,355.215632399798,355.293148178061,355.370582478472,
355.447950896899,355.525268982049,355.602552246093,355.679829330405,355.757105910892,
355.83439600629,355.911713640294,355.989119846618,356.066571855932,356.144144664254,
356.215386011167,356.292234634354,356.368989480751,356.445666820156,356.522282859931,
356.598853758556,356.675889491553,356.752431910259,356.828980246821,356.905549078269,
356.982946714336,357.059637795289,357.137388708912,357.215139622536,357.292657174154,
357.370087393574,357.447445936469,357.524748407056,357.602010369007,357.679257594789,
357.756499105997,357.833748956229,357.911021201142,357.988374159113,358.065768551422,
358.143276879091,358.214893233906,358.292410603102,358.369840670553,358.447199091823,
358.524501471038,358.601763371801,358.679010582492,358.75625210671,358.833501998056,
358.9107743122,358.988127383426,359.065521913177,359.14303041814,359.214646845275,
359.236895376301),.UNSPECIFIED.);
#328=B_SPLINE_CURVE_WITH_KNOTS('',3,(#36001,#36002,#36003,#36004,#36005,
#36006,#36007,#36008,#36009,#36010,#36011,#36012,#36013,#36014,#36015,#36016,
#36017,#36018,#36019,#36020,#36021,#36022,#36023,#36024,#36025,#36026,#36027,
#36028,#36029,#36030,#36031,#36032,#36033,#36034,#36035,#36036,#36037,#36038,
#36039,#36040,#36041,#36042,#36043,#36044,#36045,#36046,#36047,#36048,#36049,
#36050,#36051,#36052,#36053,#36054,#36055,#36056,#36057,#36058,#36059,#36060,
#36061,#36062,#36063,#36064,#36065,#36066,#36067,#36068,#36069,#36070,#36071,
#36072,#36073,#36074,#36075,#36076,#36077,#36078,#36079,#36080,#36081,#36082,
#36083,#36084,#36085),.UNSPECIFIED.,.F.,.F.,(4,3,3,3,3,3,3,3,3,3,3,3,3,
3,3,3,3,3,3,3,3,3,3,3,3,3,3,3,4),(352.952608162855,353.029299967087,353.106043896697,
353.182899467382,353.216125177059,353.293707800673,353.371197782882,353.448610760107,
353.525962313608,353.60326798052,353.680550573564,353.757822360508,353.835097360365,
353.912389591303,353.989754263668,354.0671558721,354.144663686709,354.215878788428,
354.297362761383,354.378742125522,354.46299549267,354.544148987842,354.6252256658,
354.70621109359,354.715755594113,354.791007671957,354.866272417376,354.941602667642,
354.999969855565),.UNSPECIFIED.);
#329=B_SPLINE_CURVE_WITH_KNOTS('',3,(#36087,#36088,#36089,#36090,#36091,
#36092,#36093,#36094,#36095,#36096,#36097,#36098,#36099,#36100,#36101,#36102,
#36103,#36104,#36105,#36106,#36107,#36108,#36109,#36110,#36111,#36112,#36113,
#36114,#36115,#36116,#36117,#36118,#36119,#36120,#36121,#36122,#36123,#36124,
#36125,#36126,#36127,#36128,#36129,#36130,#36131,#36132,#36133,#36134,#36135,
#36136,#36137,#36138,#36139,#36140,#36141,#36142,#36143,#36144,#36145,#36146,
#36147,#36148,#36149,#36150,#36151,#36152,#36153,#36154,#36155,#36156,#36157,
#36158,#36159,#36160,#36161,#36162,#36163,#36164,#36165,#36166,#36167,#36168,
#36169,#36170,#36171),.UNSPECIFIED.,.F.,.F.,(4,3,3,3,3,3,3,3,3,3,3,3,3,
3,3,3,3,3,3,3,3,3,3,3,3,3,3,3,4),(352.952960074025,353.03049316836,353.070571601233,
353.148101719296,353.225544748612,353.302916330438,353.380232054798,353.457507471359,
353.534768347385,353.612023658731,353.689287446823,353.766573755207,353.843940616813,
353.921349010745,353.998870643617,354.068979609284,354.145073751402,354.2210795021,
354.297013600867,354.372892715455,354.451194742664,354.52702406611,354.602852026218,
354.678693617442,354.754563843074,354.830515470671,354.906515871729,354.982615653516,
354.999308933125),.UNSPECIFIED.);
#330=B_SPLINE_CURVE_WITH_KNOTS('',3,(#36172,#36173,#36174,#36175,#36176,
#36177,#36178,#36179,#36180,#36181,#36182,#36183,#36184,#36185,#36186,#36187,
#36188,#36189,#36190,#36191,#36192,#36193,#36194,#36195,#36196,#36197,#36198,
#36199,#36200,#36201,#36202,#36203,#36204,#36205,#36206,#36207,#36208,#36209,
#36210,#36211,#36212,#36213,#36214,#36215,#36216,#36217,#36218,#36219,#36220,
#36221,#36222,#36223,#36224,#36225,#36226,#36227,#36228,#36229,#36230,#36231,
#36232,#36233,#36234,#36235,#36236,#36237,#36238,#36239,#36240,#36241,#36242,
#36243,#36244,#36245,#36246,#36247,#36248,#36249,#36250,#36251,#36252,#36253,
#36254,#36255,#36256,#36257,#36258,#36259,#36260,#36261,#36262,#36263,#36264,
#36265,#36266,#36267,#36268,#36269,#36270,#36271,#36272,#36273,#36274,#36275,
#36276,#36277,#36278,#36279,#36280,#36281,#36282,#36283,#36284,#36285,#36286,
#36287,#36288,#36289,#36290,#36291,#36292,#36293,#36294,#36295,#36296,#36297,
#36298,#36299,#36300,#36301,#36302,#36303,#36304,#36305,#36306,#36307,#36308,
#36309,#36310,#36311,#36312,#36313,#36314,#36315,#36316,#36317,#36318,#36319,
#36320,#36321,#36322,#36323,#36324,#36325,#36326,#36327,#36328),
 .UNSPECIFIED.,.F.,.F.,(4,3,3,3,3,3,3,3,3,3,3,3,3,3,3,3,3,3,3,3,3,3,3,3,
3,3,3,3,3,3,3,3,3,3,3,3,3,3,3,3,3,3,3,3,3,3,3,3,3,3,3,3,4),(354.999969855647,
355.082432061683,355.164893919423,355.247355435717,355.329816617414,355.412277471365,
355.49473800442,355.577198223426,355.659658135234,355.742117746692,355.824577064648,
355.90703609595,355.989494847447,356.071953325985,356.154411538413,356.236869491577,
356.319327192325,356.401784647503,356.484241863957,356.570254090459,356.653578434882,
356.736045040328,356.818510801569,356.900975746022,356.983439901098,357.065903294207,
357.148365952755,357.230827904148,357.313289175787,357.395749795071,357.478209789398,
357.560669186162,357.643128012757,357.725586296574,357.808044065001,357.890501345427,
357.974634580838,358.05710057893,358.139564955285,358.222027819548,358.304489281338,
358.386949450259,358.469408435895,358.551866347812,358.637462193337,358.719926929937,
358.802388701939,358.884847947781,358.967305105758,359.049767624039,359.132225294894,
359.214684084845,359.236633112011),.UNSPECIFIED.);
#331=B_SPLINE_CURVE_WITH_KNOTS('',3,(#36334,#36335,#36336,#36337,#36338,
#36339,#36340,#36341,#36342,#36343,#36344,#36345,#36346,#36347,#36348,#36349,
#36350,#36351,#36352,#36353,#36354,#36355,#36356,#36357,#36358,#36359,#36360,
#36361,#36362,#36363,#36364,#36365,#36366,#36367,#36368,#36369,#36370,#36371,
#36372,#36373,#36374,#36375,#36376,#36377,#36378,#36379,#36380,#36381,#36382,
#36383,#36384,#36385,#36386,#36387,#36388,#36389,#36390,#36391,#36392,#36393,
#36394,#36395,#36396,#36397,#36398,#36399,#36400,#36401,#36402,#36403,#36404,
#36405,#36406,#36407,#36408,#36409,#36410,#36411,#36412,#36413,#36414,#36415,
#36416,#36417,#36418,#36419,#36420,#36421,#36422,#36423,#36424,#36425,#36426,
#36427,#36428,#36429,#36430,#36431,#36432,#36433,#36434,#36435,#36436,#36437,
#36438,#36439,#36440,#36441,#36442,#36443,#36444,#36445,#36446,#36447,#36448,
#36449,#36450,#36451,#36452,#36453,#36454,#36455,#36456,#36457,#36458,#36459,
#36460,#36461,#36462,#36463,#36464,#36465,#36466,#36467,#36468,#36469,#36470,
#36471,#36472,#36473,#36474,#36475,#36476,#36477,#36478,#36479,#36480,#36481,
#36482,#36483,#36484,#36485,#36486,#36487,#36488,#36489,#36490,#36491,#36492,
#36493,#36494,#36495,#36496,#36497,#36498,#36499,#36500,#36501,#36502),
 .UNSPECIFIED.,.F.,.F.,(4,3,3,3,3,3,3,3,3,3,3,3,3,3,3,3,3,3,3,3,3,3,3,3,
3,3,3,3,3,3,3,3,3,3,3,3,3,3,3,3,3,3,3,3,3,3,3,3,3,3,3,3,3,3,3,3,4),(361.283155162939,
361.361992357148,361.440737819558,361.519381858553,361.597966756718,361.676494051824,
361.714030873699,361.795039269603,361.876123526435,361.960569564672,362.041875646379,
362.123259436148,362.204764097177,362.213907679383,362.291423457646,362.368857758057,
362.446226176484,362.523544261634,362.600827525678,362.678104609989,362.755381190477,
362.832671285875,362.909988919879,362.987395126203,363.064847135517,363.142419943839,
363.213661290753,363.29050991394,363.367264760337,363.443942099742,363.520558139517,
363.597129038141,363.674164771139,363.750707189845,363.827255526407,363.903824357855,
363.981221993922,364.057913074875,364.135663988498,364.213414902122,364.29093245374,
364.36836267316,364.445721216055,364.523023686642,364.600285648592,364.677532874375,
364.754774385583,364.832024235815,364.909296480728,364.986649438699,365.064043831008,
365.141552158676,365.213168513491,365.290675335511,365.368105554801,365.445456107835,
365.520350523813),.UNSPECIFIED.);
#332=B_SPLINE_CURVE_WITH_KNOTS('',3,(#36503,#36504,#36505,#36506,#36507,
#36508,#36509,#36510,#36511,#36512,#36513,#36514,#36515,#36516,#36517,#36518,
#36519,#36520,#36521,#36522,#36523,#36524,#36525,#36526,#36527,#36528,#36529,
#36530,#36531,#36532,#36533,#36534,#36535,#36536,#36537,#36538,#36539,#36540,
#36541,#36542,#36543,#36544,#36545,#36546,#36547,#36548,#36549,#36550,#36551,
#36552,#36553,#36554,#36555,#36556,#36557,#36558,#36559,#36560,#36561,#36562,
#36563,#36564,#36565,#36566,#36567,#36568,#36569,#36570,#36571,#36572,#36573,
#36574,#36575,#36576,#36577,#36578,#36579,#36580,#36581,#36582,#36583,#36584),
 .UNSPECIFIED.,.F.,.F.,(4,3,3,3,3,3,3,3,3,3,3,3,3,3,3,3,3,3,3,3,3,3,3,3,
3,3,3,4),(359.236895376301,359.313689066245,359.390398232431,359.467039107372,
359.543627869032,359.620180653732,359.696726555118,359.773272110338,359.849831895196,
359.926420491938,360.003098426069,360.079824295919,360.156668757418,360.214400456644,
360.291983080258,360.369473062467,360.446886039692,360.524237593193,360.601543260104,
360.678825853149,360.756097640093,360.83337263995,360.910664870888,360.988029543253,
361.065431151685,361.142938966293,361.214154068014,361.283155162827),
 .UNSPECIFIED.);
#333=B_SPLINE_CURVE_WITH_KNOTS('',3,(#36586,#36587,#36588,#36589,#36590,
#36591,#36592,#36593,#36594,#36595,#36596,#36597,#36598,#36599,#36600,#36601,
#36602,#36603,#36604,#36605,#36606,#36607,#36608,#36609,#36610,#36611,#36612,
#36613,#36614,#36615,#36616,#36617,#36618,#36619,#36620,#36621,#36622,#36623,
#36624,#36625,#36626,#36627,#36628,#36629,#36630,#36631,#36632,#36633,#36634,
#36635,#36636,#36637,#36638,#36639,#36640,#36641,#36642,#36643,#36644,#36645,
#36646,#36647,#36648,#36649,#36650,#36651,#36652,#36653,#36654,#36655,#36656,
#36657,#36658,#36659,#36660,#36661),.UNSPECIFIED.,.F.,.F.,(4,3,3,3,3,3,
3,3,3,3,3,3,3,3,3,3,3,3,3,3,3,3,3,3,3,4),(359.236633112011,359.319094715865,
359.401555653835,359.484015953321,359.566475641718,359.64893474642,359.731393294819,
359.813851314306,359.896308832267,359.982986727927,360.065453513763,360.147918627107,
360.230382177612,360.31284427491,360.395305028611,360.477764548308,360.560222943576,
360.642680323973,360.725146710239,360.807609912253,360.890070368533,360.972528517444,
361.054994122323,361.137454001538,361.219918114902,361.283155162826),
 .UNSPECIFIED.);
#334=B_SPLINE_CURVE_WITH_KNOTS('',3,(#36662,#36663,#36664,#36665,#36666,
#36667,#36668,#36669,#36670,#36671,#36672,#36673,#36674,#36675,#36676,#36677,
#36678,#36679,#36680,#36681,#36682,#36683,#36684,#36685,#36686,#36687,#36688,
#36689,#36690,#36691,#36692,#36693,#36694,#36695,#36696,#36697,#36698,#36699,
#36700,#36701,#36702,#36703,#36704,#36705,#36706,#36707,#36708,#36709,#36710,
#36711,#36712,#36713,#36714,#36715,#36716,#36717,#36718,#36719,#36720,#36721,
#36722,#36723,#36724,#36725,#36726,#36727,#36728,#36729,#36730,#36731,#36732,
#36733,#36734,#36735,#36736,#36737,#36738,#36739,#36740,#36741,#36742,#36743,
#36744,#36745,#36746,#36747,#36748,#36749,#36750,#36751,#36752,#36753,#36754,
#36755,#36756,#36757,#36758,#36759,#36760,#36761,#36762,#36763,#36764,#36765,
#36766,#36767,#36768,#36769,#36770,#36771,#36772,#36773,#36774,#36775,#36776,
#36777,#36778,#36779,#36780,#36781,#36782,#36783,#36784,#36785,#36786,#36787,
#36788,#36789,#36790,#36791,#36792,#36793,#36794,#36795,#36796,#36797,#36798,
#36799,#36800,#36801,#36802,#36803,#36804,#36805,#36806,#36807,#36808,#36809,
#36810,#36811,#36812,#36813,#36814,#36815,#36816,#36817,#36818),
 .UNSPECIFIED.,.F.,.F.,(4,3,3,3,3,3,3,3,3,3,3,3,3,3,3,3,3,3,3,3,3,3,3,3,
3,3,3,3,3,3,3,3,3,3,3,3,3,3,3,3,3,3,3,3,3,3,3,3,3,3,3,3,4),(361.283155162924,
361.365617368961,361.4480792267,361.530540742994,361.613001924692,361.695462778643,
361.777923311697,361.860383530704,361.942843442512,362.025303053969,362.107762371925,
362.190221403228,362.272680154724,362.355138633263,362.437596845691,362.520054798855,
362.602512499603,362.68496995478,362.767427171235,362.853439397734,362.936763742154,
363.0192303476,363.101696108841,363.184161053294,363.266625208369,363.349088601478,
363.431551260027,363.51401321142,363.596474483059,363.678935102343,363.76139509667,
363.843854493434,363.926313320029,364.008771603846,364.091229372273,364.173686652699,
364.257819888105,364.340285886196,364.422750262552,364.505213126814,364.587674588605,
364.670134757526,364.752593743161,364.835051655079,364.920647500593,365.003112237193,
365.085574009195,365.168033255037,365.250490413014,365.332952931295,365.41541060215,
365.497869392101,365.519818419191),.UNSPECIFIED.);
#335=B_SPLINE_CURVE_WITH_KNOTS('',3,(#36824,#36825,#36826,#36827,#36828,
#36829,#36830,#36831,#36832,#36833,#36834,#36835,#36836,#36837,#36838,#36839,
#36840,#36841,#36842,#36843,#36844,#36845,#36846,#36847,#36848,#36849,#36850,
#36851,#36852,#36853,#36854,#36855,#36856,#36857,#36858,#36859,#36860,#36861,
#36862,#36863,#36864,#36865,#36866,#36867,#36868,#36869,#36870,#36871,#36872,
#36873,#36874,#36875,#36876,#36877,#36878,#36879,#36880,#36881,#36882,#36883,
#36884,#36885,#36886,#36887,#36888,#36889,#36890,#36891,#36892,#36893,#36894,
#36895,#36896,#36897,#36898,#36899,#36900,#36901,#36902,#36903,#36904,#36905,
#36906,#36907,#36908,#36909,#36910,#36911,#36912,#36913,#36914,#36915,#36916,
#36917,#36918,#36919,#36920,#36921,#36922,#36923,#36924,#36925,#36926,#36927,
#36928,#36929,#36930,#36931,#36932,#36933,#36934,#36935,#36936,#36937,#36938,
#36939,#36940,#36941,#36942,#36943,#36944,#36945,#36946,#36947,#36948,#36949,
#36950,#36951,#36952,#36953,#36954,#36955,#36956,#36957,#36958,#36959,#36960,
#36961,#36962,#36963,#36964,#36965,#36966,#36967,#36968,#36969,#36970,#36971,
#36972,#36973,#36974,#36975,#36976,#36977,#36978,#36979,#36980),
 .UNSPECIFIED.,.F.,.F.,(4,3,3,3,3,3,3,3,3,3,3,3,3,3,3,3,3,3,3,3,3,3,3,3,
3,3,3,3,3,3,3,3,3,3,3,3,3,3,3,3,3,3,3,3,3,3,3,3,3,3,3,3,4),(367.566340470006,
367.648802676042,367.731264533782,367.813726050076,367.896187231773,367.978648085724,
368.061108618779,368.143568837785,368.226028749593,368.308488361051,368.390947679007,
368.473406710309,368.555865461806,368.638323940344,368.720782152772,368.803240105936,
368.885697806684,368.968155261862,369.050612478316,369.136624704818,369.219949049241,
369.302415654687,369.384881415928,369.467346360381,369.549810515457,369.632273908566,
369.714736567114,369.797198518507,369.879659790146,369.96212040943,370.044580403757,
370.127039800521,370.209498627116,370.291956910933,370.37441467936,370.456871959786,
370.541005195197,370.623471193289,370.705935569645,370.788398433907,370.870859895697,
370.953320064619,371.035779050254,371.118236962171,371.203832807696,371.286297544296,
371.368759316298,371.451218562141,371.533675720118,371.616138238399,371.698595909254,
371.781054699205,371.803003726371),.UNSPECIFIED.);
#336=B_SPLINE_CURVE_WITH_KNOTS('',3,(#36981,#36982,#36983,#36984,#36985,
#36986,#36987,#36988,#36989,#36990,#36991,#36992,#36993,#36994,#36995,#36996,
#36997,#36998,#36999,#37000,#37001,#37002,#37003,#37004,#37005,#37006,#37007,
#37008,#37009,#37010,#37011,#37012,#37013,#37014,#37015,#37016,#37017,#37018,
#37019,#37020,#37021,#37022,#37023,#37024,#37025,#37026,#37027,#37028,#37029,
#37030,#37031,#37032,#37033,#37034,#37035,#37036,#37037,#37038,#37039,#37040,
#37041,#37042,#37043,#37044,#37045,#37046,#37047,#37048,#37049,#37050,#37051,
#37052,#37053,#37054,#37055,#37056,#37057,#37058,#37059),.UNSPECIFIED.,
 .F.,.F.,(4,3,3,3,3,3,3,3,3,3,3,3,3,3,3,3,3,3,3,3,3,3,3,3,3,3,4),(365.520350523813,
365.59761345909,365.674861075843,365.752102564901,365.829351979924,365.9066233764,
365.983975351626,366.061368388441,366.138876067688,366.212922124861,366.289743322016,
366.36647528423,366.443134262378,366.519736448839,366.59629799072,366.673345208909,
366.749889383553,366.826443663599,366.903022628578,366.980435905491,367.057147385798,
367.134911561014,367.21267573623,367.304424888357,367.395763544426,367.486235917466,
367.566340470006),.UNSPECIFIED.);
#337=B_SPLINE_CURVE_WITH_KNOTS('',3,(#37061,#37062,#37063,#37064,#37065,
#37066,#37067,#37068,#37069,#37070,#37071,#37072,#37073,#37074,#37075,#37076,
#37077,#37078,#37079,#37080,#37081,#37082,#37083,#37084,#37085,#37086,#37087,
#37088,#37089,#37090,#37091,#37092,#37093,#37094,#37095,#37096,#37097,#37098,
#37099,#37100,#37101,#37102,#37103,#37104,#37105,#37106,#37107,#37108,#37109,
#37110,#37111,#37112,#37113,#37114,#37115,#37116,#37117,#37118,#37119,#37120,
#37121,#37122,#37123,#37124,#37125,#37126,#37127,#37128,#37129,#37130,#37131,
#37132,#37133,#37134,#37135,#37136),.UNSPECIFIED.,.F.,.F.,(4,3,3,3,3,3,
3,3,3,3,3,3,3,3,3,3,3,3,3,3,3,3,3,3,3,4),(365.519818419191,365.602280023045,
365.684740961015,365.767201260501,365.849660948898,365.9321200536,366.014578601999,
366.097036621485,366.179494139447,366.266172035107,366.348638820942,366.431103934286,
366.513567484791,366.596029582089,366.67849033579,366.760949855487,366.843408250755,
366.925865631152,367.008332017419,367.090795219433,367.173255675713,367.255713824624,
367.338179429503,367.420639308717,367.503103422081,367.566340470006),
 .UNSPECIFIED.);
#338=B_SPLINE_CURVE_WITH_KNOTS('',3,(#37137,#37138,#37139,#37140,#37141,
#37142,#37143,#37144,#37145,#37146,#37147,#37148,#37149,#37150,#37151,#37152,
#37153,#37154,#37155,#37156,#37157,#37158,#37159,#37160,#37161,#37162,#37163,
#37164,#37165,#37166,#37167,#37168,#37169,#37170,#37171,#37172,#37173,#37174,
#37175,#37176,#37177,#37178,#37179,#37180,#37181,#37182,#37183,#37184,#37185,
#37186,#37187,#37188,#37189,#37190,#37191,#37192,#37193,#37194,#37195,#37196,
#37197,#37198,#37199,#37200,#37201,#37202,#37203,#37204,#37205,#37206,#37207,
#37208,#37209,#37210,#37211,#37212,#37213,#37214,#37215,#37216,#37217,#37218,
#37219,#37220,#37221,#37222,#37223,#37224,#37225,#37226,#37227,#37228,#37229,
#37230,#37231,#37232,#37233,#37234,#37235,#37236,#37237,#37238,#37239,#37240,
#37241,#37242,#37243,#37244,#37245,#37246,#37247,#37248,#37249,#37250,#37251,
#37252,#37253,#37254,#37255,#37256,#37257,#37258,#37259,#37260,#37261,#37262,
#37263,#37264,#37265,#37266,#37267,#37268,#37269,#37270,#37271,#37272,#37273,
#37274,#37275,#37276,#37277,#37278,#37279,#37280,#37281,#37282,#37283,#37284,
#37285,#37286,#37287,#37288,#37289,#37290,#37291,#37292,#37293,#37294,#37295,
#37296,#37297,#37298,#37299,#37300,#37301,#37302,#37303,#37304,#37305),
 .UNSPECIFIED.,.F.,.F.,(4,3,3,3,3,3,3,3,3,3,3,3,3,3,3,3,3,3,3,3,3,3,3,3,
3,3,3,3,3,3,3,3,3,3,3,3,3,3,3,3,3,3,3,3,3,3,3,3,3,3,3,3,3,3,3,3,4),(367.566340470006,
367.648290370595,367.73037350154,367.812676296979,367.895091244229,367.977702695954,
368.046691721997,368.12352775412,368.200274769847,368.27694900741,368.353566646932,
368.430143823559,368.50701331187,368.583573414393,368.66014371154,368.736738772563,
368.813829011934,368.890556208516,368.967827969282,369.045099730048,369.122694399482,
369.200196665592,369.277622150663,369.35498642204,369.432305003131,369.509600707602,
369.586885752258,369.664174144191,369.741479889717,369.818857929704,369.896273001449,
369.97379361572,370.043507738099,370.124994052532,370.206376134891,370.290460036699,
370.371617355552,370.452698139307,370.533688131341,370.542711742124,370.623724848415,
370.704813542688,370.789089093553,370.870398559943,370.951785461154,371.033292599919,
371.04191574615,371.11945589795,371.196912152052,371.274287332535,371.351616341408,
371.428913220703,371.506191991676,371.583487044263,371.660788730736,371.738144147497,
371.802470582125),.UNSPECIFIED.);
#339=B_SPLINE_CURVE_WITH_KNOTS('',3,(#37311,#37312,#37313,#37314,#37315,
#37316,#37317,#37318,#37319,#37320,#37321,#37322,#37323,#37324,#37325,#37326,
#37327,#37328,#37329,#37330,#37331,#37332,#37333,#37334,#37335,#37336,#37337,
#37338,#37339,#37340,#37341,#37342,#37343,#37344,#37345,#37346,#37347,#37348,
#37349,#37350,#37351,#37352,#37353,#37354,#37355,#37356,#37357,#37358,#37359,
#37360,#37361,#37362,#37363,#37364,#37365,#37366,#37367,#37368,#37369,#37370,
#37371,#37372,#37373,#37374,#37375,#37376,#37377,#37378,#37379,#37380,#37381,
#37382,#37383,#37384,#37385,#37386,#37387,#37388,#37389,#37390,#37391,#37392,
#37393,#37394,#37395,#37396,#37397,#37398,#37399,#37400,#37401,#37402,#37403,
#37404,#37405,#37406,#37407,#37408,#37409,#37410,#37411,#37412,#37413,#37414,
#37415,#37416,#37417,#37418,#37419,#37420,#37421,#37422,#37423,#37424,#37425,
#37426,#37427,#37428,#37429,#37430,#37431,#37432,#37433,#37434,#37435,#37436,
#37437,#37438,#37439,#37440,#37441,#37442,#37443,#37444,#37445,#37446,#37447,
#37448,#37449,#37450,#37451,#37452,#37453,#37454,#37455,#37456,#37457,#37458,
#37459,#37460,#37461,#37462,#37463,#37464,#37465,#37466,#37467,#37468,#37469,
#37470,#37471,#37472,#37473,#37474,#37475,#37476,#37477,#37478,#37479),
 .UNSPECIFIED.,.F.,.F.,(4,3,3,3,3,3,3,3,3,3,3,3,3,3,3,3,3,3,3,3,3,3,3,3,
3,3,3,3,3,3,3,3,3,3,3,3,3,3,3,3,3,3,3,3,3,3,3,3,3,3,3,3,3,3,3,3,4),(373.849525777186,
373.939882086844,374.027315055066,374.119133035441,374.210951015816,374.28853363943,
374.366023621639,374.443436598864,374.520788152365,374.598093819277,374.675376412322,
374.752648199266,374.829923199122,374.907215430061,374.984580102425,375.061981710858,
375.139489525466,375.210704627185,375.29218860014,375.373567964279,375.457821331427,
375.538974826598,375.620051504557,375.701036932347,375.71058143287,375.791589828774,
375.872674085606,375.957120123843,376.03842620555,376.119809995319,376.201314656348,
376.210458238554,376.287974016817,376.365408317228,376.442776735655,376.520094820805,
376.59737808485,376.674655169161,376.751931749649,376.829221845046,376.906539479051,
376.983945685375,377.061397694688,377.13897050301,377.210211849924,377.287067742821,
377.363828411422,377.440510132449,377.521143703061,377.597712851444,377.674257387839,
377.750791894756,377.827330946169,377.903916893023,377.980530118534,378.057216121923,
378.085578697343),.UNSPECIFIED.);
#340=B_SPLINE_CURVE_WITH_KNOTS('',3,(#37480,#37481,#37482,#37483,#37484,
#37485,#37486,#37487,#37488,#37489,#37490,#37491,#37492,#37493,#37494,#37495,
#37496,#37497,#37498,#37499,#37500,#37501,#37502,#37503,#37504,#37505,#37506,
#37507,#37508,#37509,#37510,#37511,#37512,#37513,#37514,#37515,#37516,#37517,
#37518,#37519,#37520,#37521,#37522,#37523,#37524,#37525,#37526,#37527,#37528,
#37529,#37530,#37531,#37532,#37533,#37534,#37535,#37536,#37537,#37538,#37539,
#37540,#37541,#37542,#37543,#37544,#37545,#37546,#37547,#37548,#37549,#37550,
#37551,#37552,#37553,#37554,#37555),.UNSPECIFIED.,.F.,.F.,(4,3,3,3,3,3,
3,3,3,3,3,3,3,3,3,3,3,3,3,3,3,3,3,3,3,4),(371.803003726371,371.885465330225,
371.967926268195,372.050386567681,372.132846256078,372.21530536078,372.297763909179,
372.380221928665,372.462679446627,372.549357342287,372.631824128122,372.714289241466,
372.796752791971,372.879214889269,372.96167564297,373.044135162667,373.126593557935,
373.209050938332,373.291517324598,373.373980526612,373.456440982893,373.538899131804,
373.621364736683,373.703824615897,373.786288729261,373.849525777186),
 .UNSPECIFIED.);
#341=B_SPLINE_CURVE_WITH_KNOTS('',3,(#37557,#37558,#37559,#37560,#37561,
#37562,#37563,#37564,#37565,#37566,#37567,#37568,#37569,#37570,#37571,#37572,
#37573,#37574,#37575,#37576,#37577,#37578,#37579,#37580,#37581,#37582,#37583,
#37584,#37585,#37586,#37587,#37588,#37589,#37590,#37591,#37592,#37593,#37594,
#37595,#37596,#37597,#37598,#37599,#37600,#37601,#37602,#37603,#37604,#37605,
#37606,#37607,#37608,#37609,#37610,#37611,#37612,#37613,#37614,#37615,#37616,
#37617,#37618,#37619,#37620,#37621,#37622,#37623,#37624,#37625,#37626,#37627,
#37628,#37629,#37630,#37631,#37632,#37633,#37634,#37635,#37636,#37637,#37638),
 .UNSPECIFIED.,.F.,.F.,(4,3,3,3,3,3,3,3,3,3,3,3,3,3,3,3,3,3,3,3,3,3,3,3,
3,3,3,4),(371.802470582125,371.879927317619,371.96012553591,372.040323754201,
372.117187138853,372.193956970663,372.270649506651,372.347280941818,372.423867422602,
372.500725465058,372.577283788021,372.653848122693,372.730433035821,372.807507717428,
372.884214538297,372.961473150274,373.038731762251,373.115212093748,373.191604985852,
373.267926963156,373.344189739056,373.420420198739,373.496633175304,373.572843488199,
373.649093809448,373.725365467059,373.801709882622,373.849525777084),
 .UNSPECIFIED.);
#342=B_SPLINE_CURVE_WITH_KNOTS('',3,(#37639,#37640,#37641,#37642,#37643,
#37644,#37645,#37646,#37647,#37648,#37649,#37650,#37651,#37652,#37653,#37654,
#37655,#37656,#37657,#37658,#37659,#37660,#37661,#37662,#37663,#37664,#37665,
#37666,#37667,#37668,#37669,#37670,#37671,#37672,#37673,#37674,#37675,#37676,
#37677,#37678,#37679,#37680,#37681,#37682,#37683,#37684,#37685,#37686,#37687,
#37688,#37689,#37690,#37691,#37692,#37693,#37694,#37695,#37696,#37697,#37698,
#37699,#37700,#37701,#37702,#37703,#37704,#37705,#37706,#37707,#37708,#37709,
#37710,#37711,#37712,#37713,#37714,#37715,#37716,#37717,#37718,#37719,#37720,
#37721,#37722,#37723,#37724,#37725,#37726,#37727,#37728,#37729,#37730,#37731,
#37732,#37733,#37734,#37735,#37736,#37737,#37738,#37739,#37740,#37741,#37742,
#37743,#37744,#37745,#37746,#37747,#37748,#37749,#37750,#37751,#37752,#37753,
#37754,#37755,#37756,#37757,#37758,#37759,#37760,#37761,#37762,#37763,#37764,
#37765,#37766,#37767,#37768,#37769,#37770,#37771,#37772,#37773,#37774,#37775,
#37776,#37777,#37778,#37779,#37780,#37781,#37782,#37783,#37784,#37785,#37786,
#37787,#37788,#37789,#37790,#37791,#37792,#37793,#37794,#37795,#37796,#37797,
#37798,#37799,#37800,#37801,#37802,#37803,#37804,#37805,#37806,#37807),
 .UNSPECIFIED.,.F.,.F.,(4,3,3,3,3,3,3,3,3,3,3,3,3,3,3,3,3,3,3,3,3,3,3,3,
3,3,3,3,3,3,3,3,3,3,3,3,3,3,3,3,3,3,3,3,3,3,3,3,3,3,3,3,3,3,3,3,4),(373.849525777185,
373.962412552688,374.037139770302,374.114669888365,374.192112917681,374.269484499507,
374.346800223867,374.424075640428,374.501336516453,374.5785918278,374.655855615891,
374.733141924275,374.810508785882,374.887917179814,374.965438812686,375.035547778353,
375.112383810476,375.189130826203,375.265805063766,375.342422703287,375.418999879914,
375.495869368226,375.572429470748,375.648999767896,375.725594828918,375.80268506829,
375.879412264871,375.956684025638,376.033955786404,376.111550455838,376.189052721949,
376.266478207019,376.343842478396,376.421161059487,376.498456763959,376.575741808615,
376.653030200548,376.730335946073,376.807713986061,376.885129057805,376.962649672077,
377.032363794455,377.113850108888,377.195232191247,377.279316093056,377.360473411909,
377.441554195663,377.522544187697,377.531567798481,377.612580904771,377.693669599045,
377.77794514991,377.8592546163,377.94064151751,378.022148656275,378.030771802506,
378.086546493803),.UNSPECIFIED.);
#343=B_SPLINE_CURVE_WITH_KNOTS('',3,(#37813,#37814,#37815,#37816,#37817,
#37818,#37819,#37820,#37821,#37822,#37823,#37824,#37825,#37826,#37827,#37828,
#37829,#37830,#37831,#37832,#37833,#37834,#37835,#37836,#37837,#37838,#37839,
#37840,#37841,#37842,#37843,#37844,#37845,#37846,#37847,#37848,#37849,#37850,
#37851,#37852,#37853,#37854,#37855,#37856,#37857,#37858,#37859,#37860,#37861,
#37862,#37863,#37864,#37865,#37866,#37867,#37868,#37869,#37870,#37871,#37872,
#37873,#37874,#37875,#37876,#37877,#37878,#37879,#37880,#37881,#37882,#37883,
#37884,#37885,#37886,#37887,#37888,#37889,#37890,#37891,#37892,#37893,#37894,
#37895,#37896,#37897,#37898,#37899,#37900,#37901,#37902,#37903,#37904,#37905,
#37906,#37907,#37908,#37909,#37910,#37911,#37912,#37913,#37914,#37915,#37916,
#37917,#37918,#37919,#37920,#37921,#37922,#37923,#37924,#37925,#37926,#37927,
#37928,#37929,#37930,#37931,#37932,#37933,#37934,#37935,#37936,#37937,#37938,
#37939,#37940,#37941,#37942,#37943,#37944,#37945,#37946,#37947,#37948,#37949,
#37950,#37951,#37952,#37953,#37954,#37955,#37956,#37957,#37958,#37959,#37960,
#37961,#37962,#37963,#37964,#37965,#37966,#37967,#37968,#37969,#37970,#37971,
#37972,#37973,#37974,#37975,#37976,#37977,#37978,#37979,#37980,#37981,#37982,
#37983,#37984),.UNSPECIFIED.,.F.,.F.,(4,3,3,3,3,3,3,3,3,3,3,3,3,3,3,3,3,
3,3,3,3,3,3,3,3,3,3,3,3,3,3,3,3,3,3,3,3,3,3,3,3,3,3,3,3,3,3,3,3,3,3,3,3,
3,3,3,3,4),(380.132711084365,380.209472684032,380.286293881187,380.363025843401,
380.439684821549,380.516287008011,380.592848549892,380.66989576808,380.746439942725,
380.82299422277,380.89957318775,380.976986464663,381.05369794497,381.131462120185,
381.209226295401,381.286808919015,381.364298901224,381.441711878449,381.51906343195,
381.596369098861,381.673651691906,381.750923478849,381.828198478706,381.905490709644,
381.982855382009,382.060256990441,382.137764805049,382.208979906771,382.290463879726,
382.371843243866,382.456096611013,382.537250106185,382.618326784144,382.699312211935,
382.708856712455,382.789865108359,382.87094936519,382.955395403427,383.036701485134,
383.118085274902,383.199589935931,383.20873351814,383.286249296403,383.363683596814,
383.441052015241,383.518370100391,383.595653364436,383.672930448747,383.750207029235,
383.827497124633,383.904814758637,383.982220964962,384.059672974275,384.137245782597,
384.208487129509,384.289356128012,384.366119952296,384.370225126515),
 .UNSPECIFIED.);
#344=B_SPLINE_CURVE_WITH_KNOTS('',3,(#37985,#37986,#37987,#37988,#37989,
#37990,#37991,#37992,#37993,#37994,#37995,#37996,#37997,#37998,#37999,#38000,
#38001,#38002,#38003,#38004,#38005,#38006,#38007,#38008,#38009,#38010,#38011,
#38012,#38013,#38014,#38015,#38016,#38017,#38018,#38019,#38020,#38021,#38022,
#38023,#38024,#38025,#38026,#38027,#38028,#38029,#38030,#38031,#38032,#38033,
#38034,#38035,#38036,#38037,#38038,#38039,#38040,#38041,#38042,#38043,#38044,
#38045,#38046,#38047,#38048,#38049,#38050,#38051,#38052,#38053,#38054,#38055,
#38056,#38057,#38058,#38059,#38060,#38061,#38062,#38063,#38064,#38065,#38066),
 .UNSPECIFIED.,.F.,.F.,(4,3,3,3,3,3,3,3,3,3,3,3,3,3,3,3,3,3,3,3,3,3,3,3,
3,3,3,4),(378.085578697343,378.162400136614,378.209965461293,378.287483012911,
378.364913232331,378.442271775226,378.519574245813,378.596836207763,378.674083433546,
378.751324944753,378.828574794986,378.905847039899,378.98319999787,379.060594390178,
379.138102717847,379.209719072662,379.286373742231,379.362941556512,379.43943891038,
379.515882139391,379.592985757496,379.669379149644,379.745770602541,379.822174824489,
379.899808889424,379.976317652966,380.054514368598,380.132711084231),
 .UNSPECIFIED.);
#345=B_SPLINE_CURVE_WITH_KNOTS('',3,(#38068,#38069,#38070,#38071,#38072,
#38073,#38074,#38075,#38076,#38077,#38078,#38079,#38080,#38081,#38082,#38083,
#38084,#38085,#38086,#38087,#38088,#38089,#38090,#38091,#38092,#38093,#38094,
#38095,#38096,#38097,#38098,#38099,#38100,#38101,#38102,#38103,#38104,#38105,
#38106,#38107,#38108,#38109,#38110,#38111,#38112,#38113,#38114,#38115,#38116,
#38117,#38118,#38119,#38120,#38121,#38122,#38123,#38124,#38125,#38126,#38127,
#38128,#38129,#38130,#38131,#38132,#38133,#38134,#38135,#38136,#38137,#38138,
#38139,#38140,#38141,#38142,#38143,#38144,#38145,#38146,#38147,#38148,#38149),
 .UNSPECIFIED.,.F.,.F.,(4,3,3,3,3,3,3,3,3,3,3,3,3,3,3,3,3,3,3,3,3,3,3,3,
3,3,3,4),(378.086546493803,378.164014608403,378.241412658057,378.318756189873,
378.396060711637,378.475200599002,378.552489271051,378.629787960677,378.707110677723,
378.787627960932,378.865082320076,378.942592443613,379.020205864669,379.029179810557,
379.106043195209,379.182813027019,379.259505563008,379.336136998175,379.412723478958,
379.489581521414,379.566139844378,379.64270417905,379.719289092178,379.796363773785,
379.873070594654,379.950329206631,380.027587818608,380.132711084365),
 .UNSPECIFIED.);
#346=B_SPLINE_CURVE_WITH_KNOTS('',3,(#38150,#38151,#38152,#38153,#38154,
#38155,#38156,#38157,#38158,#38159,#38160,#38161,#38162,#38163,#38164,#38165,
#38166,#38167,#38168,#38169,#38170,#38171,#38172,#38173,#38174,#38175,#38176,
#38177,#38178,#38179,#38180,#38181,#38182,#38183,#38184,#38185,#38186,#38187,
#38188,#38189,#38190,#38191,#38192,#38193,#38194,#38195,#38196,#38197,#38198,
#38199,#38200,#38201,#38202,#38203,#38204,#38205,#38206,#38207,#38208,#38209,
#38210,#38211,#38212,#38213,#38214,#38215,#38216,#38217,#38218,#38219,#38220,
#38221,#38222,#38223,#38224,#38225,#38226,#38227,#38228,#38229,#38230,#38231,
#38232,#38233,#38234,#38235,#38236,#38237,#38238,#38239,#38240,#38241,#38242,
#38243,#38244,#38245,#38246,#38247,#38248,#38249,#38250,#38251,#38252,#38253,
#38254,#38255,#38256,#38257,#38258,#38259,#38260,#38261,#38262,#38263,#38264,
#38265,#38266,#38267,#38268,#38269,#38270,#38271,#38272,#38273,#38274,#38275,
#38276,#38277,#38278,#38279,#38280,#38281,#38282,#38283,#38284,#38285,#38286,
#38287,#38288,#38289,#38290,#38291,#38292,#38293,#38294,#38295,#38296,#38297,
#38298,#38299,#38300,#38301,#38302,#38303,#38304,#38305,#38306,#38307,#38308,
#38309,#38310,#38311,#38312,#38313,#38314,#38315,#38316,#38317,#38318),
 .UNSPECIFIED.,.F.,.F.,(4,3,3,3,3,3,3,3,3,3,3,3,3,3,3,3,3,3,3,3,3,3,3,3,
3,3,3,3,3,3,3,3,3,3,3,3,3,3,3,3,3,3,3,3,3,3,3,3,3,3,3,3,3,3,3,3,4),(380.132711084509,
380.209146011696,380.285502285353,380.361796391818,380.438044762713,380.51427208158,
380.590490501068,380.666714837056,380.74295990752,380.819281847043,380.895645188911,
380.972115510485,381.025995826659,381.103525944722,381.180968974038,381.258340555864,
381.335656280224,381.412931696785,381.49019257281,381.567447884157,381.644711672248,
381.721997980632,381.799364842238,381.87677323617,381.954294869042,382.02440383471,
382.101239866833,382.17798688256,382.254661120123,382.331278759644,382.407855936271,
382.484725424582,382.561285527105,382.637855824252,382.714450885275,382.791541124646,
382.868268321228,382.945540081994,383.022811842761,383.100406512195,383.177908778305,
383.255334263376,383.332698534753,383.410017115843,383.487312820315,383.564597864971,
383.641886256904,383.71919200243,383.796570042417,383.873985114162,383.951505728433,
384.021219850812,384.102728867264,384.184095183531,384.265374191124,384.346544891823,
384.369798917099),.UNSPECIFIED.);
#347=B_SPLINE_CURVE_WITH_KNOTS('',3,(#38324,#38325,#38326,#38327,#38328,
#38329,#38330,#38331,#38332,#38333,#38334,#38335,#38336,#38337,#38338,#38339,
#38340,#38341,#38342,#38343,#38344,#38345,#38346,#38347,#38348,#38349,#38350,
#38351,#38352,#38353,#38354,#38355,#38356,#38357,#38358,#38359,#38360,#38361,
#38362,#38363,#38364,#38365,#38366,#38367,#38368,#38369,#38370,#38371,#38372,
#38373,#38374,#38375,#38376,#38377,#38378,#38379,#38380,#38381,#38382,#38383,
#38384,#38385,#38386,#38387,#38388,#38389,#38390,#38391,#38392,#38393,#38394,
#38395,#38396,#38397,#38398,#38399,#38400,#38401,#38402,#38403,#38404,#38405,
#38406,#38407,#38408,#38409,#38410,#38411,#38412,#38413,#38414,#38415,#38416,
#38417,#38418,#38419,#38420,#38421,#38422,#38423,#38424,#38425,#38426,#38427,
#38428,#38429,#38430,#38431,#38432,#38433,#38434,#38435,#38436,#38437,#38438,
#38439,#38440,#38441,#38442,#38443,#38444,#38445,#38446,#38447,#38448,#38449,
#38450,#38451,#38452,#38453,#38454,#38455,#38456,#38457,#38458,#38459,#38460,
#38461,#38462,#38463,#38464,#38465,#38466,#38467,#38468,#38469,#38470,#38471,
#38472,#38473,#38474,#38475,#38476,#38477,#38478,#38479,#38480,#38481,#38482,
#38483,#38484,#38485,#38486,#38487,#38488,#38489,#38490,#38491,#38492,#38493,
#38494,#38495),.UNSPECIFIED.,.F.,.F.,(4,3,3,3,3,3,3,3,3,3,3,3,3,3,3,3,3,
3,3,3,3,3,3,3,3,3,3,3,3,3,3,3,3,3,3,3,3,3,3,3,3,3,3,3,3,3,3,3,3,3,3,3,3,
3,3,3,3,4),(386.415896391638,386.492266579159,386.568580662424,386.648476575073,
386.724737129527,386.800994886678,386.877264638518,386.953561182954,387.029937546182,
387.106360703212,387.182883946858,387.207747963617,387.284569160772,387.361301122986,
387.437960101134,387.514562287595,387.591123829476,387.668171047665,387.744715222309,
387.821269502354,387.897848467334,387.975261744247,388.051973224554,388.129737399771,
388.207501574987,388.285084198601,388.36257418081,388.439987158035,388.517338711537,
388.594644378448,388.671926971493,388.749198758437,388.826473758294,388.903765989233,
388.981130661597,389.05853227003,389.136040084638,389.207255186356,389.288739159311,
389.370118523451,389.454371890598,389.53552538577,389.616602063728,389.697587491518,
389.707131992041,389.788140387945,389.869224644777,389.953670683014,390.034976764721,
390.116360554489,390.197865215518,390.207008797725,390.284529776728,390.361971240382,
390.439334128285,390.516651255725,390.593936971202,390.65265496374),
 .UNSPECIFIED.);
#348=B_SPLINE_CURVE_WITH_KNOTS('',3,(#38496,#38497,#38498,#38499,#38500,
#38501,#38502,#38503,#38504,#38505,#38506,#38507,#38508,#38509,#38510,#38511,
#38512,#38513,#38514,#38515,#38516,#38517,#38518,#38519,#38520,#38521,#38522,
#38523,#38524,#38525,#38526,#38527,#38528,#38529,#38530,#38531,#38532,#38533,
#38534,#38535,#38536,#38537,#38538,#38539,#38540,#38541,#38542,#38543,#38544,
#38545,#38546,#38547,#38548,#38549,#38550,#38551,#38552,#38553,#38554,#38555,
#38556,#38557,#38558,#38559,#38560,#38561,#38562,#38563,#38564,#38565,#38566,
#38567,#38568,#38569,#38570,#38571,#38572,#38573,#38574),.UNSPECIFIED.,
 .F.,.F.,(4,3,3,3,3,3,3,3,3,3,3,3,3,3,3,3,3,3,3,3,3,3,3,3,3,3,4),(384.370225126515,
384.446895198235,384.52350568592,384.600072743613,384.676622302571,384.753164657178,
384.829714382817,384.906286057132,384.982939517875,385.059634903868,385.13644705767,
385.208240740879,385.285758292497,385.363188511917,385.440547054812,385.5178495254,
385.59511148735,385.672358713133,385.74960022434,385.826850074573,385.904122319486,
385.981475277457,386.058869669766,386.136377997434,386.207994352248,386.315585392158,
386.415896391545),.UNSPECIFIED.);
#349=B_SPLINE_CURVE_WITH_KNOTS('',3,(#38576,#38577,#38578,#38579,#38580,
#38581,#38582,#38583,#38584,#38585,#38586,#38587,#38588,#38589,#38590,#38591,
#38592,#38593,#38594,#38595,#38596,#38597,#38598,#38599,#38600,#38601,#38602,
#38603,#38604,#38605,#38606,#38607,#38608,#38609,#38610,#38611,#38612,#38613,
#38614,#38615,#38616,#38617,#38618,#38619,#38620,#38621,#38622,#38623,#38624,
#38625,#38626,#38627,#38628,#38629,#38630,#38631,#38632,#38633,#38634,#38635,
#38636,#38637,#38638,#38639,#38640,#38641,#38642,#38643,#38644,#38645,#38646,
#38647,#38648,#38649,#38650,#38651,#38652,#38653,#38654,#38655,#38656,#38657),
 .UNSPECIFIED.,.F.,.F.,(4,3,3,3,3,3,3,3,3,3,3,3,3,3,3,3,3,3,3,3,3,3,3,3,
3,3,3,4),(384.369798917099,384.450830355207,384.520423854837,384.601436961128,
384.6825256554,384.766801206265,384.848110672655,384.929497573866,385.011004712631,
385.019627858862,385.097156012071,385.174602887032,385.251984065739,385.3293150832,
385.40661143803,385.483901738366,385.561191646104,385.638495168102,385.71582631623,
385.793245806051,385.870711164473,385.948296550771,386.018035866913,386.103676425215,
386.188941402707,386.273971573959,386.358616605109,386.415896391545),
 .UNSPECIFIED.);
#350=B_SPLINE_CURVE_WITH_KNOTS('',3,(#38658,#38659,#38660,#38661,#38662,
#38663,#38664,#38665,#38666,#38667,#38668,#38669,#38670,#38671,#38672,#38673,
#38674,#38675,#38676,#38677,#38678,#38679,#38680,#38681,#38682,#38683,#38684,
#38685,#38686,#38687,#38688,#38689,#38690,#38691,#38692,#38693,#38694,#38695,
#38696,#38697,#38698,#38699,#38700,#38701,#38702,#38703,#38704,#38705,#38706,
#38707,#38708,#38709,#38710,#38711,#38712,#38713,#38714,#38715,#38716,#38717,
#38718,#38719,#38720,#38721,#38722,#38723,#38724,#38725,#38726,#38727,#38728,
#38729,#38730,#38731,#38732,#38733,#38734,#38735,#38736,#38737,#38738,#38739,
#38740,#38741,#38742,#38743,#38744,#38745,#38746,#38747,#38748,#38749,#38750,
#38751,#38752,#38753,#38754,#38755,#38756,#38757,#38758,#38759,#38760,#38761,
#38762,#38763,#38764,#38765,#38766,#38767,#38768,#38769,#38770,#38771,#38772,
#38773,#38774,#38775,#38776,#38777,#38778,#38779,#38780,#38781,#38782,#38783,
#38784,#38785,#38786,#38787,#38788,#38789,#38790,#38791,#38792,#38793,#38794,
#38795,#38796,#38797,#38798,#38799,#38800,#38801,#38802,#38803,#38804,#38805,
#38806,#38807,#38808,#38809,#38810,#38811,#38812,#38813,#38814),
 .UNSPECIFIED.,.F.,.F.,(4,3,3,3,3,3,3,3,3,3,3,3,3,3,3,3,3,3,3,3,3,3,3,3,
3,3,3,3,3,3,3,3,3,3,3,3,3,3,3,3,3,3,3,3,3,3,3,3,3,3,3,3,4),(386.415896391545,
386.498358597581,386.580820455321,386.663281971615,386.745743153312,386.828204007263,
386.910664540318,386.993124759324,387.075584671132,387.15804428259,387.240503600546,
387.322962631848,387.405421383345,387.487879861883,387.570338074311,387.652796027475,
387.735253728223,387.817711183401,387.900168399856,387.986180626357,388.069504970781,
388.151971576226,388.234437337468,388.31690228192,388.399366436996,388.481829830105,
388.564292488654,388.646754440046,388.729215711685,388.811676330969,388.894136325296,
388.976595722061,389.059054548656,389.141512832472,389.2239706009,389.306427881325,
389.390561116737,389.473027114828,389.555491491184,389.637954355446,389.720415817236,
389.802875986158,389.885334971793,389.96779288371,390.053388729235,390.135853465835,
390.218315237837,390.300774483679,390.383231641656,390.465694159938,390.548151830793,
390.630610620743,390.652559647909),.UNSPECIFIED.);
#351=B_SPLINE_CURVE_WITH_KNOTS('',3,(#38820,#38821,#38822,#38823,#38824,
#38825,#38826,#38827,#38828,#38829,#38830,#38831,#38832,#38833,#38834,#38835,
#38836,#38837,#38838,#38839,#38840,#38841,#38842,#38843,#38844,#38845,#38846,
#38847,#38848,#38849,#38850,#38851,#38852,#38853,#38854,#38855,#38856,#38857,
#38858,#38859,#38860,#38861,#38862,#38863,#38864,#38865,#38866,#38867,#38868,
#38869,#38870,#38871,#38872,#38873,#38874,#38875,#38876,#38877,#38878,#38879,
#38880,#38881,#38882,#38883,#38884,#38885,#38886,#38887,#38888,#38889,#38890,
#38891,#38892,#38893,#38894,#38895,#38896,#38897,#38898,#38899,#38900,#38901,
#38902,#38903,#38904,#38905,#38906,#38907,#38908,#38909,#38910,#38911,#38912,
#38913,#38914,#38915,#38916,#38917,#38918,#38919,#38920,#38921,#38922,#38923,
#38924,#38925,#38926,#38927,#38928,#38929,#38930,#38931,#38932,#38933,#38934,
#38935,#38936,#38937,#38938,#38939,#38940,#38941,#38942,#38943,#38944,#38945,
#38946,#38947,#38948,#38949,#38950,#38951,#38952,#38953,#38954,#38955,#38956,
#38957,#38958,#38959,#38960,#38961,#38962,#38963,#38964,#38965,#38966,#38967,
#38968,#38969,#38970,#38971,#38972,#38973,#38974,#38975,#38976),
 .UNSPECIFIED.,.F.,.F.,(4,3,3,3,3,3,3,3,3,3,3,3,3,3,3,3,3,3,3,3,3,3,3,3,
3,3,3,3,3,3,3,3,3,3,3,3,3,3,3,3,3,3,3,3,3,3,3,3,3,3,3,3,4),(392.699081698725,
392.781543904761,392.864005762501,392.946467278795,393.028928460492,393.111389314443,
393.193849847498,393.276310066504,393.358769978312,393.44122958977,393.523688907726,
393.606147939028,393.688606690525,393.771065169063,393.853523381491,393.935981334655,
394.018439035403,394.100896490581,394.183353707035,394.269365933537,394.35269027796,
394.435156883406,394.517622644647,394.6000875891,394.682551744176,394.765015137285,
394.847477795833,394.929939747226,395.012401018865,395.094861638149,395.177321632476,
395.25978102924,395.342239855835,395.424698139652,395.507155908079,395.589613188505,
395.673746423916,395.756212422008,395.838676798363,395.921139662626,396.003601124416,
396.086061293337,396.168520278973,396.25097819089,396.336574036415,396.419038773015,
396.501500545017,396.583959790859,396.666416948836,396.748879467117,396.831337137972,
396.913795927923,396.935744955089),.UNSPECIFIED.);
#352=B_SPLINE_CURVE_WITH_KNOTS('',3,(#38977,#38978,#38979,#38980,#38981,
#38982,#38983,#38984,#38985,#38986,#38987,#38988,#38989,#38990,#38991,#38992,
#38993,#38994,#38995,#38996,#38997,#38998,#38999,#39000,#39001,#39002,#39003,
#39004,#39005,#39006,#39007,#39008,#39009,#39010,#39011,#39012,#39013,#39014,
#39015,#39016,#39017,#39018,#39019,#39020,#39021,#39022,#39023,#39024,#39025,
#39026,#39027,#39028,#39029,#39030,#39031,#39032,#39033,#39034,#39035,#39036,
#39037,#39038,#39039,#39040,#39041,#39042,#39043,#39044,#39045,#39046,#39047,
#39048,#39049,#39050,#39051,#39052,#39053,#39054,#39055,#39056,#39057,#39058),
 .UNSPECIFIED.,.F.,.F.,(4,3,3,3,3,3,3,3,3,3,3,3,3,3,3,3,3,3,3,3,3,3,3,3,
3,3,3,4),(390.65265496374,390.729930386465,390.807215958564,390.884525701835,
390.96508487865,391.042526763526,391.120024575373,391.197626008844,391.206762409095,
391.283611032282,391.360365878679,391.437043218083,391.513659257858,391.590230156482,
391.66726588948,391.743808308186,391.820356644748,391.896925476196,391.974323112263,
392.051014193216,392.12876510684,392.206516020464,392.288683850341,392.370716624168,
392.452807892807,392.534533417735,392.61680755823,392.699081698725),
 .UNSPECIFIED.);
#353=B_SPLINE_CURVE_WITH_KNOTS('',3,(#39060,#39061,#39062,#39063,#39064,
#39065,#39066,#39067,#39068,#39069,#39070,#39071,#39072,#39073,#39074,#39075,
#39076,#39077,#39078,#39079,#39080,#39081,#39082,#39083,#39084,#39085,#39086,
#39087,#39088,#39089,#39090,#39091,#39092,#39093,#39094,#39095,#39096,#39097,
#39098,#39099,#39100,#39101,#39102,#39103,#39104,#39105,#39106,#39107,#39108,
#39109,#39110,#39111,#39112,#39113,#39114,#39115,#39116,#39117,#39118,#39119,
#39120,#39121,#39122,#39123,#39124,#39125,#39126,#39127,#39128,#39129,#39130,
#39131,#39132,#39133,#39134,#39135),.UNSPECIFIED.,.F.,.F.,(4,3,3,3,3,3,
3,3,3,3,3,3,3,3,3,3,3,3,3,3,3,3,3,3,3,4),(390.652559647909,390.735021251763,
390.817482189734,390.899942489219,390.982402177616,391.064861282318,391.147319830717,
391.229777850204,391.312235368165,391.398913263825,391.481380049661,391.563845163004,
391.64630871351,391.728770810807,391.811231564509,391.893691084206,391.976149479473,
392.058606859871,392.141073246137,392.223536448151,392.305996904431,392.388455053342,
392.470920658221,392.553380537436,392.6358446508,392.699081698724),
 .UNSPECIFIED.);
#354=B_SPLINE_CURVE_WITH_KNOTS('',3,(#39136,#39137,#39138,#39139,#39140,
#39141,#39142,#39143,#39144,#39145,#39146,#39147,#39148,#39149,#39150,#39151,
#39152,#39153,#39154,#39155,#39156,#39157,#39158,#39159,#39160,#39161,#39162,
#39163,#39164,#39165,#39166,#39167,#39168,#39169,#39170,#39171,#39172,#39173,
#39174,#39175,#39176,#39177,#39178,#39179,#39180,#39181,#39182,#39183,#39184,
#39185,#39186,#39187,#39188,#39189,#39190,#39191,#39192,#39193,#39194,#39195,
#39196,#39197,#39198,#39199,#39200,#39201,#39202,#39203,#39204,#39205,#39206,
#39207,#39208,#39209,#39210,#39211,#39212,#39213,#39214,#39215,#39216,#39217,
#39218,#39219,#39220,#39221,#39222,#39223,#39224,#39225,#39226,#39227,#39228,
#39229,#39230,#39231,#39232,#39233,#39234,#39235,#39236,#39237,#39238,#39239,
#39240,#39241,#39242,#39243,#39244,#39245,#39246,#39247,#39248,#39249,#39250,
#39251,#39252,#39253,#39254,#39255,#39256,#39257,#39258,#39259,#39260,#39261,
#39262,#39263,#39264,#39265,#39266,#39267,#39268,#39269,#39270,#39271,#39272,
#39273,#39274,#39275,#39276,#39277,#39278,#39279,#39280,#39281,#39282,#39283,
#39284,#39285,#39286,#39287,#39288,#39289,#39290,#39291,#39292,#39293,#39294,
#39295,#39296,#39297,#39298,#39299,#39300,#39301,#39302,#39303,#39304),
 .UNSPECIFIED.,.F.,.F.,(4,3,3,3,3,3,3,3,3,3,3,3,3,3,3,3,3,3,3,3,3,3,3,3,
3,3,3,3,3,3,3,3,3,3,3,3,3,3,3,3,3,3,3,3,3,3,3,3,3,3,3,3,3,3,3,3,4),(392.699081698724,
392.793961387981,392.889826204111,392.986708190667,393.00689192327,393.083755307922,
393.160525139732,393.237217675721,393.313849110887,393.390435591671,393.467293634127,
393.54385195709,393.620416291763,393.69700120489,393.774075886498,393.850782707367,
393.928041319344,394.005299931321,394.082830127781,394.160273222386,394.237644856442,
394.314960620011,394.392236062789,394.469496945209,394.546752250853,394.624016021147,
394.701302299632,394.778669112424,394.856077447131,394.933599003694,395.003707939372,
395.081238057435,395.158681086751,395.236052668577,395.313368392936,395.390643809498,
395.467904685523,395.545159996869,395.622423784961,395.699710093345,395.777076954951,
395.854485348883,395.932006981755,396.002115947423,396.078955451781,396.155705180829,
396.232381376134,396.30900022039,396.387270367678,396.463830766461,396.540385985712,
396.616950589475,396.69650329178,396.773165637115,396.849872557563,396.926668187919,
396.935161398696),.UNSPECIFIED.);
#355=B_SPLINE_CURVE_WITH_KNOTS('',3,(#39310,#39311,#39312,#39313,#39314,
#39315,#39316,#39317,#39318,#39319,#39320,#39321,#39322,#39323,#39324,#39325,
#39326,#39327,#39328,#39329,#39330,#39331,#39332,#39333,#39334,#39335,#39336,
#39337,#39338,#39339,#39340,#39341,#39342,#39343,#39344,#39345,#39346,#39347,
#39348,#39349,#39350,#39351,#39352,#39353,#39354,#39355,#39356,#39357,#39358,
#39359,#39360,#39361,#39362,#39363,#39364,#39365,#39366,#39367,#39368,#39369,
#39370,#39371,#39372,#39373,#39374,#39375,#39376,#39377,#39378,#39379,#39380,
#39381,#39382,#39383,#39384,#39385,#39386,#39387,#39388,#39389,#39390,#39391,
#39392,#39393,#39394,#39395,#39396,#39397,#39398,#39399,#39400,#39401,#39402,
#39403,#39404,#39405,#39406,#39407,#39408,#39409,#39410,#39411,#39412,#39413,
#39414,#39415,#39416,#39417,#39418,#39419,#39420,#39421,#39422,#39423,#39424,
#39425,#39426,#39427,#39428,#39429,#39430,#39431,#39432,#39433,#39434,#39435,
#39436,#39437,#39438,#39439,#39440,#39441,#39442,#39443,#39444,#39445,#39446,
#39447,#39448,#39449,#39450,#39451,#39452,#39453,#39454,#39455,#39456,#39457,
#39458,#39459,#39460,#39461,#39462,#39463,#39464,#39465,#39466),
 .UNSPECIFIED.,.F.,.F.,(4,3,3,3,3,3,3,3,3,3,3,3,3,3,3,3,3,3,3,3,3,3,3,3,
3,3,3,3,3,3,3,3,3,3,3,3,3,3,3,3,3,3,3,3,3,3,3,3,3,3,3,3,4),(398.982267005904,
399.06472921194,399.14719106968,399.229652585974,399.312113767671,399.394574621622,
399.477035154677,399.559495373683,399.641955285491,399.724414896949,399.806874214905,
399.889333246207,399.971791997704,400.054250476242,400.13670868867,400.219166641834,
400.301624342582,400.38408179776,400.466539014214,400.552551240716,400.63587558514,
400.718342190585,400.800807951827,400.883272896279,400.965737051355,401.048200444464,
401.130663103012,401.213125054405,401.295586326044,401.378046945328,401.460506939655,
401.542966336419,401.625425163015,401.707883446831,401.790341215259,401.872798495684,
401.956931731096,402.039397729187,402.121862105543,402.204324969805,402.286786431596,
402.369246600517,402.451705586152,402.53416349807,402.619759343595,402.702224080195,
402.784685852197,402.867145098039,402.949602256016,403.032064774297,403.114522445152,
403.196981235103,403.218930262269),.UNSPECIFIED.);
#356=B_SPLINE_CURVE_WITH_KNOTS('',3,(#39467,#39468,#39469,#39470,#39471,
#39472,#39473,#39474,#39475,#39476,#39477,#39478,#39479,#39480,#39481,#39482,
#39483,#39484,#39485,#39486,#39487,#39488,#39489,#39490,#39491,#39492,#39493,
#39494,#39495,#39496,#39497,#39498,#39499,#39500,#39501,#39502,#39503,#39504,
#39505,#39506,#39507,#39508,#39509,#39510,#39511,#39512,#39513,#39514,#39515,
#39516,#39517,#39518,#39519,#39520,#39521,#39522,#39523,#39524,#39525,#39526,
#39527,#39528,#39529,#39530,#39531,#39532,#39533,#39534,#39535,#39536,#39537,
#39538,#39539,#39540,#39541,#39542),.UNSPECIFIED.,.F.,.F.,(4,3,3,3,3,3,
3,3,3,3,3,3,3,3,3,3,3,3,3,3,3,3,3,3,3,4),(396.935744955089,397.018206558943,
397.100667496913,397.183127796399,397.265587484796,397.348046589498,397.430505137897,
397.512963157383,397.595420675345,397.682098570996,397.764565356832,397.847030470175,
397.929494020681,398.011956117978,398.09441687168,398.176876391377,398.259334786644,
398.341792167041,398.424258553308,398.506721755322,398.589182211602,398.671640360513,
398.754105965392,398.836565844606,398.91902995797,398.982267005763),
 .UNSPECIFIED.);
#357=B_SPLINE_CURVE_WITH_KNOTS('',3,(#39544,#39545,#39546,#39547,#39548,
#39549,#39550,#39551,#39552,#39553,#39554,#39555,#39556,#39557,#39558,#39559,
#39560,#39561,#39562,#39563,#39564,#39565,#39566,#39567,#39568,#39569,#39570,
#39571,#39572,#39573,#39574,#39575,#39576,#39577,#39578,#39579,#39580,#39581,
#39582,#39583,#39584,#39585,#39586,#39587,#39588,#39589,#39590,#39591,#39592,
#39593,#39594,#39595,#39596,#39597,#39598,#39599,#39600,#39601,#39602,#39603,
#39604,#39605,#39606,#39607,#39608,#39609,#39610,#39611,#39612,#39613,#39614,
#39615,#39616,#39617,#39618,#39619,#39620,#39621,#39622,#39623,#39624,#39625),
 .UNSPECIFIED.,.F.,.F.,(4,3,3,3,3,3,3,3,3,3,3,3,3,3,3,3,3,3,3,3,3,3,3,3,
3,3,3,4),(396.935161398696,397.000523955473,397.078118624907,397.155620891017,
397.233046376088,397.310410647465,397.387729228556,397.465024933027,397.542309977683,
397.619598369616,397.696904115142,397.774282155129,397.851697226874,397.929217841145,
397.998931963524,398.080418277957,398.161800360316,398.245884262125,398.327041580978,
398.408122364732,398.489112356766,398.49813596755,398.57854070701,398.659011250048,
398.739825189012,398.820496803775,398.901381904839,398.982267005904),
 .UNSPECIFIED.);
#358=B_SPLINE_CURVE_WITH_KNOTS('',3,(#39626,#39627,#39628,#39629,#39630,
#39631,#39632,#39633,#39634,#39635,#39636,#39637,#39638,#39639,#39640,#39641,
#39642,#39643,#39644,#39645,#39646,#39647,#39648,#39649,#39650,#39651,#39652,
#39653,#39654,#39655,#39656,#39657,#39658,#39659,#39660,#39661,#39662,#39663,
#39664,#39665,#39666,#39667,#39668,#39669,#39670,#39671,#39672,#39673,#39674,
#39675,#39676,#39677,#39678,#39679,#39680,#39681,#39682,#39683,#39684,#39685,
#39686,#39687,#39688,#39689,#39690,#39691,#39692,#39693,#39694,#39695,#39696,
#39697,#39698,#39699,#39700,#39701,#39702,#39703,#39704,#39705,#39706,#39707,
#39708,#39709,#39710,#39711,#39712,#39713,#39714,#39715,#39716,#39717,#39718,
#39719,#39720,#39721,#39722,#39723,#39724,#39725,#39726,#39727,#39728,#39729,
#39730,#39731,#39732,#39733,#39734,#39735,#39736,#39737,#39738,#39739,#39740,
#39741,#39742,#39743,#39744,#39745,#39746,#39747,#39748,#39749,#39750,#39751,
#39752,#39753,#39754,#39755,#39756,#39757,#39758,#39759,#39760,#39761,#39762,
#39763,#39764,#39765,#39766,#39767,#39768,#39769,#39770,#39771,#39772,#39773,
#39774,#39775,#39776,#39777,#39778,#39779,#39780,#39781,#39782,#39783,#39784,
#39785,#39786,#39787,#39788,#39789,#39790,#39791,#39792,#39793,#39794),
 .UNSPECIFIED.,.F.,.F.,(4,3,3,3,3,3,3,3,3,3,3,3,3,3,3,3,3,3,3,3,3,3,3,3,
3,3,3,3,3,3,3,3,3,3,3,3,3,3,3,3,3,3,3,3,3,3,3,3,3,3,3,3,3,3,3,3,4),(398.982267006007,
398.997339971575,399.074868124784,399.152314999745,399.229696178453,399.307027195914,
399.384323550744,399.46161385108,399.538903758818,399.616207280817,399.693538428944,
399.770957918765,399.848423277186,399.926008663485,399.995747979626,400.072611364278,
400.149381196088,400.226073732077,400.302705167243,400.379291648027,400.456149690483,
400.532708013447,400.609272348119,400.685857261246,400.762931942854,400.839638763723,
400.9168973757,400.994155987677,401.071686184137,401.149129278742,401.226500912798,
401.303816676367,401.381092119145,401.458353001565,401.535608307209,401.612872077503,
401.690158355987,401.767525168779,401.844933503486,401.922455060049,401.992563995728,
402.070094113791,402.147537143107,402.224908724933,402.302224449293,402.379499865854,
402.45676074188,402.534016053226,402.611279841318,402.688566149701,402.765933011308,
402.84334140524,402.920863038112,402.990972003779,403.067812533307,403.144549620671,
403.219566237065),.UNSPECIFIED.);
#359=B_SPLINE_CURVE_WITH_KNOTS('',3,(#39800,#39801,#39802,#39803,#39804,
#39805,#39806,#39807,#39808,#39809,#39810,#39811,#39812,#39813,#39814,#39815,
#39816,#39817,#39818,#39819,#39820,#39821,#39822,#39823,#39824,#39825,#39826,
#39827,#39828,#39829,#39830,#39831,#39832,#39833,#39834,#39835,#39836,#39837,
#39838,#39839,#39840,#39841,#39842,#39843,#39844,#39845,#39846,#39847,#39848,
#39849,#39850,#39851,#39852,#39853,#39854,#39855,#39856,#39857,#39858,#39859,
#39860,#39861,#39862,#39863,#39864,#39865,#39866,#39867,#39868,#39869,#39870,
#39871,#39872,#39873,#39874,#39875,#39876,#39877,#39878,#39879,#39880,#39881,
#39882,#39883,#39884,#39885,#39886,#39887,#39888,#39889,#39890,#39891,#39892,
#39893,#39894,#39895,#39896,#39897,#39898,#39899,#39900,#39901,#39902,#39903,
#39904,#39905,#39906,#39907,#39908,#39909,#39910,#39911,#39912,#39913,#39914,
#39915,#39916,#39917,#39918,#39919,#39920,#39921,#39922,#39923,#39924,#39925,
#39926,#39927,#39928,#39929,#39930,#39931,#39932,#39933,#39934,#39935,#39936,
#39937,#39938,#39939,#39940,#39941,#39942,#39943,#39944,#39945,#39946,#39947,
#39948,#39949,#39950,#39951,#39952,#39953,#39954,#39955,#39956,#39957,#39958,
#39959,#39960,#39961,#39962,#39963,#39964,#39965,#39966,#39967,#39968),
 .UNSPECIFIED.,.F.,.F.,(4,3,3,3,3,3,3,3,3,3,3,3,3,3,3,3,3,3,3,3,3,3,3,3,
3,3,3,3,3,3,3,3,3,3,3,3,3,3,3,3,3,3,3,3,3,3,3,3,3,3,3,3,3,3,3,3,4),(405.266047532152,
405.342168931996,405.418201910201,405.494163189336,405.570069420944,405.649194065781,
405.72505049336,405.800905647069,405.876774507432,405.952672063747,406.028652258912,
406.104681216099,406.180812293953,406.203066579635,406.280584131253,406.358014350673,
406.435372893568,406.512675364155,406.589937326106,406.667184551888,406.744426063095,
406.821675913328,406.898948158241,406.976301116212,407.053695508521,407.131203836189,
407.202820191005,407.280337560201,407.357767627653,407.435126048922,407.512428428137,
407.5896903289,407.666937539591,407.744179063809,407.821428955156,407.898701269299,
407.976054340525,408.053448870277,408.130957375239,408.202573802374,408.279394999529,
408.356126961743,408.432785939891,408.509388126352,408.585949668233,408.662996886422,
408.739541061066,408.816095341111,408.892674306091,408.970087583004,409.046799063311,
409.124563238527,409.202327413743,409.279899717308,409.357391118293,409.434795562625,
409.502619229227),.UNSPECIFIED.);
#360=B_SPLINE_CURVE_WITH_KNOTS('',3,(#39969,#39970,#39971,#39972,#39973,
#39974,#39975,#39976,#39977,#39978,#39979,#39980,#39981,#39982,#39983,#39984,
#39985,#39986,#39987,#39988,#39989,#39990,#39991,#39992,#39993,#39994,#39995,
#39996,#39997,#39998,#39999,#40000,#40001,#40002,#40003,#40004,#40005,#40006,
#40007,#40008,#40009,#40010,#40011,#40012,#40013,#40014,#40015,#40016,#40017,
#40018,#40019,#40020,#40021,#40022,#40023,#40024,#40025,#40026,#40027,#40028,
#40029,#40030,#40031,#40032,#40033,#40034,#40035,#40036,#40037,#40038,#40039,
#40040,#40041,#40042,#40043,#40044),.UNSPECIFIED.,.F.,.F.,(4,3,3,3,3,3,
3,3,3,3,3,3,3,3,3,3,3,3,3,3,3,3,3,3,3,4),(403.218930262269,403.301391865812,
403.383852803484,403.466313102684,403.548772790808,403.631231895249,403.7136904434,
403.796148462651,403.878605980389,403.965281519416,404.047748304511,404.130213417161,
404.21267696702,404.295139063719,404.377599816867,404.460059336059,404.542517730868,
404.624975110854,404.707441495662,404.789904696405,404.872365151602,404.954823299618,
405.037288901668,405.119748778805,405.202212886862,405.26541460481),
 .UNSPECIFIED.);
#361=B_SPLINE_CURVE_WITH_KNOTS('',3,(#40046,#40047,#40048,#40049,#40050,
#40051,#40052,#40053,#40054,#40055,#40056,#40057,#40058,#40059,#40060,#40061,
#40062,#40063,#40064,#40065,#40066,#40067,#40068,#40069,#40070,#40071,#40072,
#40073,#40074,#40075,#40076,#40077,#40078,#40079,#40080,#40081,#40082,#40083,
#40084,#40085,#40086,#40087,#40088,#40089,#40090,#40091,#40092,#40093,#40094,
#40095,#40096,#40097,#40098,#40099,#40100,#40101,#40102,#40103,#40104,#40105,
#40106,#40107,#40108,#40109,#40110,#40111,#40112,#40113,#40114,#40115,#40116,
#40117,#40118,#40119,#40120,#40121,#40122,#40123,#40124),.UNSPECIFIED.,
 .F.,.F.,(4,3,3,3,3,3,3,3,3,3,3,3,3,3,3,3,3,3,3,3,3,3,3,3,3,3,4),(403.219566237065,
403.29618493328,403.372762816884,403.449839966252,403.526400016109,403.602969984034,
403.67956443912,403.757018332297,403.833744806059,403.911562408944,403.98938001183,
404.066974681264,404.144476947374,404.221902432444,404.299266703822,404.376585284913,
404.453880989385,404.531166034041,404.608454425974,404.6857601715,404.763138211487,
404.840553283232,404.918073897503,404.987788019881,405.080944670191,405.173367791108,
405.265452312954),.UNSPECIFIED.);
#362=B_SPLINE_CURVE_WITH_KNOTS('',3,(#40125,#40126,#40127,#40128,#40129,
#40130,#40131,#40132,#40133,#40134,#40135,#40136,#40137,#40138,#40139,#40140,
#40141,#40142,#40143,#40144,#40145,#40146,#40147,#40148,#40149,#40150,#40151,
#40152,#40153,#40154,#40155,#40156,#40157,#40158,#40159,#40160,#40161,#40162,
#40163,#40164,#40165,#40166,#40167,#40168,#40169,#40170,#40171,#40172,#40173,
#40174,#40175,#40176,#40177,#40178,#40179,#40180,#40181,#40182,#40183,#40184,
#40185,#40186,#40187,#40188,#40189,#40190,#40191,#40192,#40193,#40194,#40195,
#40196,#40197,#40198,#40199,#40200,#40201,#40202,#40203,#40204,#40205,#40206,
#40207,#40208,#40209,#40210,#40211,#40212,#40213,#40214,#40215,#40216,#40217,
#40218,#40219,#40220,#40221,#40222,#40223,#40224,#40225,#40226,#40227,#40228,
#40229,#40230,#40231,#40232,#40233,#40234,#40235,#40236,#40237,#40238,#40239,
#40240,#40241,#40242,#40243,#40244,#40245,#40246,#40247,#40248,#40249,#40250,
#40251,#40252,#40253,#40254,#40255,#40256,#40257,#40258,#40259,#40260,#40261,
#40262,#40263,#40264,#40265,#40266,#40267,#40268,#40269,#40270,#40271,#40272,
#40273,#40274,#40275,#40276,#40277,#40278,#40279,#40280,#40281,#40282,#40283,
#40284,#40285,#40286,#40287,#40288,#40289,#40290,#40291,#40292,#40293),
 .UNSPECIFIED.,.F.,.F.,(4,3,3,3,3,3,3,3,3,3,3,3,3,3,3,3,3,3,3,3,3,3,3,3,
3,3,3,3,3,3,3,3,3,3,3,3,3,3,3,3,3,3,3,3,3,3,3,3,3,3,3,3,3,3,3,3,4),(405.265452313083,
405.339961026927,405.414439462604,405.486992023906,405.568005130196,405.649093824469,
405.733369375335,405.814678841724,405.896065742935,405.977572881699,405.986196027932,
406.063724181141,406.141171056103,406.21855223481,406.295883252271,406.373179607101,
406.450469907437,406.527759815175,406.605063337174,406.682394485301,406.759813975122,
406.837279333544,406.914864719842,406.984604035983,407.061467420635,407.138237252445,
407.214929788433,407.2915612236,407.368147704383,407.44500574684,407.521564069803,
407.598128404475,407.674713317602,407.75178799921,407.828494820079,407.905753432056,
407.983012044034,408.060542240494,408.137985335099,408.215356969155,408.292672732723,
408.369948175502,408.447209057922,408.524464363566,408.60172813386,408.679014412345,
408.756381225137,408.833789559843,408.911311116406,408.981420052084,409.058948032863,
409.136392455252,409.21376749302,409.291079443884,409.368354321232,409.445611213136,
409.50212192641),.UNSPECIFIED.);
#363=B_SPLINE_CURVE_WITH_KNOTS('',3,(#40299,#40300,#40301,#40302,#40303,
#40304,#40305,#40306,#40307,#40308,#40309,#40310,#40311,#40312,#40313,#40314,
#40315,#40316,#40317,#40318,#40319,#40320,#40321,#40322,#40323,#40324,#40325,
#40326,#40327,#40328,#40329,#40330,#40331,#40332,#40333,#40334,#40335,#40336,
#40337,#40338,#40339,#40340,#40341,#40342,#40343,#40344,#40345,#40346,#40347,
#40348,#40349,#40350,#40351,#40352,#40353,#40354,#40355,#40356,#40357,#40358,
#40359,#40360,#40361,#40362,#40363,#40364,#40365,#40366,#40367,#40368,#40369,
#40370,#40371,#40372,#40373,#40374,#40375,#40376,#40377,#40378,#40379,#40380,
#40381,#40382,#40383,#40384,#40385,#40386,#40387,#40388,#40389,#40390,#40391,
#40392,#40393,#40394,#40395,#40396,#40397,#40398,#40399,#40400,#40401,#40402,
#40403,#40404,#40405,#40406,#40407,#40408,#40409,#40410,#40411,#40412,#40413,
#40414,#40415,#40416,#40417,#40418,#40419,#40420,#40421,#40422,#40423,#40424,
#40425,#40426,#40427,#40428,#40429,#40430,#40431,#40432,#40433,#40434,#40435,
#40436,#40437,#40438,#40439,#40440,#40441,#40442,#40443,#40444,#40445,#40446,
#40447,#40448,#40449,#40450,#40451,#40452,#40453,#40454,#40455),
 .UNSPECIFIED.,.F.,.F.,(4,3,3,3,3,3,3,3,3,3,3,3,3,3,3,3,3,3,3,3,3,3,3,3,
3,3,3,3,3,3,3,3,3,3,3,3,3,3,3,3,3,3,3,3,3,3,3,3,3,3,3,3,4),(411.548637620263,
411.631099826299,411.713561684039,411.796023200333,411.87848438203,411.960945235981,
412.043405769036,412.125865988042,412.20832589985,412.290785511308,412.373244829264,
412.455703860566,412.538162612063,412.620621090601,412.703079303029,412.785537256194,
412.867994956942,412.950452412119,413.032909628574,413.118921855076,413.202246199499,
413.284712804945,413.367178566186,413.449643510639,413.532107665714,413.614571058823,
413.697033717372,413.779495668765,413.861956940403,413.944417559688,414.026877554014,
414.109336950779,414.191795777374,414.274254061191,414.356711829618,414.439169110044,
414.523302345455,414.605768343547,414.688232719902,414.770695584164,414.853157045955,
414.935617214876,415.018076200512,415.100534112429,415.186129957954,415.268594694554,
415.351056466556,415.433515712398,415.515972870375,415.598435388656,415.680893059511,
415.763351849462,415.785300876628),.UNSPECIFIED.);
#364=B_SPLINE_CURVE_WITH_KNOTS('',3,(#40456,#40457,#40458,#40459,#40460,
#40461,#40462,#40463,#40464,#40465,#40466,#40467,#40468,#40469,#40470,#40471,
#40472,#40473,#40474,#40475,#40476,#40477,#40478,#40479,#40480,#40481,#40482,
#40483,#40484,#40485,#40486,#40487,#40488,#40489,#40490,#40491,#40492,#40493,
#40494,#40495,#40496,#40497,#40498,#40499,#40500,#40501,#40502,#40503,#40504,
#40505,#40506,#40507,#40508,#40509,#40510,#40511,#40512,#40513,#40514,#40515,
#40516,#40517,#40518,#40519,#40520,#40521,#40522,#40523,#40524,#40525,#40526,
#40527,#40528,#40529,#40530,#40531,#40532,#40533,#40534,#40535,#40536,#40537),
 .UNSPECIFIED.,.F.,.F.,(4,3,3,3,3,3,3,3,3,3,3,3,3,3,3,3,3,3,3,3,3,3,3,3,
3,3,3,4),(409.502619229227,409.579929720954,409.657698633974,409.734970961888,
409.812244860335,409.889534347183,409.967671016666,410.045068067043,410.123574546078,
410.202081025113,410.283564998068,410.364944362208,410.449197729356,410.530351224527,
410.611427902487,410.692413330278,410.701957830797,410.782966226701,410.864050483532,
410.948496521769,411.029802603476,411.111186393244,411.192691054272,411.201834636482,
411.289530195866,411.376982381924,411.463959432209,411.548637620263),
 .UNSPECIFIED.);
#365=B_SPLINE_CURVE_WITH_KNOTS('',3,(#40539,#40540,#40541,#40542,#40543,
#40544,#40545,#40546,#40547,#40548,#40549,#40550,#40551,#40552,#40553,#40554,
#40555,#40556,#40557,#40558,#40559,#40560,#40561,#40562,#40563,#40564,#40565,
#40566,#40567,#40568,#40569,#40570,#40571,#40572,#40573,#40574,#40575,#40576,
#40577,#40578,#40579,#40580,#40581,#40582,#40583,#40584,#40585,#40586,#40587,
#40588,#40589,#40590,#40591,#40592,#40593,#40594,#40595,#40596,#40597,#40598,
#40599,#40600,#40601,#40602,#40603,#40604,#40605,#40606,#40607,#40608,#40609,
#40610,#40611,#40612,#40613,#40614,#40615,#40616,#40617,#40618,#40619,#40620),
 .UNSPECIFIED.,.F.,.F.,(4,3,3,3,3,3,3,3,3,3,3,3,3,3,3,3,3,3,3,3,3,3,3,3,
3,3,3,4),(409.50212192641,409.579382058547,409.656660938385,409.737452718823,
409.814850708878,409.89230004659,409.969847131038,409.979828060135,410.056664092258,
410.133411107985,410.210085345548,410.28670298507,410.363280161696,410.440149650008,
410.51670975253,410.593280049678,410.6698751107,410.746965350071,410.823692546653,
410.900964307419,410.978236068186,411.058503823145,411.13865788409,411.218708071292,
411.301190458535,411.381034500472,411.464836060367,411.548637620263),
 .UNSPECIFIED.);
#366=B_SPLINE_CURVE_WITH_KNOTS('',3,(#40621,#40622,#40623,#40624,#40625,
#40626,#40627,#40628,#40629,#40630,#40631,#40632,#40633,#40634,#40635,#40636,
#40637,#40638,#40639,#40640,#40641,#40642,#40643,#40644,#40645,#40646,#40647,
#40648,#40649,#40650,#40651,#40652,#40653,#40654,#40655,#40656,#40657,#40658,
#40659,#40660,#40661,#40662,#40663,#40664,#40665,#40666,#40667,#40668,#40669,
#40670,#40671,#40672,#40673,#40674,#40675,#40676,#40677,#40678,#40679,#40680,
#40681,#40682,#40683,#40684,#40685,#40686,#40687,#40688,#40689,#40690,#40691,
#40692,#40693,#40694,#40695,#40696,#40697,#40698,#40699,#40700,#40701,#40702,
#40703,#40704,#40705,#40706,#40707,#40708,#40709,#40710,#40711,#40712,#40713,
#40714,#40715,#40716,#40717,#40718,#40719,#40720,#40721,#40722,#40723,#40724,
#40725,#40726,#40727,#40728,#40729,#40730,#40731,#40732,#40733,#40734,#40735,
#40736,#40737,#40738,#40739,#40740,#40741,#40742,#40743,#40744,#40745,#40746,
#40747,#40748,#40749,#40750,#40751,#40752,#40753,#40754,#40755,#40756,#40757,
#40758,#40759,#40760,#40761,#40762,#40763,#40764,#40765,#40766,#40767,#40768,
#40769,#40770,#40771,#40772,#40773,#40774,#40775,#40776,#40777,#40778,#40779,
#40780,#40781,#40782,#40783,#40784,#40785,#40786,#40787,#40788,#40789,#40790,
#40791,#40792),.UNSPECIFIED.,.F.,.F.,(4,3,3,3,3,3,3,3,3,3,3,3,3,3,3,3,3,
3,3,3,3,3,3,3,3,3,3,3,3,3,3,3,3,3,3,3,3,3,3,3,3,3,3,3,3,3,3,3,3,3,3,3,3,
3,3,3,3,4),(411.548637620392,411.631116923562,411.717498711731,411.800360156989,
411.883345085508,411.966503474013,411.976644076237,412.05813039067,412.139512473029,
412.223596374837,412.30475369369,412.385834477445,412.466824469478,412.475848080263,
412.556861186553,412.637949880827,412.722225431692,412.803534898082,412.884921799293,
412.966428938058,412.975052084288,413.052580237497,413.130027112458,413.207408291166,
413.284739308626,413.362035663457,413.439325963793,413.516615871531,413.593919393529,
413.671250541656,413.748670031477,413.826135389899,413.903720776197,413.973460092339,
414.050323476991,414.127093308801,414.203785844789,414.280417279956,414.35700376074,
414.433861803196,414.510420126159,414.586984460832,414.663569373959,414.740644055567,
414.817350876436,414.894609488413,414.97186810039,415.04940838302,415.126859511665,
415.20423713556,415.281549096136,415.358824470978,415.436077322192,415.513321696487,
415.590593756579,415.667880944835,415.745225934373,415.784711144052),
 .UNSPECIFIED.);
#367=B_SPLINE_CURVE_WITH_KNOTS('',3,(#40798,#40799,#40800,#40801,#40802,
#40803,#40804,#40805,#40806,#40807,#40808,#40809,#40810,#40811,#40812,#40813,
#40814,#40815,#40816,#40817,#40818,#40819,#40820,#40821,#40822,#40823,#40824,
#40825,#40826,#40827,#40828,#40829,#40830,#40831,#40832,#40833,#40834,#40835,
#40836,#40837,#40838,#40839,#40840,#40841,#40842,#40843,#40844,#40845,#40846,
#40847,#40848,#40849,#40850,#40851,#40852,#40853,#40854,#40855,#40856,#40857,
#40858,#40859,#40860,#40861,#40862,#40863,#40864,#40865,#40866,#40867,#40868,
#40869,#40870,#40871,#40872,#40873,#40874,#40875,#40876,#40877,#40878,#40879,
#40880,#40881,#40882,#40883,#40884,#40885,#40886,#40887,#40888,#40889,#40890,
#40891,#40892,#40893,#40894,#40895,#40896,#40897,#40898,#40899,#40900,#40901,
#40902,#40903,#40904,#40905,#40906,#40907,#40908,#40909,#40910,#40911,#40912,
#40913,#40914,#40915,#40916,#40917,#40918,#40919,#40920,#40921,#40922,#40923,
#40924,#40925,#40926,#40927,#40928,#40929,#40930,#40931,#40932,#40933,#40934,
#40935,#40936,#40937,#40938,#40939,#40940,#40941,#40942,#40943,#40944,#40945,
#40946,#40947,#40948,#40949,#40950,#40951,#40952,#40953,#40954,#40955,#40956,
#40957,#40958,#40959,#40960,#40961,#40962,#40963,#40964,#40965,#40966),
 .UNSPECIFIED.,.F.,.F.,(4,3,3,3,3,3,3,3,3,3,3,3,3,3,3,3,3,3,3,3,3,3,3,3,
3,3,3,3,3,3,3,3,3,3,3,3,3,3,3,3,3,3,3,3,3,3,3,3,3,3,3,3,3,3,3,3,4),(417.831822927443,
417.917729261325,418.004018421998,418.090499078249,418.17721376897,418.200109916068,
418.277625694331,418.355059994742,418.432428413169,418.509746498319,418.587029762363,
418.664306846675,418.741583427162,418.81887352256,418.896191156564,418.973597362888,
419.051049372202,419.128622180524,419.199863527437,419.276712150624,419.353466997021,
419.430144336426,419.506760376201,419.583331274826,419.660367007823,419.736909426529,
419.813457763091,419.890026594539,419.967424230606,420.044115311559,420.121866225182,
420.199617138806,420.277134690424,420.354564909844,420.431923452739,420.509225923326,
420.586487885276,420.663735111059,420.740976622266,420.818226472499,420.895498717412,
420.972851675383,421.050246067692,421.12775439536,421.199370750176,421.276895112083,
421.354330721744,421.431693240297,421.511244244508,421.58850615986,421.665746689699,
421.742979892556,421.824260237913,421.901548057031,421.978864899425,422.05624938853,
422.068101273987),.UNSPECIFIED.);
#368=B_SPLINE_CURVE_WITH_KNOTS('',3,(#40967,#40968,#40969,#40970,#40971,
#40972,#40973,#40974,#40975,#40976,#40977,#40978,#40979,#40980,#40981,#40982,
#40983,#40984,#40985,#40986,#40987,#40988,#40989,#40990,#40991,#40992,#40993,
#40994,#40995,#40996,#40997,#40998,#40999,#41000,#41001,#41002,#41003,#41004,
#41005,#41006,#41007,#41008,#41009,#41010,#41011,#41012,#41013,#41014,#41015,
#41016,#41017,#41018,#41019,#41020,#41021,#41022,#41023,#41024,#41025,#41026,
#41027,#41028,#41029,#41030,#41031,#41032,#41033,#41034,#41035,#41036,#41037,
#41038,#41039,#41040,#41041,#41042),.UNSPECIFIED.,.F.,.F.,(4,3,3,3,3,3,
3,3,3,3,3,3,3,3,3,3,3,3,3,3,3,3,3,3,3,4),(415.785300876628,415.867762480482,
415.950223418452,416.032683717938,416.115143406335,416.197602511037,416.280061059436,
416.362519078922,416.444976596884,416.531654492544,416.614121278379,416.696586391723,
416.779049942228,416.861512039526,416.943972793228,417.026432312925,417.108890708192,
417.191348088589,417.273814474856,417.35627767687,417.43873813315,417.521196282061,
417.60366188694,417.686121766155,417.768585879518,417.831822927443),
 .UNSPECIFIED.);
#369=B_SPLINE_CURVE_WITH_KNOTS('',3,(#41044,#41045,#41046,#41047,#41048,
#41049,#41050,#41051,#41052,#41053,#41054,#41055,#41056,#41057,#41058,#41059,
#41060,#41061,#41062,#41063,#41064,#41065,#41066,#41067,#41068,#41069,#41070,
#41071,#41072,#41073,#41074,#41075,#41076,#41077,#41078,#41079,#41080,#41081,
#41082,#41083,#41084,#41085,#41086,#41087,#41088,#41089,#41090,#41091,#41092,
#41093,#41094,#41095,#41096,#41097,#41098,#41099,#41100,#41101,#41102,#41103,
#41104,#41105,#41106,#41107,#41108,#41109,#41110,#41111,#41112,#41113,#41114,
#41115,#41116,#41117,#41118,#41119,#41120,#41121,#41122,#41123,#41124,#41125,
#41126,#41127,#41128),.UNSPECIFIED.,.F.,.F.,(4,3,3,3,3,3,3,3,3,3,3,3,3,
3,3,3,3,3,3,3,3,3,3,3,3,3,3,3,4),(415.784711144052,415.862145526228,415.939682750499,
415.970276108441,416.047806226504,416.12524925582,416.202620837646,416.279936562006,
416.357211978567,416.434472854593,416.511728165939,416.588991954031,416.666278262415,
416.743645124021,416.821053517953,416.898575150825,416.968684116492,417.044412302149,
417.120052278303,417.19562098838,417.275021363452,417.350500604425,417.425964305112,
417.501427624748,417.576905721553,417.652447414651,417.728026121681,417.803692848326,
417.830823988957),.UNSPECIFIED.);
#370=B_SPLINE_CURVE_WITH_KNOTS('',3,(#41129,#41130,#41131,#41132,#41133,
#41134,#41135,#41136,#41137,#41138,#41139,#41140,#41141,#41142,#41143,#41144,
#41145,#41146,#41147,#41148,#41149,#41150,#41151,#41152,#41153,#41154,#41155,
#41156,#41157,#41158,#41159,#41160,#41161,#41162,#41163,#41164,#41165,#41166,
#41167,#41168,#41169,#41170,#41171,#41172,#41173,#41174,#41175,#41176,#41177,
#41178,#41179,#41180,#41181,#41182,#41183,#41184,#41185,#41186,#41187,#41188,
#41189,#41190,#41191,#41192,#41193,#41194,#41195,#41196,#41197,#41198,#41199,
#41200,#41201,#41202,#41203,#41204,#41205,#41206,#41207,#41208,#41209,#41210,
#41211,#41212,#41213,#41214,#41215,#41216,#41217,#41218,#41219,#41220,#41221,
#41222,#41223,#41224,#41225,#41226,#41227,#41228,#41229,#41230,#41231,#41232,
#41233,#41234,#41235,#41236,#41237,#41238,#41239,#41240,#41241,#41242,#41243,
#41244,#41245,#41246,#41247,#41248,#41249,#41250,#41251,#41252,#41253,#41254,
#41255,#41256,#41257,#41258,#41259,#41260,#41261,#41262,#41263,#41264,#41265,
#41266,#41267,#41268,#41269,#41270,#41271,#41272,#41273,#41274,#41275,#41276,
#41277,#41278,#41279,#41280,#41281,#41282,#41283,#41284,#41285),
 .UNSPECIFIED.,.F.,.F.,(4,3,3,3,3,3,3,3,3,3,3,3,3,3,3,3,3,3,3,3,3,3,3,3,
3,3,3,3,3,3,3,3,3,3,3,3,3,3,3,3,3,3,3,3,3,3,3,3,3,3,3,3,4),(417.831822927443,
417.914285133479,417.996746991219,418.079208507513,418.16166968921,418.244130543161,
418.326591076216,418.409051295222,418.49151120703,418.573970818488,418.656430136444,
418.738889167746,418.821347919243,418.903806397781,418.986264610209,419.068722563373,
419.151180264121,419.233637719299,419.316094935754,419.402107162255,419.485431506679,
419.567898112124,419.650363873366,419.732828817818,419.815292972894,419.897756366003,
419.980219024552,420.062680975944,420.145142247583,420.227602866867,420.310062861194,
420.392522257958,420.474981084554,420.55743936837,420.639897136798,420.722354417223,
420.806487652635,420.888953650726,420.971418027082,421.053880891344,421.136342353135,
421.218802522056,421.301261507691,421.383719419608,421.469315265133,421.551780001734,
421.634241773735,421.716701019578,421.799158177554,421.881620695836,421.964078366691,
422.046537156641,422.068486183807),.UNSPECIFIED.);
#371=B_SPLINE_CURVE_WITH_KNOTS('',3,(#41291,#41292,#41293,#41294,#41295,
#41296,#41297,#41298,#41299,#41300,#41301,#41302,#41303,#41304,#41305,#41306,
#41307,#41308,#41309,#41310,#41311,#41312,#41313,#41314,#41315,#41316,#41317,
#41318,#41319,#41320,#41321,#41322,#41323,#41324,#41325,#41326,#41327,#41328,
#41329,#41330,#41331,#41332,#41333,#41334,#41335,#41336,#41337,#41338,#41339,
#41340,#41341,#41342,#41343,#41344,#41345,#41346,#41347,#41348,#41349,#41350,
#41351,#41352,#41353,#41354,#41355,#41356,#41357,#41358,#41359,#41360,#41361,
#41362,#41363,#41364,#41365,#41366,#41367,#41368,#41369,#41370,#41371,#41372,
#41373,#41374,#41375,#41376,#41377,#41378,#41379,#41380,#41381,#41382,#41383,
#41384,#41385,#41386,#41387,#41388,#41389,#41390,#41391,#41392,#41393,#41394,
#41395,#41396,#41397,#41398,#41399,#41400,#41401,#41402,#41403,#41404,#41405,
#41406,#41407,#41408,#41409,#41410,#41411,#41412,#41413,#41414,#41415,#41416,
#41417,#41418,#41419,#41420,#41421,#41422,#41423,#41424,#41425,#41426,#41427,
#41428,#41429,#41430,#41431,#41432,#41433,#41434,#41435,#41436,#41437,#41438,
#41439,#41440,#41441,#41442,#41443,#41444,#41445,#41446,#41447),
 .UNSPECIFIED.,.F.,.F.,(4,3,3,3,3,3,3,3,3,3,3,3,3,3,3,3,3,3,3,3,3,3,3,3,
3,3,3,3,3,3,3,3,3,3,3,3,3,3,3,3,3,3,3,3,3,3,3,3,3,3,3,3,4),(424.115008234622,
424.197470440658,424.279932298398,424.362393814692,424.444854996389,424.52731585034,
424.609776383395,424.692236602401,424.774696514209,424.857156125667,424.939615443623,
425.022074474925,425.104533226422,425.18699170496,425.269449917388,425.351907870552,
425.4343655713,425.516823026478,425.599280242933,425.685292469434,425.768616813858,
425.851083419303,425.933549180545,426.016014124997,426.098478280073,426.180941673182,
426.263404331731,426.345866283123,426.428327554762,426.510788174046,426.593248168373,
426.675707565138,426.758166391733,426.840624675549,426.923082443977,427.005539724402,
427.089672959814,427.172138957905,427.254603334261,427.337066198523,427.419527660314,
427.501987829235,427.584446814871,427.666904726788,427.752500572313,427.834965308913,
427.917427080915,427.999886326757,428.082343484734,428.164806003015,428.24726367387,
428.329722463821,428.351671490987),.UNSPECIFIED.);
#372=B_SPLINE_CURVE_WITH_KNOTS('',3,(#41448,#41449,#41450,#41451,#41452,
#41453,#41454,#41455,#41456,#41457,#41458,#41459,#41460,#41461,#41462,#41463,
#41464,#41465,#41466,#41467,#41468,#41469,#41470,#41471,#41472,#41473,#41474,
#41475,#41476,#41477,#41478,#41479,#41480,#41481,#41482,#41483,#41484,#41485,
#41486,#41487,#41488,#41489,#41490,#41491,#41492,#41493,#41494,#41495,#41496,
#41497,#41498,#41499,#41500,#41501,#41502,#41503,#41504,#41505,#41506,#41507,
#41508,#41509,#41510,#41511,#41512,#41513,#41514,#41515,#41516,#41517,#41518,
#41519,#41520,#41521,#41522,#41523,#41524,#41525,#41526,#41527,#41528,#41529),
 .UNSPECIFIED.,.F.,.F.,(4,3,3,3,3,3,3,3,3,3,3,3,3,3,3,3,3,3,3,3,3,3,3,3,
3,3,3,4),(422.068101273987,422.145616415958,422.199124361545,422.2759455587,
422.352677520914,422.429336499062,422.505938685523,422.582500227404,422.659547445593,
422.736091620237,422.812645900282,422.889224865262,422.966638142175,423.043349622482,
423.121113797699,423.198877972915,423.275729950139,423.352489963892,423.429174304041,
423.505799199108,423.582382255955,423.658943276863,423.735496866981,423.812057624682,
423.888677214912,423.965326054594,424.042071142312,424.114488541238),
 .UNSPECIFIED.);
#373=B_SPLINE_CURVE_WITH_KNOTS('',3,(#41531,#41532,#41533,#41534,#41535,
#41536,#41537,#41538,#41539,#41540,#41541,#41542,#41543,#41544,#41545,#41546,
#41547,#41548,#41549,#41550,#41551,#41552,#41553,#41554,#41555,#41556,#41557,
#41558,#41559,#41560,#41561,#41562,#41563,#41564,#41565,#41566,#41567,#41568,
#41569,#41570,#41571,#41572,#41573,#41574,#41575,#41576,#41577,#41578,#41579,
#41580,#41581,#41582,#41583,#41584,#41585,#41586,#41587,#41588,#41589,#41590,
#41591,#41592,#41593,#41594,#41595,#41596,#41597,#41598,#41599,#41600,#41601,
#41602,#41603,#41604,#41605,#41606),.UNSPECIFIED.,.F.,.F.,(4,3,3,3,3,3,
3,3,3,3,3,3,3,3,3,3,3,3,3,3,3,3,3,3,3,4),(422.068486183807,422.150947787661,
422.233408725631,422.315869025117,422.398328713514,422.480787818216,422.563246366615,
422.645704386102,422.728161904063,422.814839799723,422.897306585559,422.979771698902,
423.062235249407,423.144697346705,423.227158100407,423.309617620104,423.392076015371,
423.474533395768,423.556999782035,423.639462984048,423.721923440329,423.80438158924,
423.886847194119,423.969307073333,424.051771186697,424.115008234622),
 .UNSPECIFIED.);
#374=B_SPLINE_CURVE_WITH_KNOTS('',3,(#41607,#41608,#41609,#41610,#41611,
#41612,#41613,#41614,#41615,#41616,#41617,#41618,#41619,#41620,#41621,#41622,
#41623,#41624,#41625,#41626,#41627,#41628,#41629,#41630,#41631,#41632,#41633,
#41634,#41635,#41636,#41637,#41638,#41639,#41640,#41641,#41642,#41643,#41644,
#41645,#41646,#41647,#41648,#41649,#41650,#41651,#41652,#41653,#41654,#41655,
#41656,#41657,#41658,#41659,#41660,#41661,#41662,#41663,#41664,#41665,#41666,
#41667,#41668,#41669,#41670,#41671,#41672,#41673,#41674,#41675,#41676,#41677,
#41678,#41679,#41680,#41681,#41682,#41683,#41684,#41685,#41686,#41687,#41688,
#41689,#41690,#41691,#41692,#41693,#41694,#41695,#41696,#41697,#41698,#41699,
#41700,#41701,#41702,#41703,#41704,#41705,#41706,#41707,#41708,#41709,#41710,
#41711,#41712,#41713,#41714,#41715,#41716,#41717,#41718,#41719,#41720,#41721,
#41722,#41723,#41724,#41725,#41726,#41727,#41728,#41729,#41730,#41731,#41732,
#41733,#41734,#41735,#41736,#41737,#41738,#41739,#41740,#41741,#41742,#41743,
#41744,#41745,#41746,#41747,#41748,#41749,#41750,#41751,#41752,#41753,#41754,
#41755,#41756,#41757,#41758,#41759,#41760,#41761,#41762,#41763,#41764,#41765,
#41766,#41767,#41768,#41769,#41770,#41771,#41772,#41773,#41774,#41775,#41776,
#41777,#41778),.UNSPECIFIED.,.F.,.F.,(4,3,3,3,3,3,3,3,3,3,3,3,3,3,3,3,3,
3,3,3,3,3,3,3,3,3,3,3,3,3,3,3,3,3,3,3,3,3,3,3,3,3,3,3,3,3,3,3,3,3,3,3,3,
3,3,3,3,4),(424.115885367393,424.191504095843,424.267055281936,424.342555776663,
424.419229827192,424.494691854454,424.570156747353,424.64563967224,424.723216799404,
424.798820852266,424.877384516583,424.955948180899,425.033542850333,425.111045116443,
425.188470601514,425.265834872891,425.343153453981,425.420449158453,425.497734203109,
425.575022595042,425.652328340568,425.729706380555,425.8071214523,425.884642066571,
425.95435618895,426.035842503383,426.117224585742,426.20130848755,426.282465806403,
426.363546590159,426.444536582192,426.453560192975,426.534573299266,426.615661993539,
426.699937544405,426.781247010794,426.862633912005,426.94414105077,426.952764197001,
427.03029235021,427.107739225172,427.185120403879,427.26245142134,427.339747776171,
427.417038076507,427.494327984246,427.571631506244,427.648962654371,427.726382144192,
427.803847502614,427.881432888912,427.951172205052,428.028047342388,428.104830802628,
428.181519055578,428.258152428406,428.334738399456,428.352171190823),
 .UNSPECIFIED.);
#375=B_SPLINE_CURVE_WITH_KNOTS('',3,(#41784,#41785,#41786,#41787,#41788,
#41789,#41790,#41791,#41792,#41793,#41794,#41795,#41796,#41797,#41798,#41799,
#41800,#41801,#41802,#41803,#41804,#41805,#41806,#41807,#41808,#41809,#41810,
#41811,#41812,#41813,#41814,#41815,#41816,#41817,#41818,#41819,#41820,#41821,
#41822,#41823,#41824,#41825,#41826,#41827,#41828,#41829,#41830,#41831,#41832,
#41833,#41834,#41835,#41836,#41837,#41838,#41839,#41840,#41841,#41842,#41843,
#41844,#41845,#41846,#41847,#41848,#41849,#41850,#41851,#41852,#41853,#41854,
#41855,#41856,#41857,#41858,#41859,#41860,#41861,#41862,#41863,#41864,#41865,
#41866,#41867,#41868,#41869,#41870,#41871,#41872,#41873,#41874,#41875,#41876,
#41877,#41878,#41879,#41880,#41881,#41882,#41883,#41884,#41885,#41886,#41887,
#41888,#41889,#41890,#41891,#41892,#41893,#41894,#41895,#41896,#41897,#41898,
#41899,#41900,#41901,#41902,#41903,#41904,#41905,#41906,#41907,#41908,#41909,
#41910,#41911,#41912,#41913,#41914,#41915,#41916,#41917,#41918,#41919,#41920,
#41921,#41922,#41923,#41924,#41925,#41926,#41927,#41928,#41929,#41930,#41931,
#41932,#41933,#41934,#41935,#41936,#41937,#41938,#41939,#41940,#41941,#41942,
#41943,#41944,#41945,#41946,#41947,#41948,#41949,#41950,#41951,#41952,#41953,
#41954,#41955),.UNSPECIFIED.,.F.,.F.,(4,3,3,3,3,3,3,3,3,3,3,3,3,3,3,3,3,
3,3,3,3,3,3,3,3,3,3,3,3,3,3,3,3,3,3,3,3,3,3,3,3,3,3,3,3,3,3,3,3,3,3,3,3,
3,3,3,3,4),(430.399063857647,430.47506981317,430.551009478196,430.626899514323,
430.702762601598,430.778613508728,430.854467241634,430.930338807012,431.006280296983,
431.082261107464,431.158338427554,431.19690686387,431.278390836825,431.359770200965,
431.444023568112,431.525177063284,431.606253741244,431.687239169034,431.696783669554,
431.777792065458,431.858876322289,431.943322360527,432.024628442234,432.106012232002,
432.18751689303,432.196660475239,432.274176253502,432.351610553913,432.42897897234,
432.50629705749,432.583580321534,432.660857405846,432.738133986334,432.815424081731,
432.892741715736,432.97014792206,433.047599931373,433.125172739696,433.196414086608,
433.273262709795,433.350017556192,433.426694895597,433.503310935372,433.579881833997,
433.656917566995,433.7334599857,433.810008322263,433.886577153711,433.963974789777,
434.04066587073,434.118416784354,434.196167697978,434.273691750868,434.351130704965,
434.428482608017,434.5057841065,434.583046149192,434.634961198303),
 .UNSPECIFIED.);
#376=B_SPLINE_CURVE_WITH_KNOTS('',3,(#41956,#41957,#41958,#41959,#41960,
#41961,#41962,#41963,#41964,#41965,#41966,#41967,#41968,#41969,#41970,#41971,
#41972,#41973,#41974,#41975,#41976,#41977,#41978,#41979,#41980,#41981,#41982,
#41983,#41984,#41985,#41986,#41987,#41988,#41989,#41990,#41991,#41992,#41993,
#41994,#41995,#41996,#41997,#41998,#41999,#42000,#42001,#42002,#42003,#42004,
#42005,#42006,#42007,#42008,#42009,#42010,#42011,#42012,#42013,#42014,#42015,
#42016,#42017,#42018,#42019,#42020,#42021,#42022,#42023,#42024,#42025,#42026,
#42027,#42028,#42029,#42030,#42031),.UNSPECIFIED.,.F.,.F.,(4,3,3,3,3,3,
3,3,3,3,3,3,3,3,3,3,3,3,3,3,3,3,3,3,3,4),(428.351671490987,428.434133094841,
428.516594032811,428.599054332297,428.681514020694,428.763973125396,428.846431673795,
428.928889693281,429.011347211243,429.098025106903,429.180491892739,429.262957006082,
429.345420556587,429.427882653885,429.510343407587,429.592802927284,429.675261322551,
429.757718702948,429.840185089215,429.922648291229,430.005108747509,430.08756689642,
430.170032501299,430.252492380514,430.334956493877,430.398193541802),
 .UNSPECIFIED.);
#377=B_SPLINE_CURVE_WITH_KNOTS('',3,(#42033,#42034,#42035,#42036,#42037,
#42038,#42039,#42040,#42041,#42042,#42043,#42044,#42045,#42046,#42047,#42048,
#42049,#42050,#42051,#42052,#42053,#42054,#42055,#42056,#42057,#42058,#42059,
#42060,#42061,#42062,#42063,#42064,#42065,#42066,#42067,#42068,#42069,#42070,
#42071,#42072,#42073,#42074,#42075,#42076,#42077,#42078,#42079,#42080,#42081,
#42082,#42083,#42084,#42085,#42086,#42087,#42088,#42089,#42090,#42091,#42092,
#42093,#42094,#42095,#42096,#42097,#42098,#42099,#42100,#42101,#42102,#42103,
#42104,#42105,#42106,#42107,#42108,#42109,#42110,#42111,#42112,#42113,#42114),
 .UNSPECIFIED.,.F.,.F.,(4,3,3,3,3,3,3,3,3,3,3,3,3,3,3,3,3,3,3,3,3,3,3,3,
3,3,3,4),(428.352171190823,428.428734883338,428.505293287412,428.581860967938,
428.658452493169,428.735126353376,428.811843832614,428.888674740058,428.949580213103,
429.027110409563,429.104553504168,429.181925138224,429.259240901792,429.336516344571,
429.41377722699,429.491032532635,429.568296302929,429.645582581413,429.722949394205,
429.800357728912,429.877879285475,429.947988221154,430.031143785834,430.114144129527,
430.196918607618,430.27955349429,430.361988636971,430.398193541718),
 .UNSPECIFIED.);
#378=B_SPLINE_CURVE_WITH_KNOTS('',3,(#42115,#42116,#42117,#42118,#42119,
#42120,#42121,#42122,#42123,#42124,#42125,#42126,#42127,#42128,#42129,#42130,
#42131,#42132,#42133,#42134,#42135,#42136,#42137,#42138,#42139,#42140,#42141,
#42142,#42143,#42144,#42145,#42146,#42147,#42148,#42149,#42150,#42151,#42152,
#42153,#42154,#42155,#42156,#42157,#42158,#42159,#42160,#42161,#42162,#42163,
#42164,#42165,#42166,#42167,#42168,#42169,#42170,#42171,#42172,#42173,#42174,
#42175,#42176,#42177,#42178,#42179,#42180,#42181,#42182,#42183,#42184,#42185,
#42186,#42187,#42188,#42189,#42190,#42191,#42192,#42193,#42194,#42195,#42196,
#42197,#42198,#42199,#42200,#42201,#42202,#42203,#42204,#42205,#42206,#42207,
#42208,#42209,#42210,#42211,#42212,#42213,#42214,#42215,#42216,#42217,#42218,
#42219,#42220,#42221,#42222,#42223,#42224,#42225,#42226,#42227,#42228,#42229,
#42230,#42231,#42232,#42233,#42234,#42235,#42236,#42237,#42238,#42239,#42240,
#42241,#42242,#42243,#42244,#42245,#42246,#42247,#42248,#42249,#42250,#42251,
#42252,#42253,#42254,#42255,#42256,#42257,#42258,#42259,#42260,#42261,#42262,
#42263,#42264,#42265,#42266,#42267,#42268,#42269,#42270,#42271,#42272,#42273,
#42274,#42275,#42276,#42277,#42278,#42279,#42280,#42281,#42282,#42283),
 .UNSPECIFIED.,.F.,.F.,(4,3,3,3,3,3,3,3,3,3,3,3,3,3,3,3,3,3,3,3,3,3,3,3,
3,3,3,3,3,3,3,3,3,3,3,3,3,3,3,3,3,3,3,3,3,3,3,3,3,3,3,3,3,3,3,3,4),(430.398193541802,
430.477934676748,430.557733637174,430.637599956251,430.717603913083,430.797679697289,
430.877905131397,430.946396229205,431.023232261328,431.099979277055,431.176653514618,
431.253271154139,431.329848330766,431.406717819077,431.4832779216,431.559848218747,
431.636443279769,431.713533519141,431.790260715722,431.867532476489,431.944804237256,
432.02239890669,432.0999011728,432.177326657871,432.254690929248,432.332009510339,
432.40930521481,432.486590259466,432.563878651399,432.641184396925,432.718562436912,
432.795977508657,432.873498122928,432.943212245306,433.024698559739,433.106080642097,
433.190164543906,433.271321862759,433.352402646513,433.433392638546,433.442416249332,
433.523429355622,433.604518049896,433.688793600761,433.770103067151,433.851489968362,
433.932997107127,433.941620253357,434.019164244903,434.096602312649,434.17397907238,
434.251308597381,434.328604931425,434.405895237983,434.483179196186,434.560499114131,
434.634363295085),.UNSPECIFIED.);
#379=B_SPLINE_CURVE_WITH_KNOTS('',3,(#42289,#42290,#42291,#42292,#42293,
#42294,#42295,#42296,#42297,#42298,#42299,#42300,#42301,#42302,#42303,#42304,
#42305,#42306,#42307,#42308,#42309,#42310,#42311,#42312,#42313,#42314,#42315,
#42316,#42317,#42318,#42319,#42320,#42321,#42322,#42323,#42324,#42325,#42326,
#42327,#42328,#42329,#42330,#42331,#42332,#42333,#42334,#42335,#42336,#42337,
#42338,#42339,#42340,#42341,#42342,#42343,#42344,#42345,#42346,#42347,#42348,
#42349,#42350,#42351,#42352,#42353,#42354,#42355,#42356,#42357,#42358,#42359,
#42360,#42361,#42362,#42363,#42364,#42365,#42366,#42367,#42368,#42369,#42370,
#42371,#42372,#42373,#42374,#42375,#42376,#42377,#42378,#42379,#42380,#42381,
#42382,#42383,#42384,#42385,#42386,#42387,#42388,#42389,#42390,#42391,#42392,
#42393,#42394,#42395,#42396,#42397,#42398,#42399,#42400,#42401,#42402,#42403,
#42404,#42405,#42406,#42407,#42408,#42409,#42410,#42411,#42412,#42413,#42414,
#42415,#42416,#42417,#42418,#42419,#42420,#42421,#42422,#42423,#42424,#42425,
#42426,#42427,#42428,#42429,#42430,#42431,#42432,#42433,#42434,#42435,#42436,
#42437,#42438,#42439,#42440,#42441,#42442,#42443,#42444,#42445),
 .UNSPECIFIED.,.F.,.F.,(4,3,3,3,3,3,3,3,3,3,3,3,3,3,3,3,3,3,3,3,3,3,3,3,
3,3,3,3,3,3,3,3,3,3,3,3,3,3,3,3,3,3,3,3,3,3,3,3,3,3,3,3,4),(436.681385966666,
436.763848172672,436.846310030382,436.928771546646,437.011232728315,437.093693582238,
437.176154115265,437.258614334245,437.341074246026,437.423533857458,437.50599317539,
437.588452206667,437.67091095814,437.753369436655,437.835827649061,437.918285602203,
438.000743302929,438.083200758086,438.16565797452,438.251669978609,438.334994107569,
438.417460712945,438.499926474119,438.582391418507,438.66485557352,438.747318966568,
438.829781625058,438.912243576395,438.99470484798,439.077165467212,439.159625461489,
439.242084858207,439.324543684757,439.407001968531,439.489459736917,439.571917017304,
439.656049835307,439.738515833271,439.820980209508,439.903443073659,439.985904535348,
440.068364704175,440.150823689725,440.233281601565,440.318876664537,440.401341400926,
440.483803172746,440.566262418435,440.648719576287,440.731182094189,440.81363976478,
440.896098554141,440.918042105346),.UNSPECIFIED.);
#380=B_SPLINE_CURVE_WITH_KNOTS('',3,(#42446,#42447,#42448,#42449,#42450,
#42451,#42452,#42453,#42454,#42455,#42456,#42457,#42458,#42459,#42460,#42461,
#42462,#42463,#42464,#42465,#42466,#42467,#42468,#42469,#42470,#42471,#42472,
#42473,#42474,#42475,#42476,#42477,#42478,#42479,#42480,#42481,#42482,#42483,
#42484,#42485,#42486,#42487,#42488,#42489,#42490,#42491,#42492,#42493,#42494,
#42495,#42496,#42497,#42498,#42499,#42500,#42501,#42502,#42503,#42504,#42505,
#42506,#42507,#42508,#42509,#42510,#42511,#42512,#42513,#42514,#42515,#42516,
#42517,#42518,#42519,#42520,#42521,#42522,#42523,#42524,#42525,#42526,#42527),
 .UNSPECIFIED.,.F.,.F.,(4,3,3,3,3,3,3,3,3,3,3,3,3,3,3,3,3,3,3,3,3,3,3,3,
3,3,3,4),(434.634961198303,434.71220303447,434.789448602289,434.866711955887,
434.944007156678,435.021386553096,435.098815887312,435.176345568828,435.195921309347,
435.273438678543,435.350868745995,435.428227167264,435.505529546479,435.582791447241,
435.660038657932,435.737280182151,435.814530073497,435.89180238764,435.969155458866,
436.046549988618,436.12405849358,436.195674920716,436.276868002695,436.357923541258,
436.438790770997,436.519548903297,436.600434123478,436.681319343659),
 .UNSPECIFIED.);
#381=B_SPLINE_CURVE_WITH_KNOTS('',3,(#42529,#42530,#42531,#42532,#42533,
#42534,#42535,#42536,#42537,#42538,#42539,#42540,#42541,#42542,#42543,#42544,
#42545,#42546,#42547,#42548,#42549,#42550,#42551,#42552,#42553,#42554,#42555,
#42556,#42557,#42558,#42559,#42560,#42561,#42562,#42563,#42564,#42565,#42566,
#42567,#42568,#42569,#42570,#42571,#42572,#42573,#42574,#42575,#42576,#42577,
#42578,#42579,#42580,#42581,#42582,#42583,#42584,#42585,#42586,#42587,#42588,
#42589,#42590,#42591,#42592,#42593,#42594,#42595,#42596,#42597,#42598,#42599,
#42600,#42601,#42602,#42603,#42604,#42605,#42606,#42607,#42608,#42609,#42610),
 .UNSPECIFIED.,.F.,.F.,(4,3,3,3,3,3,3,3,3,3,3,3,3,3,3,3,3,3,3,3,3,3,3,3,
3,3,3,4),(434.634363295085,434.711781031404,434.789244072866,434.866828149655,
434.940028261408,435.01689164606,435.09366147787,435.170354013859,435.246985449026,
435.32357192981,435.400429972266,435.476988295229,435.553552629902,435.630137543029,
435.707212224636,435.783919045505,435.861177657482,435.938436269459,436.015252140749,
436.091978335191,436.168616513899,436.245204529027,436.321757030141,436.398288642394,
436.474832648956,436.551381985816,436.627980740001,436.681378848981),
 .UNSPECIFIED.);
#382=B_SPLINE_CURVE_WITH_KNOTS('',3,(#42611,#42612,#42613,#42614,#42615,
#42616,#42617,#42618,#42619,#42620,#42621,#42622,#42623,#42624,#42625,#42626,
#42627,#42628,#42629,#42630,#42631,#42632,#42633,#42634,#42635,#42636,#42637,
#42638,#42639,#42640,#42641,#42642,#42643,#42644,#42645,#42646,#42647,#42648,
#42649,#42650,#42651,#42652,#42653,#42654,#42655,#42656,#42657,#42658,#42659,
#42660,#42661,#42662,#42663,#42664,#42665,#42666,#42667,#42668,#42669,#42670,
#42671,#42672,#42673,#42674,#42675,#42676,#42677,#42678,#42679,#42680,#42681,
#42682,#42683,#42684,#42685,#42686,#42687,#42688,#42689,#42690,#42691,#42692,
#42693,#42694,#42695,#42696,#42697,#42698,#42699,#42700,#42701,#42702,#42703,
#42704,#42705,#42706,#42707,#42708,#42709,#42710,#42711,#42712,#42713,#42714,
#42715,#42716,#42717,#42718,#42719,#42720,#42721,#42722,#42723,#42724,#42725,
#42726,#42727,#42728,#42729,#42730,#42731,#42732,#42733,#42734,#42735,#42736,
#42737,#42738,#42739,#42740,#42741,#42742,#42743,#42744,#42745,#42746,#42747,
#42748,#42749,#42750,#42751,#42752,#42753,#42754,#42755,#42756,#42757,#42758,
#42759,#42760,#42761,#42762,#42763,#42764,#42765,#42766,#42767,#42768,#42769,
#42770,#42771,#42772,#42773,#42774,#42775,#42776),.UNSPECIFIED.,.F.,.F.,
(4,3,3,3,3,3,3,3,3,3,3,3,3,3,3,3,3,3,3,3,3,3,3,3,3,3,3,3,3,3,3,3,3,3,3,
3,3,3,3,3,3,3,3,3,3,3,3,3,3,3,3,3,3,3,3,4),(436.681378849124,436.778854694112,
436.87810332322,436.93684427751,437.014374395573,437.091817424889,437.169189006715,
437.246504731075,437.323780147636,437.401041023662,437.478296335008,437.5555601231,
437.632846431484,437.71021329309,437.787621687022,437.865143319894,437.935252285561,
438.012088317684,438.088835333411,438.165509570974,438.242127210496,438.318704387123,
438.395573875434,438.472133977957,438.548704275104,438.625299336126,438.702389575498,
438.779116772079,438.856388532846,438.933660293612,439.011254963046,439.088757229156,
439.166182714227,439.243546985604,439.320865566695,439.398161271166,439.475446315822,
439.552734707755,439.630040453281,439.707418493268,439.784833565012,439.862354179284,
439.932068301663,440.013554616096,440.094936698455,440.179020600263,440.260177919116,
440.341258702871,440.422248694905,440.431272305688,440.512283283703,440.593369813142,
440.674600105717,440.755901737176,440.837349893263,440.918106228972),
 .UNSPECIFIED.);
#383=B_SPLINE_CURVE_WITH_KNOTS('',3,(#42782,#42783,#42784,#42785,#42786,
#42787,#42788,#42789,#42790,#42791,#42792,#42793,#42794,#42795,#42796,#42797,
#42798,#42799,#42800,#42801,#42802,#42803,#42804,#42805,#42806,#42807,#42808,
#42809,#42810,#42811,#42812,#42813,#42814,#42815,#42816,#42817,#42818,#42819,
#42820,#42821,#42822,#42823,#42824,#42825,#42826,#42827,#42828,#42829,#42830,
#42831,#42832,#42833,#42834,#42835,#42836,#42837,#42838,#42839,#42840,#42841,
#42842,#42843,#42844,#42845,#42846,#42847,#42848,#42849,#42850,#42851,#42852,
#42853,#42854,#42855,#42856,#42857,#42858,#42859,#42860,#42861,#42862,#42863,
#42864,#42865,#42866,#42867,#42868,#42869,#42870,#42871,#42872,#42873,#42874,
#42875,#42876,#42877,#42878,#42879,#42880,#42881,#42882,#42883,#42884,#42885,
#42886,#42887,#42888,#42889,#42890,#42891,#42892,#42893,#42894,#42895,#42896,
#42897,#42898,#42899,#42900,#42901,#42902,#42903,#42904,#42905,#42906,#42907,
#42908,#42909,#42910,#42911,#42912,#42913,#42914,#42915,#42916,#42917,#42918,
#42919,#42920,#42921,#42922,#42923,#42924,#42925,#42926,#42927,#42928,#42929,
#42930,#42931,#42932,#42933,#42934,#42935,#42936,#42937,#42938,#42939,#42940,
#42941,#42942,#42943,#42944,#42945,#42946,#42947,#42948,#42949,#42950,#42951,
#42952,#42953),.UNSPECIFIED.,.F.,.F.,(4,3,3,3,3,3,3,3,3,3,3,3,3,3,3,3,3,
3,3,3,3,3,3,3,3,3,3,3,3,3,3,3,3,3,3,3,3,3,3,3,3,3,3,3,3,3,3,3,3,3,3,3,3,
3,3,3,3,4),(442.964564156161,443.069008632475,443.176903439814,443.193950200302,
443.270771397457,443.347503359671,443.424162337819,443.500764524281,443.577326066162,
443.65437328435,443.730917458995,443.80747173904,443.88405070402,443.961463980933,
444.03817546124,444.115939636455,444.193703811671,444.271286435285,444.348776417494,
444.426189394719,444.50354094822,444.580846615131,444.658129208176,444.73540099512,
444.812675994976,444.889968225914,444.967332898279,445.044734506712,445.12224232132,
445.193457423041,445.274941395996,445.356320760136,445.440574127284,445.521727622455,
445.602804300415,445.683789728205,445.693334228725,445.774342624629,445.85542688146,
445.939872919697,446.021179001404,446.102562791172,446.184067452201,446.19321103441,
446.270726812673,446.348161113084,446.425529531511,446.502847616661,446.580130880706,
446.657407965018,446.734684545506,446.811974640903,446.889292274908,446.966698481232,
447.044150490546,447.121723298868,447.192964645779,447.201503895611),
 .UNSPECIFIED.);
#384=B_SPLINE_CURVE_WITH_KNOTS('',3,(#42954,#42955,#42956,#42957,#42958,
#42959,#42960,#42961,#42962,#42963,#42964,#42965,#42966,#42967,#42968,#42969,
#42970,#42971,#42972,#42973,#42974,#42975,#42976,#42977,#42978,#42979,#42980,
#42981,#42982,#42983,#42984,#42985,#42986,#42987,#42988,#42989,#42990,#42991,
#42992,#42993,#42994,#42995,#42996,#42997,#42998,#42999,#43000,#43001,#43002,
#43003,#43004,#43005,#43006,#43007,#43008,#43009,#43010,#43011,#43012,#43013,
#43014,#43015,#43016,#43017,#43018,#43019,#43020,#43021,#43022,#43023,#43024,
#43025,#43026,#43027,#43028,#43029),.UNSPECIFIED.,.F.,.F.,(4,3,3,3,3,3,
3,3,3,3,3,3,3,3,3,3,3,3,3,3,3,3,3,3,3,4),(440.918042105346,441.0005037092,
441.08296464717,441.165424946656,441.247884635053,441.330343739755,441.412802288154,
441.49526030764,441.577717825602,441.664395721262,441.746862507097,441.829327620441,
441.911791170946,441.994253268244,442.076714021946,442.159173541643,442.24163193691,
442.324089317308,442.406555703574,442.489018905588,442.571479361868,442.653937510779,
442.736403115658,442.818862994873,442.901327108237,442.964564156161),
 .UNSPECIFIED.);
#385=B_SPLINE_CURVE_WITH_KNOTS('',3,(#43031,#43032,#43033,#43034,#43035,
#43036,#43037,#43038,#43039,#43040,#43041,#43042,#43043,#43044,#43045,#43046,
#43047,#43048,#43049,#43050,#43051,#43052,#43053,#43054,#43055,#43056,#43057,
#43058,#43059,#43060,#43061,#43062,#43063,#43064,#43065,#43066,#43067,#43068,
#43069,#43070,#43071,#43072,#43073,#43074,#43075,#43076,#43077,#43078,#43079,
#43080,#43081,#43082,#43083,#43084,#43085,#43086,#43087,#43088,#43089,#43090,
#43091,#43092,#43093,#43094,#43095,#43096,#43097,#43098,#43099,#43100,#43101,
#43102,#43103,#43104,#43105,#43106,#43107,#43108,#43109,#43110,#43111,#43112,
#43113,#43114,#43115),.UNSPECIFIED.,.F.,.F.,(4,3,3,3,3,3,3,3,3,3,3,3,3,
3,3,3,3,3,3,3,3,3,3,3,3,3,3,3,4),(440.918106228972,440.930476309714,441.008004462923,
441.085451337885,441.162832516592,441.240163534053,441.317459888883,441.394750189219,
441.472040096958,441.549343618956,441.626674767083,441.704094256904,441.781559615326,
441.859145001624,441.928884317765,442.005747702417,442.082517534227,442.159210070215,
442.235841505382,442.312427986166,442.389286028622,442.465844351585,442.542408686258,
442.618993599385,442.696068280993,442.772775101861,442.850033713839,442.927292325816,
442.964564156161),.UNSPECIFIED.);
#386=B_SPLINE_CURVE_WITH_KNOTS('',3,(#43116,#43117,#43118,#43119,#43120,
#43121,#43122,#43123,#43124,#43125,#43126,#43127,#43128,#43129,#43130,#43131,
#43132,#43133,#43134,#43135,#43136,#43137,#43138,#43139,#43140,#43141,#43142,
#43143,#43144,#43145,#43146,#43147,#43148,#43149,#43150,#43151,#43152,#43153,
#43154,#43155,#43156,#43157,#43158,#43159,#43160,#43161,#43162,#43163,#43164,
#43165,#43166,#43167,#43168,#43169,#43170,#43171,#43172,#43173,#43174,#43175,
#43176,#43177,#43178,#43179,#43180,#43181,#43182,#43183,#43184,#43185,#43186,
#43187,#43188,#43189,#43190,#43191,#43192,#43193,#43194,#43195,#43196,#43197,
#43198,#43199,#43200,#43201,#43202,#43203,#43204,#43205,#43206,#43207,#43208,
#43209,#43210,#43211,#43212,#43213,#43214,#43215,#43216,#43217,#43218,#43219,
#43220,#43221,#43222,#43223,#43224,#43225,#43226,#43227,#43228,#43229,#43230,
#43231,#43232,#43233,#43234,#43235,#43236,#43237,#43238,#43239,#43240,#43241,
#43242,#43243,#43244,#43245,#43246,#43247,#43248,#43249,#43250,#43251,#43252,
#43253,#43254,#43255,#43256,#43257,#43258,#43259,#43260,#43261,#43262,#43263,
#43264,#43265,#43266,#43267,#43268,#43269,#43270,#43271,#43272,#43273,#43274,
#43275,#43276,#43277,#43278,#43279,#43280,#43281,#43282,#43283,#43284),
 .UNSPECIFIED.,.F.,.F.,(4,3,3,3,3,3,3,3,3,3,3,3,3,3,3,3,3,3,3,3,3,3,3,3,
3,3,3,3,3,3,3,3,3,3,3,3,3,3,3,3,3,3,3,3,3,3,3,3,3,3,3,3,3,3,3,3,4),(442.964564156239,
443.041606665765,443.118563047945,443.195449387586,443.272281715771,443.349076022084,
443.425858940481,443.50263918525,443.579431196097,443.656249417148,443.733148432809,
443.810093056011,443.887141978737,443.925700333867,444.00323045193,444.080673481246,
444.158045063072,444.235360787431,444.312636203992,444.389897080018,444.467152391364,
444.544416179456,444.62170248784,444.699069349446,444.776477743378,444.85399937625,
444.924108341917,445.00094437404,445.077691389767,445.15436562733,445.230983266851,
445.307560443478,445.384429931789,445.460990034312,445.537560331459,445.614155392481,
445.691245631853,445.767972828434,445.845244589201,445.922516349968,446.000111019402,
446.077613285513,446.155038770583,446.23240304196,446.309721623051,446.387017327523,
446.464302372179,446.541590764112,446.618896509638,446.696274549625,446.77368962137,
446.851210235641,446.920924358019,447.002401893102,447.083786687234,447.16505270286,
447.201722713917),.UNSPECIFIED.);
#387=B_SPLINE_CURVE_WITH_KNOTS('',3,(#43290,#43291,#43292,#43293,#43294,
#43295,#43296,#43297,#43298,#43299,#43300,#43301,#43302,#43303,#43304,#43305,
#43306,#43307,#43308,#43309,#43310,#43311,#43312,#43313,#43314,#43315,#43316,
#43317,#43318,#43319,#43320,#43321,#43322,#43323,#43324,#43325,#43326,#43327,
#43328,#43329,#43330,#43331,#43332,#43333,#43334,#43335,#43336,#43337,#43338,
#43339,#43340,#43341,#43342,#43343,#43344,#43345,#43346,#43347,#43348,#43349,
#43350,#43351,#43352,#43353,#43354,#43355,#43356,#43357,#43358,#43359,#43360,
#43361,#43362,#43363,#43364,#43365,#43366,#43367,#43368,#43369,#43370,#43371,
#43372,#43373,#43374,#43375,#43376,#43377,#43378,#43379,#43380,#43381,#43382,
#43383,#43384,#43385,#43386,#43387,#43388,#43389,#43390,#43391,#43392,#43393,
#43394,#43395,#43396,#43397,#43398,#43399,#43400,#43401,#43402,#43403,#43404,
#43405,#43406,#43407,#43408,#43409,#43410,#43411,#43412,#43413,#43414,#43415,
#43416,#43417,#43418,#43419,#43420,#43421,#43422,#43423,#43424,#43425,#43426,
#43427,#43428,#43429,#43430,#43431,#43432,#43433,#43434,#43435,#43436,#43437,
#43438,#43439,#43440,#43441,#43442,#43443,#43444,#43445,#43446,#43447,#43448,
#43449,#43450,#43451,#43452,#43453,#43454,#43455,#43456,#43457,#43458,#43459,
#43460,#43461),.UNSPECIFIED.,.F.,.F.,(4,3,3,3,3,3,3,3,3,3,3,3,3,3,3,3,3,
3,3,3,3,3,3,3,3,3,3,3,3,3,3,3,3,3,3,3,3,3,3,3,3,3,3,3,3,3,3,3,3,3,3,3,3,
3,3,3,3,4),(449.247749463436,449.324633812506,449.401433890599,449.478165896341,
449.554845974575,449.634518412739,449.711153848794,449.787789394436,449.864439596091,
449.941119006604,450.017880231656,450.09468995308,450.171599527214,450.192225479887,
450.269046677042,450.345778639256,450.422437617404,450.499039803865,450.575601345746,
450.652648563934,450.729192738579,450.805747018624,450.882325983604,450.959739260517,
451.036450740824,451.11421491604,451.191979091257,451.269561714871,451.34705169708,
451.424464674305,451.501816227806,451.579121894718,451.656404487763,451.733676274706,
451.810951274563,451.888243505501,451.965608177866,452.043009786299,452.120517600907,
452.191732702626,452.273216675581,452.354596039721,452.438849406868,452.52000290204,
452.601079579999,452.682065007789,452.691609508311,452.772617904215,452.853702161046,
452.938148199284,453.019454280991,453.100838070759,453.182342731788,453.191486313996,
453.268994750771,453.346431169528,453.423794734071,453.484880270082),
 .UNSPECIFIED.);
#388=B_SPLINE_CURVE_WITH_KNOTS('',3,(#43462,#43463,#43464,#43465,#43466,
#43467,#43468,#43469,#43470,#43471,#43472,#43473,#43474,#43475,#43476,#43477,
#43478,#43479,#43480,#43481,#43482,#43483,#43484,#43485,#43486,#43487,#43488,
#43489,#43490,#43491,#43492,#43493,#43494,#43495,#43496,#43497,#43498,#43499,
#43500,#43501,#43502,#43503,#43504,#43505,#43506,#43507,#43508,#43509,#43510,
#43511,#43512,#43513,#43514,#43515,#43516,#43517,#43518,#43519,#43520,#43521,
#43522,#43523,#43524,#43525,#43526,#43527,#43528,#43529,#43530,#43531,#43532,
#43533,#43534,#43535,#43536,#43537,#43538,#43539,#43540,#43541,#43542,#43543),
 .UNSPECIFIED.,.F.,.F.,(4,3,3,3,3,3,3,3,3,3,3,3,3,3,3,3,3,3,3,3,3,3,3,3,
3,3,3,4),(447.201503895611,447.278341299462,447.355086736831,447.431756469874,
447.508366699878,447.584933580683,447.661483067255,447.738025422464,447.814575221681,
447.891147042584,447.967800680472,448.044496309227,448.121308597704,448.192718257149,
448.270235808767,448.347666028187,448.425024571082,448.502327041669,448.579589003619,
448.656836229402,448.734077740609,448.811327590842,448.888599835755,448.965952793727,
449.043347186035,449.120855513704,449.192471868518,449.247749463341),
 .UNSPECIFIED.);
#389=B_SPLINE_CURVE_WITH_KNOTS('',3,(#43545,#43546,#43547,#43548,#43549,
#43550,#43551,#43552,#43553,#43554,#43555,#43556,#43557,#43558,#43559,#43560,
#43561,#43562,#43563,#43564,#43565,#43566,#43567,#43568,#43569,#43570,#43571,
#43572,#43573,#43574,#43575,#43576,#43577,#43578,#43579,#43580,#43581,#43582,
#43583,#43584,#43585,#43586,#43587,#43588,#43589,#43590,#43591,#43592,#43593,
#43594,#43595,#43596,#43597,#43598,#43599,#43600,#43601,#43602,#43603,#43604,
#43605,#43606,#43607,#43608,#43609,#43610,#43611,#43612,#43613,#43614,#43615,
#43616,#43617,#43618,#43619,#43620,#43621,#43622,#43623,#43624,#43625,#43626),
 .UNSPECIFIED.,.F.,.F.,(4,3,3,3,3,3,3,3,3,3,3,3,3,3,3,3,3,3,3,3,3,3,3,3,
3,3,3,4),(447.201722713917,447.282847402085,447.363869242774,447.420128362045,
447.501141468335,447.582230162609,447.666505713474,447.747815179864,447.829202081075,
447.91070921984,447.91933236607,447.996860519279,448.07430739424,448.151688572948,
448.229019590409,448.306315945239,448.383606245575,448.460896153313,448.538199675311,
448.615530823439,448.69295031326,448.770415671682,448.84800105798,448.917740374121,
449.008245292473,449.098328326512,449.187621314979,449.24774946334),
 .UNSPECIFIED.);
#390=B_SPLINE_CURVE_WITH_KNOTS('',3,(#43627,#43628,#43629,#43630,#43631,
#43632,#43633,#43634,#43635,#43636,#43637,#43638,#43639,#43640,#43641,#43642,
#43643,#43644,#43645,#43646,#43647,#43648,#43649,#43650,#43651,#43652,#43653,
#43654,#43655,#43656,#43657,#43658,#43659,#43660,#43661,#43662,#43663,#43664,
#43665,#43666,#43667,#43668,#43669,#43670,#43671,#43672,#43673,#43674,#43675,
#43676,#43677,#43678,#43679,#43680,#43681,#43682,#43683,#43684,#43685,#43686,
#43687,#43688,#43689,#43690,#43691,#43692,#43693,#43694,#43695,#43696,#43697,
#43698,#43699,#43700,#43701,#43702,#43703,#43704,#43705,#43706,#43707,#43708,
#43709,#43710,#43711,#43712,#43713,#43714,#43715,#43716,#43717,#43718,#43719,
#43720,#43721,#43722,#43723,#43724,#43725,#43726,#43727,#43728,#43729,#43730,
#43731,#43732,#43733,#43734,#43735,#43736,#43737,#43738,#43739,#43740,#43741,
#43742,#43743,#43744,#43745,#43746,#43747,#43748,#43749,#43750,#43751,#43752,
#43753,#43754,#43755,#43756,#43757,#43758,#43759,#43760,#43761,#43762,#43763,
#43764,#43765,#43766,#43767,#43768,#43769,#43770,#43771,#43772,#43773,#43774,
#43775,#43776,#43777,#43778,#43779,#43780,#43781,#43782,#43783),
 .UNSPECIFIED.,.F.,.F.,(4,3,3,3,3,3,3,3,3,3,3,3,3,3,3,3,3,3,3,3,3,3,3,3,
3,3,3,3,3,3,3,3,3,3,3,3,3,3,3,3,3,3,3,3,3,3,3,3,3,3,3,3,4),(449.24774946334,
449.330211669376,449.412673527116,449.49513504341,449.577596225107,449.660057079059,
449.742517612113,449.824977831119,449.907437742927,449.989897354385,450.072356672341,
450.154815703643,450.23727445514,450.319732933678,450.402191146106,450.484649099271,
450.567106800018,450.649564255196,450.732021471651,450.818033698152,450.901358042576,
450.983824648021,451.066290409263,451.148755353715,451.231219508791,451.3136829019,
451.396145560449,451.478607511841,451.56106878348,451.643529402764,451.725989397091,
451.808448793856,451.890907620451,451.973365904268,452.055823672695,452.13828095312,
452.222414188532,452.304880186624,452.387344562979,452.469807427241,452.552268889032,
452.634729057953,452.717188043589,452.799645955506,452.885241801031,452.967706537631,
453.050168309633,453.132627555475,453.215084713452,453.297547231733,453.380004902588,
453.462463692539,453.484412719705),.UNSPECIFIED.);
#391=B_SPLINE_CURVE_WITH_KNOTS('',3,(#43789,#43790,#43791,#43792,#43793,
#43794,#43795,#43796,#43797,#43798,#43799,#43800,#43801,#43802,#43803,#43804,
#43805,#43806,#43807,#43808,#43809,#43810,#43811,#43812,#43813,#43814,#43815,
#43816,#43817,#43818,#43819,#43820,#43821,#43822,#43823,#43824,#43825,#43826,
#43827,#43828,#43829,#43830,#43831,#43832,#43833,#43834,#43835,#43836,#43837,
#43838,#43839,#43840,#43841,#43842,#43843,#43844,#43845,#43846,#43847,#43848,
#43849,#43850,#43851,#43852,#43853,#43854,#43855,#43856,#43857,#43858,#43859,
#43860,#43861,#43862,#43863,#43864,#43865,#43866,#43867,#43868,#43869,#43870,
#43871,#43872,#43873,#43874,#43875,#43876,#43877,#43878,#43879,#43880,#43881,
#43882,#43883,#43884,#43885,#43886,#43887,#43888,#43889,#43890,#43891,#43892,
#43893,#43894,#43895,#43896,#43897,#43898,#43899,#43900,#43901,#43902,#43903,
#43904,#43905,#43906,#43907,#43908,#43909,#43910,#43911,#43912,#43913,#43914,
#43915,#43916,#43917,#43918,#43919,#43920,#43921,#43922,#43923,#43924,#43925,
#43926,#43927,#43928,#43929,#43930,#43931,#43932,#43933,#43934,#43935,#43936,
#43937,#43938,#43939,#43940,#43941,#43942,#43943,#43944,#43945),
 .UNSPECIFIED.,.F.,.F.,(4,3,3,3,3,3,3,3,3,3,3,3,3,3,3,3,3,3,3,3,3,3,3,3,
3,3,3,3,3,3,3,3,3,3,3,3,3,3,3,3,3,3,3,3,3,3,3,3,3,3,3,3,4),(455.53093477052,
455.613396976556,455.695858834296,455.77832035059,455.860781532287,455.943242386238,
456.025702919293,456.108163138299,456.190623050107,456.273082661565,456.355541979521,
456.438001010823,456.52045976232,456.602918240858,456.685376453286,456.767834406451,
456.850292107198,456.932749562376,457.015206778831,457.101219005332,457.184543349756,
457.267009955201,457.349475716443,457.431940660895,457.514404815971,457.59686820908,
457.679330867629,457.761792819021,457.84425409066,457.926714709944,458.009174704271,
458.091634101036,458.174092927631,458.256551211448,458.339008979875,458.4214662603,
458.505599495712,458.588065493804,458.670529870159,458.752992734421,458.835454196212,
458.917914365133,459.000373350769,459.082831262686,459.168427108211,459.250891844811,
459.333353616813,459.415812862655,459.498270020632,459.580732538913,459.663190209768,
459.745648999719,459.767598026885),.UNSPECIFIED.);
#392=B_SPLINE_CURVE_WITH_KNOTS('',3,(#43946,#43947,#43948,#43949,#43950,
#43951,#43952,#43953,#43954,#43955,#43956,#43957,#43958,#43959,#43960,#43961,
#43962,#43963,#43964,#43965,#43966,#43967,#43968,#43969,#43970,#43971,#43972,
#43973,#43974,#43975,#43976,#43977,#43978,#43979,#43980,#43981,#43982,#43983,
#43984,#43985,#43986,#43987,#43988,#43989,#43990,#43991,#43992,#43993,#43994,
#43995,#43996,#43997,#43998,#43999,#44000,#44001,#44002,#44003,#44004,#44005,
#44006,#44007,#44008,#44009,#44010,#44011,#44012,#44013,#44014,#44015,#44016,
#44017,#44018,#44019,#44020,#44021,#44022,#44023,#44024),.UNSPECIFIED.,
 .F.,.F.,(4,3,3,3,3,3,3,3,3,3,3,3,3,3,3,3,3,3,3,3,3,3,3,3,3,3,4),(453.484880270082,
453.5621695649,453.640803359958,453.718078947669,453.795365350718,453.872676591241,
453.952317424772,454.029761082876,454.110500504121,454.191239925365,454.268088548552,
454.344843394949,454.421520734353,454.498136774128,454.574707672753,454.65174340575,
454.728285824456,454.804834161018,454.881402992466,454.958800628533,455.035491709486,
455.11324262311,455.190993536734,455.282364191347,455.373352208432,455.463557419382,
455.53093477052),.UNSPECIFIED.);
#393=B_SPLINE_CURVE_WITH_KNOTS('',3,(#44026,#44027,#44028,#44029,#44030,
#44031,#44032,#44033,#44034,#44035,#44036,#44037,#44038,#44039,#44040,#44041,
#44042,#44043,#44044,#44045,#44046,#44047,#44048,#44049,#44050,#44051,#44052,
#44053,#44054,#44055,#44056,#44057,#44058,#44059,#44060,#44061,#44062,#44063,
#44064,#44065,#44066,#44067,#44068,#44069,#44070,#44071,#44072,#44073,#44074,
#44075,#44076,#44077,#44078,#44079,#44080,#44081,#44082,#44083,#44084,#44085,
#44086,#44087,#44088,#44089,#44090,#44091,#44092,#44093,#44094,#44095,#44096,
#44097,#44098,#44099,#44100,#44101),.UNSPECIFIED.,.F.,.F.,(4,3,3,3,3,3,
3,3,3,3,3,3,3,3,3,3,3,3,3,3,3,3,3,3,3,4),(453.484412719705,453.566874323559,
453.649335261529,453.731795561015,453.814255249412,453.896714354114,453.979172902513,
454.061630921999,454.144088439961,454.230766335621,454.313233121457,454.3956982348,
454.478161785305,454.560623882603,454.643084636305,454.725544156002,454.808002551269,
454.890459931666,454.972926317933,455.055389519947,455.137849976227,455.220308125138,
455.302773730017,455.385233609232,455.467697722596,455.53093477052),
 .UNSPECIFIED.);
#394=B_SPLINE_CURVE_WITH_KNOTS('',3,(#44102,#44103,#44104,#44105,#44106,
#44107,#44108,#44109,#44110,#44111,#44112,#44113,#44114,#44115,#44116,#44117,
#44118,#44119,#44120,#44121,#44122,#44123,#44124,#44125,#44126,#44127,#44128,
#44129,#44130,#44131,#44132,#44133,#44134,#44135,#44136,#44137,#44138,#44139,
#44140,#44141,#44142,#44143,#44144,#44145,#44146,#44147,#44148,#44149,#44150,
#44151,#44152,#44153,#44154,#44155,#44156,#44157,#44158,#44159,#44160,#44161,
#44162,#44163,#44164,#44165,#44166,#44167,#44168,#44169,#44170,#44171,#44172,
#44173,#44174,#44175,#44176,#44177,#44178,#44179,#44180,#44181,#44182,#44183,
#44184,#44185,#44186,#44187,#44188,#44189,#44190,#44191,#44192,#44193,#44194,
#44195,#44196,#44197,#44198,#44199,#44200,#44201,#44202,#44203,#44204,#44205,
#44206,#44207,#44208,#44209,#44210,#44211,#44212,#44213,#44214,#44215,#44216,
#44217,#44218,#44219,#44220,#44221,#44222,#44223,#44224,#44225,#44226,#44227,
#44228,#44229,#44230,#44231,#44232,#44233,#44234,#44235,#44236,#44237,#44238,
#44239,#44240,#44241,#44242,#44243,#44244,#44245,#44246,#44247,#44248,#44249,
#44250,#44251,#44252,#44253,#44254,#44255,#44256,#44257,#44258,#44259,#44260,
#44261,#44262,#44263,#44264,#44265,#44266,#44267,#44268,#44269,#44270),
 .UNSPECIFIED.,.F.,.F.,(4,3,3,3,3,3,3,3,3,3,3,3,3,3,3,3,3,3,3,3,3,3,3,3,
3,3,3,3,3,3,3,3,3,3,3,3,3,3,3,3,3,3,3,3,3,3,3,3,3,3,3,3,3,3,3,3,4),(455.53093477052,
455.619328038375,455.708463066107,455.797969399037,455.887897298536,455.906596430478,
455.98345981513,456.06022964694,456.136922182928,456.213553618095,456.290140098879,
456.366998141335,456.443556464298,456.520120798971,456.596705712098,456.673780393705,
456.750487214574,456.827745826551,456.905004438528,456.982534634988,457.059977729593,
457.137349363649,457.214665127217,457.291940569996,457.369201452415,457.44645675806,
457.523720528354,457.601006806838,457.67837361963,457.755781954337,457.8333035109,
457.903412446579,457.980942564642,458.058385593958,458.135757175784,458.213072900144,
458.290348316705,458.367609192731,458.444864504077,458.522128292169,458.599414600553,
458.676781462159,458.754189856091,458.831711488963,458.90182045463,458.978663768531,
459.055416516633,459.132094944059,459.211432932134,459.288010571749,459.364567540298,
459.441118406981,459.517677734815,459.594288165648,459.670929289699,459.747644296304,
459.766798848659),.UNSPECIFIED.);
#395=B_SPLINE_CURVE_WITH_KNOTS('',3,(#44276,#44277,#44278,#44279,#44280,
#44281,#44282,#44283,#44284,#44285,#44286,#44287,#44288,#44289,#44290,#44291,
#44292,#44293,#44294,#44295,#44296,#44297,#44298,#44299,#44300,#44301,#44302,
#44303,#44304,#44305,#44306,#44307,#44308,#44309,#44310,#44311,#44312,#44313,
#44314,#44315,#44316,#44317,#44318,#44319,#44320,#44321,#44322,#44323,#44324,
#44325,#44326,#44327,#44328,#44329,#44330,#44331,#44332,#44333,#44334,#44335,
#44336,#44337,#44338,#44339,#44340,#44341,#44342,#44343,#44344,#44345,#44346,
#44347,#44348,#44349,#44350,#44351,#44352,#44353,#44354,#44355,#44356,#44357,
#44358,#44359,#44360,#44361,#44362,#44363,#44364,#44365,#44366,#44367,#44368,
#44369,#44370,#44371,#44372,#44373,#44374,#44375,#44376,#44377,#44378,#44379,
#44380,#44381,#44382,#44383,#44384,#44385,#44386,#44387,#44388,#44389,#44390,
#44391,#44392,#44393,#44394,#44395,#44396,#44397,#44398,#44399,#44400,#44401,
#44402,#44403,#44404,#44405,#44406,#44407,#44408,#44409,#44410,#44411,#44412,
#44413,#44414,#44415,#44416,#44417,#44418,#44419,#44420,#44421,#44422,#44423,
#44424,#44425,#44426,#44427,#44428,#44429,#44430,#44431,#44432,#44433,#44434,
#44435,#44436,#44437,#44438,#44439,#44440,#44441),.UNSPECIFIED.,.F.,.F.,
(4,3,3,3,3,3,3,3,3,3,3,3,3,3,3,3,3,3,3,3,3,3,3,3,3,3,3,3,3,3,3,3,3,3,3,
3,3,3,3,3,3,3,3,3,3,3,3,3,3,3,3,3,3,3,3,4),(461.8141200777,461.899839896198,
461.986073399186,462.072573444055,462.159420638358,462.18926881632,462.266786367938,
462.344216587357,462.421575130251,462.498877600838,462.576139562788,462.65338678857,
462.730628299776,462.807878150009,462.885150394921,462.962503352891,463.0398977452,
463.117406072867,463.189022427689,463.266539796888,463.343969864341,463.421328285613,
463.498630664831,463.575892565596,463.653139776289,463.73038130051,463.807631191859,
463.884903506005,463.962256577233,464.039651106987,464.117159611951,464.188776039059,
464.265597236211,464.342329198423,464.418988176569,464.495590363028,464.572151904906,
464.649199123096,464.725743297738,464.802297577781,464.878876542759,464.956289819676,
465.033001299981,465.110765475204,465.188529650428,465.266120294956,465.343616772867,
465.421034726906,465.499685965902,465.576989793296,465.654266870418,465.731531224882,
465.81120957838,465.888513538795,465.969379088835,466.050244638876),
 .UNSPECIFIED.);
#396=B_SPLINE_CURVE_WITH_KNOTS('',3,(#44442,#44443,#44444,#44445,#44446,
#44447,#44448,#44449,#44450,#44451,#44452,#44453,#44454,#44455,#44456,#44457,
#44458,#44459,#44460,#44461,#44462,#44463,#44464,#44465,#44466,#44467,#44468,
#44469,#44470,#44471,#44472,#44473,#44474,#44475,#44476,#44477,#44478,#44479,
#44480,#44481,#44482,#44483,#44484,#44485,#44486,#44487,#44488,#44489,#44490,
#44491,#44492,#44493,#44494,#44495,#44496,#44497,#44498,#44499,#44500,#44501,
#44502,#44503,#44504,#44505,#44506,#44507,#44508,#44509,#44510,#44511,#44512,
#44513,#44514,#44515,#44516,#44517),.UNSPECIFIED.,.F.,.F.,(4,3,3,3,3,3,
3,3,3,3,3,3,3,3,3,3,3,3,3,3,3,3,3,3,3,4),(459.767598026885,459.850059630739,
459.932520568709,460.014980868195,460.097440556592,460.179899661294,460.262358209693,
460.34481622918,460.427273747141,460.513951642801,460.596418428637,460.67888354198,
460.761347092486,460.843809189783,460.926269943485,461.008729463182,461.09118785845,
461.173645238847,461.256111625113,461.338574827127,461.421035283408,461.503493432319,
461.585959037198,461.668418916412,461.750883029776,461.8141200777),
 .UNSPECIFIED.);
#397=B_SPLINE_CURVE_WITH_KNOTS('',3,(#44519,#44520,#44521,#44522,#44523,
#44524,#44525,#44526,#44527,#44528,#44529,#44530,#44531,#44532,#44533,#44534,
#44535,#44536,#44537,#44538,#44539,#44540,#44541,#44542,#44543,#44544,#44545,
#44546,#44547,#44548,#44549,#44550,#44551,#44552,#44553,#44554,#44555,#44556,
#44557,#44558,#44559,#44560,#44561,#44562,#44563,#44564,#44565,#44566,#44567,
#44568,#44569,#44570,#44571,#44572,#44573,#44574,#44575,#44576,#44577,#44578,
#44579,#44580,#44581,#44582,#44583,#44584,#44585,#44586,#44587,#44588,#44589,
#44590,#44591,#44592,#44593,#44594,#44595,#44596,#44597,#44598,#44599,#44600,
#44601,#44602,#44603),.UNSPECIFIED.,.F.,.F.,(4,3,3,3,3,3,3,3,3,3,3,3,3,
3,3,3,3,3,3,3,3,3,3,3,3,3,3,3,4),(459.766798848659,459.843658493391,459.900228462681,
459.977823132115,460.055325398226,460.132750883296,460.210115154673,460.287433735764,
460.364729440236,460.442014484892,460.519302876825,460.596608622351,460.673986662338,
460.751401734083,460.828922348354,460.898636470732,460.980122785165,461.061504867524,
461.145588769333,461.226746088186,461.307826871941,461.388816863975,461.397840474758,
461.475955296957,461.554107861435,461.632351562766,461.710648170262,461.789049728251,
461.814120077565),.UNSPECIFIED.);
#398=B_SPLINE_CURVE_WITH_KNOTS('',3,(#44604,#44605,#44606,#44607,#44608,
#44609,#44610,#44611,#44612,#44613,#44614,#44615,#44616,#44617,#44618,#44619,
#44620,#44621,#44622,#44623,#44624,#44625,#44626,#44627,#44628,#44629,#44630,
#44631,#44632,#44633,#44634,#44635,#44636,#44637,#44638,#44639,#44640,#44641,
#44642,#44643,#44644,#44645,#44646,#44647,#44648,#44649,#44650,#44651,#44652,
#44653,#44654,#44655,#44656,#44657,#44658,#44659,#44660,#44661,#44662,#44663,
#44664,#44665,#44666,#44667,#44668,#44669,#44670,#44671,#44672,#44673,#44674,
#44675,#44676,#44677,#44678,#44679,#44680,#44681,#44682,#44683,#44684,#44685,
#44686,#44687,#44688,#44689,#44690,#44691,#44692,#44693,#44694,#44695,#44696,
#44697,#44698,#44699,#44700,#44701,#44702,#44703,#44704,#44705,#44706,#44707,
#44708,#44709,#44710,#44711,#44712,#44713,#44714,#44715,#44716,#44717,#44718,
#44719,#44720,#44721,#44722,#44723,#44724,#44725,#44726,#44727,#44728,#44729,
#44730,#44731,#44732,#44733,#44734,#44735,#44736,#44737,#44738,#44739,#44740,
#44741,#44742,#44743,#44744,#44745,#44746,#44747,#44748,#44749,#44750,#44751,
#44752,#44753,#44754,#44755,#44756,#44757,#44758,#44759,#44760,#44761,#44762,
#44763,#44764,#44765,#44766,#44767,#44768,#44769),.UNSPECIFIED.,.F.,.F.,
(4,3,3,3,3,3,3,3,3,3,3,3,3,3,3,3,3,3,3,3,3,3,3,3,3,3,3,3,3,3,3,3,3,3,3,
3,3,3,3,3,3,3,3,3,3,3,3,3,3,3,3,3,3,3,3,4),(461.814120077699,461.897044478783,
461.974572631993,462.052019506954,462.129400685662,462.206731703123,462.284028057954,
462.361318358291,462.438608266029,462.515911788028,462.593242936156,462.670662425977,
462.748127784399,462.825713170698,462.895452486834,462.972315871486,463.049085703295,
463.125778239283,463.20240967445,463.278996155233,463.35585419769,463.432412520653,
463.508976855325,463.585561768452,463.66263645006,463.739343270929,463.816601882907,
463.893860494885,463.971390691344,464.048833785949,464.126205420004,464.203521183572,
464.28079662635,464.358057508769,464.435312814412,464.512576584706,464.58986286319,
464.667229675981,464.744638010688,464.82215956725,464.892268502936,464.969798621002,
465.04724165032,465.124613232148,465.20192895651,465.279204373074,465.356465249102,
465.43372056045,465.510984348545,465.588270656931,465.665637518539,465.743045912474,
465.820567545348,465.890676510987,465.97105445669,466.051432402393),
 .UNSPECIFIED.);
#399=B_SPLINE_CURVE_WITH_KNOTS('',3,(#44775,#44776,#44777,#44778,#44779,
#44780,#44781,#44782,#44783,#44784,#44785,#44786,#44787,#44788,#44789,#44790,
#44791,#44792,#44793,#44794,#44795,#44796,#44797,#44798,#44799,#44800,#44801,
#44802,#44803,#44804,#44805,#44806,#44807,#44808,#44809,#44810,#44811,#44812,
#44813,#44814,#44815,#44816,#44817,#44818,#44819,#44820,#44821,#44822,#44823,
#44824,#44825,#44826,#44827,#44828,#44829,#44830,#44831,#44832,#44833,#44834,
#44835,#44836,#44837,#44838,#44839,#44840,#44841,#44842,#44843,#44844,#44845,
#44846,#44847,#44848,#44849,#44850,#44851,#44852,#44853,#44854,#44855,#44856,
#44857,#44858,#44859,#44860,#44861,#44862,#44863,#44864,#44865,#44866,#44867,
#44868,#44869,#44870,#44871,#44872,#44873,#44874,#44875,#44876,#44877,#44878,
#44879,#44880,#44881,#44882,#44883,#44884,#44885,#44886,#44887,#44888,#44889,
#44890,#44891,#44892,#44893,#44894,#44895,#44896,#44897,#44898,#44899,#44900,
#44901,#44902,#44903,#44904,#44905,#44906,#44907,#44908,#44909,#44910,#44911,
#44912,#44913,#44914,#44915,#44916,#44917,#44918,#44919,#44920,#44921,#44922,
#44923,#44924,#44925,#44926,#44927,#44928,#44929,#44930,#44931),
 .UNSPECIFIED.,.F.,.F.,(4,3,3,3,3,3,3,3,3,3,3,3,3,3,3,3,3,3,3,3,3,3,3,3,
3,3,3,3,3,3,3,3,3,3,3,3,3,3,3,3,3,3,3,3,3,3,3,3,3,3,3,3,4),(468.097305384879,
468.179767590915,468.262229448655,468.344690964949,468.427152146646,468.509613000597,
468.592073533652,468.674533752658,468.756993664466,468.839453275924,468.92191259388,
469.004371625182,469.086830376679,469.169288855217,469.251747067645,469.33420502081,
469.416662721557,469.499120176735,469.58157739319,469.667589619691,469.750913964115,
469.83338056956,469.915846330802,469.998311275254,470.08077543033,470.163238823439,
470.245701481988,470.328163433381,470.410624705019,470.493085324303,470.57554531863,
470.658004715395,470.74046354199,470.822921825806,470.905379594234,470.987836874659,
471.071970110071,471.154436108162,471.236900484518,471.31936334878,471.401824810571,
471.484284979492,471.566743965127,471.649201877045,471.73479772257,471.81726245917,
471.899724231172,471.982183477014,472.064640634991,472.147103153272,472.229560824127,
472.312019614078,472.333968641244),.UNSPECIFIED.);
#400=B_SPLINE_CURVE_WITH_KNOTS('',3,(#44932,#44933,#44934,#44935,#44936,
#44937,#44938,#44939,#44940,#44941,#44942,#44943,#44944,#44945,#44946,#44947,
#44948,#44949,#44950,#44951,#44952,#44953,#44954,#44955,#44956,#44957,#44958,
#44959,#44960,#44961,#44962,#44963,#44964,#44965,#44966,#44967,#44968,#44969,
#44970,#44971,#44972,#44973,#44974,#44975,#44976,#44977,#44978,#44979,#44980,
#44981,#44982,#44983,#44984,#44985,#44986,#44987,#44988,#44989,#44990,#44991,
#44992,#44993,#44994,#44995,#44996,#44997,#44998,#44999,#45000,#45001,#45002,
#45003,#45004,#45005,#45006,#45007,#45008,#45009,#45010,#45011,#45012,#45013,
#45014,#45015,#45016),.UNSPECIFIED.,.F.,.F.,(4,3,3,3,3,3,3,3,3,3,3,3,3,
3,3,3,3,3,3,3,3,3,3,3,3,3,3,3,4),(466.050244638876,466.127755854532,466.188283261797,
466.269767234823,466.351146599033,466.435399966145,466.516553461384,466.59763013941,
466.678615567264,466.688160067482,466.769168463268,466.850252719979,466.934698758276,
467.016004839858,467.0973886295,467.178893290403,467.188036873167,467.264497215168,
467.340875943928,467.417189540611,467.493454429304,467.569694421594,467.645922807574,
467.722154389377,467.798403969437,467.874729422595,467.951093785583,468.027569488965,
468.096918372593),.UNSPECIFIED.);
#401=B_SPLINE_CURVE_WITH_KNOTS('',3,(#45018,#45019,#45020,#45021,#45022,
#45023,#45024,#45025,#45026,#45027,#45028,#45029,#45030,#45031,#45032,#45033,
#45034,#45035,#45036,#45037,#45038,#45039,#45040,#45041,#45042,#45043,#45044,
#45045,#45046,#45047,#45048,#45049,#45050,#45051,#45052,#45053,#45054,#45055,
#45056,#45057,#45058,#45059,#45060,#45061,#45062,#45063,#45064,#45065,#45066,
#45067,#45068,#45069,#45070,#45071,#45072,#45073,#45074,#45075,#45076,#45077,
#45078,#45079,#45080,#45081,#45082,#45083,#45084,#45085,#45086,#45087,#45088,
#45089,#45090,#45091,#45092,#45093,#45094,#45095,#45096),.UNSPECIFIED.,
 .F.,.F.,(4,3,3,3,3,3,3,3,3,3,3,3,3,3,3,3,3,3,3,3,3,3,3,3,3,3,4),(466.051432402393,
466.128100662332,466.204713834782,466.281288051319,466.357851539603,466.434411961159,
466.510983881253,466.587581869918,466.664267937965,466.740999464938,466.817853223278,
466.889084519038,466.966679188465,467.044181454569,467.121606939632,467.198971211002,
467.276289792086,467.353585496551,467.4308705412,467.508158933126,467.585464678645,
467.662842718626,467.740257790364,467.817778404628,467.887492527089,467.992398955984,
468.097305384879),.UNSPECIFIED.);
#402=B_SPLINE_CURVE_WITH_KNOTS('',3,(#45097,#45098,#45099,#45100,#45101,
#45102,#45103,#45104,#45105,#45106,#45107,#45108,#45109,#45110,#45111,#45112,
#45113,#45114,#45115,#45116,#45117,#45118,#45119,#45120,#45121,#45122,#45123,
#45124,#45125,#45126,#45127,#45128,#45129,#45130,#45131,#45132,#45133,#45134,
#45135,#45136,#45137,#45138,#45139,#45140,#45141,#45142,#45143,#45144,#45145,
#45146,#45147,#45148,#45149,#45150,#45151,#45152,#45153,#45154,#45155,#45156,
#45157,#45158,#45159,#45160,#45161,#45162,#45163,#45164,#45165,#45166,#45167,
#45168,#45169,#45170,#45171,#45172,#45173,#45174,#45175,#45176,#45177,#45178,
#45179,#45180,#45181,#45182,#45183,#45184,#45185,#45186,#45187,#45188,#45189,
#45190,#45191,#45192,#45193,#45194,#45195,#45196,#45197,#45198,#45199,#45200,
#45201,#45202,#45203,#45204,#45205,#45206,#45207,#45208,#45209,#45210,#45211,
#45212,#45213,#45214,#45215,#45216,#45217,#45218,#45219,#45220,#45221,#45222,
#45223,#45224,#45225,#45226,#45227,#45228,#45229,#45230,#45231,#45232,#45233,
#45234,#45235,#45236,#45237,#45238,#45239,#45240,#45241,#45242,#45243,#45244,
#45245,#45246,#45247,#45248,#45249,#45250,#45251,#45252,#45253,#45254,#45255,
#45256,#45257,#45258,#45259,#45260,#45261,#45262,#45263,#45264,#45265),
 .UNSPECIFIED.,.F.,.F.,(4,3,3,3,3,3,3,3,3,3,3,3,3,3,3,3,3,3,3,3,3,3,3,3,
3,3,3,3,3,3,3,3,3,3,3,3,3,3,3,3,3,3,3,3,3,3,3,3,3,3,3,3,3,3,3,3,4),(468.097305384968,
468.172742017472,468.248128780957,468.323482174757,468.386696531114,468.467709637285,
468.548798331437,468.633073882363,468.714383348627,468.795770249711,468.877277388349,
468.885900535139,468.963428688398,469.040875563409,469.118256742166,469.195587759677,
469.272884114558,469.350174414944,469.427464322733,469.504767844781,469.582098992958,
469.659518482829,469.7369838413,469.814569227647,469.88430854319,469.961171927862,
470.037941759691,470.1146342957,470.191265730887,470.267852211691,470.344710254135,
470.421268577119,470.497832911812,470.574417824961,470.651492506531,470.728199327421,
470.805457939331,470.882716551241,470.960246747535,471.037689841973,471.115061475862,
471.192377239264,471.269652681875,471.346913564128,471.424168869606,471.501432639735,
471.578718918054,471.656085730683,471.733494065228,471.811015621632,471.881124559292,
471.958659520324,472.036109852615,472.113473924364,472.19078786829,472.268064511653,
472.334165849073),.UNSPECIFIED.);
#403=B_SPLINE_CURVE_WITH_KNOTS('',3,(#45271,#45272,#45273,#45274,#45275,
#45276,#45277,#45278,#45279,#45280,#45281,#45282,#45283,#45284,#45285,#45286,
#45287,#45288,#45289,#45290,#45291,#45292,#45293,#45294,#45295,#45296,#45297,
#45298,#45299,#45300,#45301,#45302,#45303,#45304,#45305,#45306,#45307,#45308,
#45309,#45310,#45311,#45312,#45313,#45314,#45315,#45316,#45317,#45318,#45319,
#45320,#45321,#45322,#45323,#45324,#45325,#45326,#45327,#45328,#45329,#45330,
#45331,#45332,#45333,#45334,#45335,#45336,#45337,#45338,#45339,#45340,#45341,
#45342,#45343,#45344,#45345,#45346,#45347,#45348,#45349,#45350,#45351,#45352,
#45353,#45354,#45355,#45356,#45357,#45358,#45359,#45360,#45361,#45362,#45363,
#45364,#45365,#45366,#45367,#45368,#45369,#45370,#45371,#45372,#45373,#45374,
#45375,#45376,#45377,#45378,#45379,#45380,#45381,#45382,#45383,#45384,#45385,
#45386,#45387,#45388,#45389,#45390,#45391,#45392,#45393,#45394,#45395,#45396,
#45397,#45398,#45399,#45400,#45401,#45402,#45403,#45404,#45405,#45406,#45407,
#45408,#45409,#45410,#45411,#45412,#45413,#45414,#45415,#45416,#45417,#45418,
#45419,#45420,#45421,#45422,#45423,#45424,#45425,#45426,#45427,#45428,#45429,
#45430,#45431,#45432,#45433,#45434,#45435,#45436,#45437,#45438,#45439),
 .UNSPECIFIED.,.F.,.F.,(4,3,3,3,3,3,3,3,3,3,3,3,3,3,3,3,3,3,3,3,3,3,3,3,
3,3,3,3,3,3,3,3,3,3,3,3,3,3,3,3,3,3,3,3,3,3,3,3,3,3,3,3,3,3,3,3,4),(474.381281477029,
474.45785620268,474.534379006077,474.610866110696,474.687346011724,474.763825899523,
474.840320428267,474.91684425907,474.993454306524,475.070112975877,475.146881411406,
475.186065764122,475.262914397353,475.339669253825,475.416346603329,475.49296265322,
475.569533561969,475.646569288659,475.723111717468,475.799660064117,475.876228905626,
475.953626523092,476.030317613975,476.108068494733,476.185819375491,476.263336904457,
476.34076710121,476.418125621448,476.495428069405,476.572690008776,476.64993721213,
476.727178701002,476.804428529013,476.881700751837,476.959053688043,477.036448058732,
477.113956365229,477.18557298686,477.263090364072,477.340520439403,477.417878868409,
477.495181255212,477.57244316341,477.649690381279,477.726931912518,477.804181810723,
477.881454131557,477.958807209175,478.036201745166,478.113710256049,478.18532659823,
478.26215530598,478.338896867184,478.415549744414,478.492151381125,478.568713263294,
478.61726357937),.UNSPECIFIED.);
#404=B_SPLINE_CURVE_WITH_KNOTS('',3,(#45440,#45441,#45442,#45443,#45444,
#45445,#45446,#45447,#45448,#45449,#45450,#45451,#45452,#45453,#45454,#45455,
#45456,#45457,#45458,#45459,#45460,#45461,#45462,#45463,#45464,#45465,#45466,
#45467,#45468,#45469,#45470,#45471,#45472,#45473,#45474,#45475,#45476,#45477,
#45478,#45479,#45480,#45481,#45482,#45483,#45484,#45485,#45486,#45487,#45488,
#45489,#45490,#45491,#45492,#45493,#45494,#45495,#45496,#45497,#45498,#45499,
#45500,#45501,#45502,#45503,#45504,#45505,#45506,#45507,#45508,#45509,#45510,
#45511,#45512,#45513,#45514,#45515),.UNSPECIFIED.,.F.,.F.,(4,3,3,3,3,3,
3,3,3,3,3,3,3,3,3,3,3,3,3,3,3,3,3,3,3,4),(472.333968641244,472.416430245098,
472.498891183068,472.581351482554,472.663811170951,472.746270275653,472.828728824052,
472.911186843538,472.9936443615,473.080322256826,473.162789042661,473.245254156005,
473.32771770651,473.410179803808,473.492640557509,473.575100077206,473.657558472473,
473.74001585287,473.822482239137,473.90494544115,473.987405897431,474.069864046341,
474.15232965122,474.234789530434,474.317253643797,474.380490686714),
 .UNSPECIFIED.);
#405=B_SPLINE_CURVE_WITH_KNOTS('',3,(#45517,#45518,#45519,#45520,#45521,
#45522,#45523,#45524,#45525,#45526,#45527,#45528,#45529,#45530,#45531,#45532,
#45533,#45534,#45535,#45536,#45537,#45538,#45539,#45540,#45541,#45542,#45543,
#45544,#45545,#45546,#45547,#45548,#45549,#45550,#45551,#45552,#45553,#45554,
#45555,#45556,#45557,#45558,#45559,#45560,#45561,#45562,#45563,#45564,#45565,
#45566,#45567,#45568,#45569,#45570,#45571,#45572,#45573,#45574,#45575,#45576,
#45577,#45578,#45579,#45580,#45581,#45582,#45583,#45584,#45585,#45586,#45587,
#45588,#45589,#45590,#45591,#45592,#45593,#45594,#45595),.UNSPECIFIED.,
 .F.,.F.,(4,3,3,3,3,3,3,3,3,3,3,3,3,3,3,3,3,3,3,3,3,3,3,3,3,3,4),(472.334165849073,
472.411421096754,472.488682793709,472.565964982701,472.644356878861,472.721759112864,
472.800645840103,472.879532567343,472.956368599592,473.033115615447,473.10978985314,
473.186407492793,473.262984669552,473.339854157782,473.416414260441,473.492984557726,
473.569579618888,473.646669858014,473.723397054735,473.800668815065,473.877940575394,
473.960532450875,474.042978969928,474.127356900436,474.209459716935,474.294975204449,
474.380490691962),.UNSPECIFIED.);
#406=B_SPLINE_CURVE_WITH_KNOTS('',3,(#45596,#45597,#45598,#45599,#45600,
#45601,#45602,#45603,#45604,#45605,#45606,#45607,#45608,#45609,#45610,#45611,
#45612,#45613,#45614,#45615,#45616,#45617,#45618,#45619,#45620,#45621,#45622,
#45623,#45624,#45625,#45626,#45627,#45628,#45629,#45630,#45631,#45632,#45633,
#45634,#45635,#45636,#45637,#45638,#45639,#45640,#45641,#45642,#45643,#45644,
#45645,#45646,#45647,#45648,#45649,#45650,#45651,#45652,#45653,#45654,#45655,
#45656,#45657,#45658,#45659,#45660,#45661,#45662,#45663,#45664,#45665,#45666,
#45667,#45668,#45669,#45670,#45671,#45672,#45673,#45674,#45675,#45676,#45677,
#45678,#45679,#45680,#45681,#45682,#45683,#45684,#45685,#45686,#45687,#45688,
#45689,#45690,#45691,#45692,#45693,#45694,#45695,#45696,#45697,#45698,#45699,
#45700,#45701,#45702,#45703,#45704,#45705,#45706,#45707,#45708,#45709,#45710,
#45711,#45712,#45713,#45714,#45715,#45716,#45717,#45718,#45719,#45720,#45721,
#45722,#45723,#45724,#45725,#45726,#45727,#45728,#45729,#45730,#45731,#45732,
#45733,#45734,#45735,#45736,#45737,#45738,#45739,#45740,#45741,#45742,#45743,
#45744,#45745,#45746,#45747,#45748,#45749,#45750,#45751,#45752,#45753,#45754,
#45755,#45756,#45757,#45758,#45759,#45760,#45761,#45762,#45763,#45764,#45765,
#45766,#45767),.UNSPECIFIED.,.F.,.F.,(4,3,3,3,3,3,3,3,3,3,3,3,3,3,3,3,3,
3,3,3,3,3,3,3,3,3,3,3,3,3,3,3,3,3,3,3,3,3,3,3,3,3,3,3,3,3,3,3,3,3,3,3,3,
3,3,3,3,4),(474.380490692059,474.460535231213,474.540649030064,474.624573918409,
474.704907259135,474.785320660555,474.865863059083,474.876348583445,474.957834908585,
475.03921700152,475.123300898008,475.204458226965,475.285539020607,475.366529022188,
475.37555258747,475.456565678807,475.53765435784,475.621929916254,475.703239366989,
475.784626252454,475.866133375462,475.874756591496,475.952284746877,476.029731624016,
476.107112804903,476.184443824544,476.261740181554,476.33903048406,476.416320393962,
476.493623918116,476.570955068389,476.648374560329,476.725839920858,476.803425309224,
476.873164599547,476.950027994422,477.026797836485,477.10349038275,477.18012182821,
477.256708319294,477.333566355332,477.410124688572,477.486689033502,477.563273956862,
477.640348619546,477.71705545051,477.794314029054,477.871572607598,477.949116904188,
478.02657129614,478.103935562688,478.181248091713,478.258522970496,478.335774262294,
478.413031632214,478.49029111365,478.567591847394,478.616565862282),
 .UNSPECIFIED.);
#407=B_SPLINE_CURVE_WITH_KNOTS('',3,(#45773,#45774,#45775,#45776,#45777,
#45778,#45779,#45780,#45781,#45782,#45783,#45784,#45785,#45786,#45787,#45788,
#45789,#45790,#45791,#45792,#45793,#45794,#45795,#45796,#45797,#45798,#45799,
#45800,#45801,#45802,#45803,#45804,#45805,#45806,#45807,#45808,#45809,#45810,
#45811,#45812,#45813,#45814,#45815,#45816,#45817,#45818,#45819,#45820,#45821,
#45822,#45823,#45824,#45825,#45826,#45827,#45828,#45829,#45830,#45831,#45832,
#45833,#45834,#45835,#45836,#45837,#45838,#45839,#45840,#45841,#45842,#45843,
#45844,#45845,#45846,#45847,#45848,#45849,#45850,#45851,#45852,#45853,#45854,
#45855,#45856,#45857,#45858,#45859,#45860,#45861,#45862,#45863,#45864,#45865,
#45866,#45867,#45868,#45869,#45870,#45871,#45872,#45873,#45874,#45875,#45876,
#45877,#45878,#45879,#45880,#45881,#45882,#45883,#45884,#45885,#45886,#45887,
#45888,#45889,#45890,#45891,#45892,#45893,#45894,#45895,#45896,#45897,#45898,
#45899,#45900,#45901,#45902,#45903,#45904,#45905,#45906,#45907,#45908,#45909,
#45910,#45911,#45912,#45913,#45914,#45915,#45916,#45917,#45918,#45919,#45920,
#45921,#45922,#45923,#45924,#45925,#45926,#45927,#45928,#45929,#45930,#45931,
#45932,#45933,#45934,#45935,#45936,#45937,#45938,#45939,#45940,#45941,#45942,
#45943,#45944),.UNSPECIFIED.,.F.,.F.,(4,3,3,3,3,3,3,3,3,3,3,3,3,3,3,3,3,
3,3,3,3,3,3,3,3,3,3,3,3,3,3,3,3,3,3,3,3,3,3,3,3,3,3,3,3,3,3,3,3,3,3,3,3,
3,3,3,3,4),(480.663675999238,480.684710626653,480.765718118816,480.846801459616,
480.931247952797,481.012553105523,481.09393596496,481.175439700502,481.184587432338,
481.262102728308,481.339536542789,481.416904472146,481.494222065579,481.571504835749,
481.648781424568,481.726057508624,481.803347107084,481.880664244083,481.958069955971,
482.035521471495,482.11309379188,482.184341043707,482.261191456613,482.33794809446,
482.414627225727,482.491245056489,482.567817743952,482.644852357843,482.721396552421,
482.797946658388,482.874517251629,482.951911602491,483.028604413594,483.106349534335,
483.184094655077,483.261610631392,483.339039282175,483.416396264486,483.493697183922,
483.57095760554,483.648203312351,483.725443317765,483.802691676646,483.879962445922,
483.957313960686,484.03470692534,484.112213865109,484.183848266446,484.261378360035,
484.341194605466,484.418541443881,484.495836336518,484.573093386162,484.650326671363,
484.727562409331,484.8048003573,484.882070368431,484.899908323481),
 .UNSPECIFIED.);
#408=B_SPLINE_CURVE_WITH_KNOTS('',3,(#45945,#45946,#45947,#45948,#45949,
#45950,#45951,#45952,#45953,#45954,#45955,#45956,#45957,#45958,#45959,#45960,
#45961,#45962,#45963,#45964,#45965,#45966,#45967,#45968,#45969,#45970,#45971,
#45972,#45973,#45974,#45975,#45976,#45977,#45978,#45979,#45980,#45981,#45982,
#45983,#45984,#45985,#45986,#45987,#45988,#45989,#45990,#45991,#45992,#45993,
#45994,#45995,#45996,#45997,#45998,#45999,#46000,#46001,#46002,#46003,#46004,
#46005,#46006,#46007,#46008,#46009,#46010,#46011,#46012,#46013,#46014,#46015,
#46016,#46017,#46018,#46019,#46020,#46021,#46022,#46023,#46024,#46025,#46026),
 .UNSPECIFIED.,.F.,.F.,(4,3,3,3,3,3,3,3,3,3,3,3,3,3,3,3,3,3,3,3,3,3,3,3,
3,3,3,4),(478.61726357937,478.693807784374,478.770356670326,478.846924814219,
478.923526802521,479.000219846047,479.07696535096,479.153821951485,479.185080209599,
479.262662623704,479.340152397017,479.417565166163,479.494916512606,479.572221973682,
479.64950436344,479.726775948689,479.804050748628,479.881342781611,479.958707260156,
480.036108676756,480.113616304678,480.184833820968,480.266932938396,480.348920644616,
480.430754232682,480.512494601567,480.594104446945,480.663675999104),
 .UNSPECIFIED.);
#409=B_SPLINE_CURVE_WITH_KNOTS('',3,(#46028,#46029,#46030,#46031,#46032,
#46033,#46034,#46035,#46036,#46037,#46038,#46039,#46040,#46041,#46042,#46043,
#46044,#46045,#46046,#46047,#46048,#46049,#46050,#46051,#46052,#46053,#46054,
#46055,#46056,#46057,#46058,#46059,#46060,#46061,#46062,#46063,#46064,#46065,
#46066,#46067,#46068,#46069,#46070,#46071,#46072,#46073,#46074,#46075,#46076,
#46077,#46078,#46079,#46080,#46081,#46082,#46083,#46084,#46085,#46086,#46087,
#46088,#46089,#46090,#46091,#46092,#46093,#46094,#46095,#46096,#46097,#46098,
#46099,#46100,#46101,#46102,#46103,#46104,#46105,#46106,#46107,#46108,#46109,
#46110,#46111,#46112),.UNSPECIFIED.,.F.,.F.,(4,3,3,3,3,3,3,3,3,3,3,3,3,
3,3,3,3,3,3,3,3,3,3,3,3,3,3,3,4),(478.616565862282,478.693957480818,478.771398631114,
478.848940229736,478.869980615649,478.947510740726,479.024953776917,479.102325365474,
479.179641096418,479.256916519409,479.334177401614,479.411432718986,479.488696512945,
479.565982827034,479.643349694059,479.720758093262,479.798279731107,479.8683886237,
479.944116203083,480.019754722875,480.095321134249,480.170827543791,480.246301274037,
480.321757502312,480.397211390023,480.472705398315,480.548221608717,480.623809108532,
480.662500463276),.UNSPECIFIED.);
#410=B_SPLINE_CURVE_WITH_KNOTS('',3,(#46113,#46114,#46115,#46116,#46117,
#46118,#46119,#46120,#46121,#46122,#46123,#46124,#46125,#46126,#46127,#46128,
#46129,#46130,#46131,#46132,#46133,#46134,#46135,#46136,#46137,#46138,#46139,
#46140,#46141,#46142,#46143,#46144,#46145,#46146,#46147,#46148,#46149,#46150,
#46151,#46152,#46153,#46154,#46155,#46156,#46157,#46158,#46159,#46160,#46161,
#46162,#46163,#46164,#46165,#46166,#46167,#46168,#46169,#46170,#46171,#46172,
#46173,#46174,#46175,#46176,#46177,#46178,#46179,#46180,#46181,#46182,#46183,
#46184,#46185,#46186,#46187,#46188,#46189,#46190,#46191,#46192,#46193,#46194,
#46195,#46196,#46197,#46198,#46199,#46200,#46201,#46202,#46203,#46204,#46205,
#46206,#46207,#46208,#46209,#46210,#46211,#46212,#46213,#46214,#46215,#46216,
#46217,#46218,#46219,#46220,#46221,#46222,#46223,#46224,#46225,#46226,#46227,
#46228,#46229,#46230,#46231,#46232,#46233,#46234,#46235,#46236,#46237,#46238,
#46239,#46240,#46241,#46242,#46243,#46244,#46245,#46246,#46247,#46248,#46249,
#46250,#46251,#46252,#46253,#46254,#46255,#46256,#46257,#46258,#46259,#46260,
#46261,#46262,#46263,#46264,#46265,#46266,#46267,#46268,#46269),
 .UNSPECIFIED.,.F.,.F.,(4,3,3,3,3,3,3,3,3,3,3,3,3,3,3,3,3,3,3,3,3,3,3,3,
3,3,3,3,3,3,3,3,3,3,3,3,3,3,3,3,3,3,3,3,3,3,3,3,3,3,3,3,4),(480.663675999238,
480.746138205274,480.828600063014,480.911061579308,480.993522761005,481.075983614956,
481.158444148011,481.240904367017,481.323364278825,481.405823890283,481.488283208239,
481.570742239541,481.653200991038,481.735659469576,481.818117682004,481.900575635168,
481.983033335916,482.065490791094,482.147948007548,482.23396023405,482.317284578474,
482.399751183919,482.482216945161,482.564681889613,482.647146044689,482.729609437798,
482.812072096347,482.894534047739,482.976995319378,483.059455938662,483.141915932989,
483.224375329753,483.306834156349,483.389292440165,483.471750208593,483.554207489018,
483.63834072443,483.720806722521,483.803271098877,483.885733963139,483.96819542493,
484.050655593851,484.133114579486,484.215572491404,484.301168336929,484.383633073529,
484.466094845531,484.548554091373,484.63101124935,484.713473767631,484.795931438486,
484.878390228437,484.900339255603),.UNSPECIFIED.);
#411=B_SPLINE_CURVE_WITH_KNOTS('',3,(#46275,#46276,#46277,#46278,#46279,
#46280,#46281,#46282,#46283,#46284,#46285,#46286,#46287,#46288,#46289,#46290,
#46291,#46292,#46293,#46294,#46295,#46296,#46297,#46298,#46299,#46300,#46301,
#46302,#46303,#46304,#46305,#46306,#46307,#46308,#46309,#46310,#46311,#46312,
#46313,#46314,#46315,#46316,#46317,#46318,#46319,#46320,#46321,#46322,#46323,
#46324,#46325,#46326,#46327,#46328,#46329,#46330,#46331,#46332,#46333,#46334,
#46335,#46336,#46337,#46338,#46339,#46340,#46341,#46342,#46343,#46344,#46345,
#46346,#46347,#46348,#46349,#46350,#46351,#46352,#46353,#46354,#46355,#46356,
#46357,#46358,#46359,#46360,#46361,#46362,#46363,#46364,#46365,#46366,#46367,
#46368,#46369,#46370,#46371,#46372,#46373,#46374,#46375,#46376,#46377,#46378,
#46379,#46380,#46381,#46382,#46383,#46384,#46385,#46386,#46387,#46388,#46389,
#46390,#46391,#46392,#46393,#46394,#46395,#46396,#46397,#46398,#46399,#46400,
#46401,#46402,#46403,#46404,#46405,#46406,#46407,#46408,#46409,#46410,#46411,
#46412,#46413,#46414,#46415,#46416,#46417,#46418,#46419,#46420,#46421,#46422,
#46423,#46424,#46425,#46426,#46427,#46428,#46429,#46430,#46431,#46432,#46433,
#46434,#46435,#46436,#46437,#46438,#46439,#46440,#46441,#46442,#46443,#46444,
#46445,#46446),.UNSPECIFIED.,.F.,.F.,(4,3,3,3,3,3,3,3,3,3,3,3,3,3,3,3,3,
3,3,3,3,3,3,3,3,3,3,3,3,3,3,3,3,3,3,3,3,3,3,3,3,3,3,3,3,3,3,3,3,3,3,3,3,
3,3,3,3,4),(486.946861306558,487.044487898057,487.143729854774,487.183109100554,
487.264573506176,487.345932819536,487.430196091212,487.511328644414,487.59238417966,
487.673348279245,487.682985906239,487.764098416933,487.845289914188,487.929683113621,
488.011102046416,488.092600239478,488.174220613748,488.182862711923,488.26023174493,
488.337518441393,488.414738542001,488.491907739137,488.569041687839,488.646169300824,
488.723296324374,488.800436904579,488.877605192613,488.954863121079,489.032167203152,
489.109594111933,489.182616323293,489.259647825886,489.336585302471,489.413444889173,
489.490242661691,489.566994648111,489.64391655893,489.720637692983,489.797363683864,
489.874108990205,489.951174226319,490.028037590024,490.105203762343,490.182369934662,
490.259996871395,490.337538182827,490.415009395564,490.492425986359,490.569803392715,
490.64716767186,490.724527198585,490.801895915988,490.879287769664,490.956760855184,
491.034275833432,491.111904375155,491.182123546032,491.183619892445),
 .UNSPECIFIED.);
#412=B_SPLINE_CURVE_WITH_KNOTS('',3,(#46447,#46448,#46449,#46450,#46451,
#46452,#46453,#46454,#46455,#46456,#46457,#46458,#46459,#46460,#46461,#46462,
#46463,#46464,#46465,#46466,#46467,#46468,#46469,#46470,#46471,#46472,#46473,
#46474,#46475,#46476,#46477,#46478,#46479,#46480,#46481,#46482,#46483,#46484,
#46485,#46486,#46487,#46488,#46489,#46490,#46491,#46492,#46493,#46494,#46495,
#46496,#46497,#46498,#46499,#46500,#46501,#46502,#46503,#46504,#46505,#46506,
#46507,#46508,#46509,#46510,#46511,#46512,#46513,#46514,#46515,#46516,#46517,
#46518,#46519,#46520,#46521,#46522,#46523,#46524,#46525,#46526,#46527,#46528),
 .UNSPECIFIED.,.F.,.F.,(4,3,3,3,3,3,3,3,3,3,3,3,3,3,3,3,3,3,3,3,3,3,3,3,
3,3,3,4),(484.899908323481,484.977267642619,485.054671733857,485.132184395316,
485.183601877815,485.260435582513,485.337180053993,485.41385153389,485.490466205502,
485.567040206957,485.644079617235,485.720636132414,485.797202697583,485.873793884144,
485.951184285404,486.027907737698,486.105631613442,486.183355489185,486.26034438458,
486.337238710065,486.414037400464,486.490781268223,486.567484870917,486.644162739328,
486.720847671068,486.797533478452,486.874268418715,486.946861306418),
 .UNSPECIFIED.);
#413=B_SPLINE_CURVE_WITH_KNOTS('',3,(#46530,#46531,#46532,#46533,#46534,
#46535,#46536,#46537,#46538,#46539,#46540,#46541,#46542,#46543,#46544,#46545,
#46546,#46547,#46548,#46549,#46550,#46551,#46552,#46553,#46554,#46555,#46556,
#46557,#46558,#46559,#46560,#46561,#46562,#46563,#46564,#46565,#46566,#46567,
#46568,#46569,#46570,#46571,#46572,#46573,#46574,#46575,#46576,#46577,#46578,
#46579,#46580,#46581,#46582,#46583,#46584,#46585,#46586,#46587,#46588,#46589,
#46590,#46591,#46592,#46593,#46594,#46595,#46596,#46597,#46598,#46599,#46600,
#46601,#46602,#46603,#46604,#46605),.UNSPECIFIED.,.F.,.F.,(4,3,3,3,3,3,
3,3,3,3,3,3,3,3,3,3,3,3,3,3,3,3,3,3,3,4),(484.900339255603,484.982800859457,
485.065261797427,485.147722096913,485.23018178531,485.312640890012,485.395099438411,
485.477557457898,485.560014975859,485.646692871519,485.729159657355,485.811624770699,
485.894088321204,485.976550418501,486.059011172203,486.1414706919,486.223929087168,
486.306386467565,486.388852853831,486.471316055845,486.553776512125,486.636234661036,
486.718700265915,486.80116014513,486.883624258494,486.946861306418),
 .UNSPECIFIED.);
#414=B_SPLINE_CURVE_WITH_KNOTS('',3,(#46606,#46607,#46608,#46609,#46610,
#46611,#46612,#46613,#46614,#46615,#46616,#46617,#46618,#46619,#46620,#46621,
#46622,#46623,#46624,#46625,#46626,#46627,#46628,#46629,#46630,#46631,#46632,
#46633,#46634,#46635,#46636,#46637,#46638,#46639,#46640,#46641,#46642,#46643,
#46644,#46645,#46646,#46647,#46648,#46649,#46650,#46651,#46652,#46653,#46654,
#46655,#46656,#46657,#46658,#46659,#46660,#46661,#46662,#46663,#46664,#46665,
#46666,#46667,#46668,#46669,#46670,#46671,#46672,#46673,#46674,#46675,#46676,
#46677,#46678,#46679,#46680,#46681,#46682,#46683,#46684,#46685,#46686,#46687,
#46688,#46689,#46690,#46691,#46692,#46693,#46694,#46695,#46696,#46697,#46698,
#46699,#46700,#46701,#46702,#46703,#46704,#46705,#46706,#46707,#46708,#46709,
#46710,#46711,#46712,#46713,#46714,#46715,#46716,#46717,#46718,#46719,#46720,
#46721,#46722,#46723,#46724,#46725,#46726,#46727,#46728,#46729,#46730,#46731,
#46732,#46733,#46734,#46735,#46736,#46737,#46738,#46739,#46740,#46741,#46742,
#46743,#46744,#46745,#46746,#46747,#46748,#46749,#46750,#46751,#46752,#46753,
#46754,#46755,#46756,#46757,#46758,#46759,#46760,#46761,#46762,#46763,#46764,
#46765,#46766,#46767,#46768,#46769,#46770,#46771,#46772,#46773,#46774),
 .UNSPECIFIED.,.F.,.F.,(4,3,3,3,3,3,3,3,3,3,3,3,3,3,3,3,3,3,3,3,3,3,3,3,
3,3,3,3,3,3,3,3,3,3,3,3,3,3,3,3,3,3,3,3,3,3,3,3,3,3,3,3,3,3,3,3,4),(486.947493603795,
487.023416751433,487.099259735571,487.175039333094,487.25077225503,487.326484557484,
487.402187752868,487.477896898353,487.553627054983,487.629439912187,487.705294636798,
487.781269679046,487.855652688107,487.933234538829,488.010724097938,488.088136999181,
488.1654888214,488.242795099555,488.320078763446,488.39735192979,488.474628616324,
488.551922840107,488.629289707096,488.70669378104,488.784203794078,488.854060696158,
488.935525654771,489.016885920646,489.10098061553,489.182115309453,489.263173304526,
489.344140380854,489.353264700183,489.434384302318,489.51558265585,489.599804167939,
489.681228944152,489.76684882418,489.852468704209,489.929849868594,490.00714889331,
490.084381506189,490.161563386952,490.238710178132,490.315850761355,490.392990868986,
490.470144636184,490.547326203241,490.624597185865,490.701914393361,490.779353655883,
490.85087671226,490.927942593232,491.004889365967,491.08176741454,491.158578222174,
491.184226656328),.UNSPECIFIED.);
#415=B_SPLINE_CURVE_WITH_KNOTS('',3,(#46777,#46778,#46779,#46780,#46781,
#46782,#46783,#46784,#46785,#46786,#46787,#46788,#46789,#46790,#46791,#46792,
#46793,#46794,#46795,#46796,#46797,#46798,#46799,#46800,#46801,#46802,#46803,
#46804,#46805,#46806,#46807,#46808,#46809,#46810,#46811,#46812,#46813,#46814,
#46815,#46816,#46817,#46818,#46819,#46820,#46821,#46822,#46823,#46824,#46825,
#46826,#46827,#46828,#46829,#46830,#46831,#46832,#46833,#46834,#46835,#46836,
#46837,#46838,#46839,#46840,#46841,#46842,#46843,#46844,#46845,#46846,#46847,
#46848,#46849,#46850,#46851,#46852,#46853,#46854,#46855,#46856,#46857,#46858),
 .UNSPECIFIED.,.F.,.F.,(4,3,3,3,3,3,3,3,3,3,3,3,3,3,3,3,3,3,3,3,3,3,3,3,
3,3,3,4),(491.184226656328,491.260981276608,491.337721764863,491.414457587017,
491.491203190154,491.567973024665,491.644823201061,491.721717208307,491.798719032839,
491.849284720311,491.926926082042,492.004482049841,492.081968133548,492.159399793344,
492.236792450328,492.314172138313,492.391547200536,492.468931565718,492.546339165133,
492.623827783714,492.701358365424,492.779001757603,492.847692728361,492.93409170758,
493.020099915774,493.10585418754,493.191201426576,493.230046613597),
 .UNSPECIFIED.);
#416=B_SPLINE_CURVE_WITH_KNOTS('',3,(#46860,#46861,#46862,#46863,#46864,
#46865,#46866,#46867,#46868,#46869,#46870,#46871,#46872,#46873,#46874,#46875,
#46876,#46877,#46878,#46879,#46880,#46881,#46882,#46883,#46884,#46885,#46886,
#46887,#46888,#46889,#46890,#46891,#46892,#46893,#46894,#46895,#46896,#46897,
#46898,#46899,#46900,#46901,#46902,#46903,#46904,#46905,#46906,#46907,#46908,
#46909,#46910,#46911,#46912,#46913,#46914,#46915,#46916,#46917,#46918,#46919,
#46920,#46921,#46922,#46923,#46924,#46925,#46926,#46927,#46928,#46929,#46930,
#46931,#46932,#46933,#46934,#46935,#46936,#46937,#46938,#46939,#46940,#46941),
 .UNSPECIFIED.,.F.,.F.,(4,3,3,3,3,3,3,3,3,3,3,3,3,3,3,3,3,3,3,3,3,3,3,3,
3,3,3,4),(493.230046613597,493.312509443594,493.394971559946,493.477432990057,
493.559893761326,493.64235390115,493.724813436927,493.807272396048,493.889730805905,
493.972188693888,494.054646087385,494.139999550714,494.222465923618,494.304930650447,
494.38739384085,494.469855604453,494.552316050861,494.634775289664,494.717233430432,
494.799690582719,494.882156161897,494.964618662462,495.047078522896,495.129536181529,
495.212000247102,495.294459009407,495.376920343153,495.420301500648),
 .UNSPECIFIED.);
#417=B_SPLINE_CURVE_WITH_KNOTS('',3,(#46945,#46946,#46947,#46948,#46949,
#46950,#46951,#46952,#46953,#46954,#46955,#46956,#46957,#46958,#46959,#46960,
#46961,#46962,#46963,#46964,#46965,#46966,#46967,#46968,#46969,#46970,#46971,
#46972,#46973,#46974,#46975,#46976,#46977,#46978,#46979,#46980,#46981),
 .UNSPECIFIED.,.F.,.F.,(4,3,3,3,3,3,3,3,3,3,3,3,4),(493.230046613687,493.306330725309,
493.382561304179,493.458756735131,493.534929937347,493.611114993347,493.681507574455,
493.771594988047,493.861949931434,493.952493420372,494.043038074755,494.133417017897,
494.18138438014),.UNSPECIFIED.);
#418=B_SPLINE_CURVE_WITH_KNOTS('',3,(#46982,#46983,#46984,#46985,#46986,
#46987,#46988,#46989,#46990,#46991,#46992,#46993,#46994,#46995,#46996,#46997,
#46998,#46999,#47000,#47001,#47002,#47003,#47004,#47005,#47006,#47007,#47008,
#47009,#47010,#47011,#47012,#47013,#47014,#47015,#47016,#47017,#47018,#47019,
#47020,#47021,#47022,#47023,#47024,#47025,#47026,#47027,#47028,#47029,#47030,
#47031,#47032,#47033,#47034,#47035,#47036,#47037,#47038,#47039,#47040,#47041,
#47042,#47043,#47044,#47045,#47046,#47047,#47048,#47049,#47050,#47051,#47052,
#47053,#47054,#47055,#47056,#47057,#47058,#47059,#47060,#47061,#47062,#47063),
 .UNSPECIFIED.,.F.,.F.,(4,3,3,3,3,3,3,3,3,3,3,3,3,3,3,3,3,3,3,3,3,3,3,3,
3,3,3,4),(491.183619892445,491.260274943168,491.336841384986,491.413335588533,
491.489773864164,491.566172475915,491.6431355611,491.719519875166,491.795915578857,
491.872337359501,491.949722308976,492.026280748062,492.104078952732,492.181877157401,
492.260273681847,492.338574297521,492.41679371464,492.494946586276,492.573047518285,
492.65111327471,492.729160503911,492.80720237782,492.885252062782,492.963355326503,
493.0414860081,493.119700448305,493.18163076877,493.230046613597),
 .UNSPECIFIED.);
#419=B_SPLINE_CURVE_WITH_KNOTS('',3,(#47067,#47068,#47069,#47070,#47071,
#47072,#47073,#47074),.UNSPECIFIED.,.F.,.F.,(4,2,2,4),(-4.092356615175,
-3.25801350823578,-2.42309659634093,-2.07498647268394),.UNSPECIFIED.);
#420=B_SPLINE_CURVE_WITH_KNOTS('',3,(#47078,#47079,#47080,#47081,#47082,
#47083,#47084,#47085,#47086,#47087,#47088,#47089,#47090,#47091,#47092,#47093,
#47094,#47095,#47096,#47097,#47098,#47099,#47100,#47101,#47102,#47103,#47104,
#47105,#47106,#47107,#47108,#47109,#47110,#47111,#47112,#47113,#47114,#47115,
#47116,#47117,#47118,#47119,#47120),.UNSPECIFIED.,.F.,.F.,(4,3,3,3,3,3,
3,3,3,3,3,3,3,3,4),(1.45814303507282E-15,0.0869025370684598,0.173949593837137,
0.261014425040484,0.347993527889018,0.434679052537863,0.499876805684693,
0.574356627358125,0.64882817249345,0.723303820461166,0.797823564118164,
0.87236646746495,0.946980958560742,0.999753611369385,1.12364870614456),
 .UNSPECIFIED.);
#421=B_SPLINE_CURVE_WITH_KNOTS('',3,(#47122,#47123,#47124,#47125,#47126,
#47127,#47128,#47129,#47130,#47131,#47132,#47133,#47134,#47135,#47136,#47137,
#47138,#47139,#47140,#47141,#47142,#47143,#47144,#47145,#47146,#47147,#47148,
#47149,#47150,#47151,#47152,#47153,#47154,#47155,#47156,#47157,#47158,#47159,
#47160,#47161,#47162,#47163,#47164,#47165,#47166,#47167,#47168,#47169,#47170,
#47171,#47172,#47173,#47174,#47175,#47176,#47177,#47178,#47179,#47180,#47181,
#47182,#47183,#47184,#47185,#47186,#47187,#47188,#47189,#47190,#47191,#47192,
#47193,#47194,#47195,#47196,#47197,#47198,#47199,#47200,#47201,#47202,#47203,
#47204,#47205,#47206,#47207,#47208,#47209,#47210,#47211,#47212,#47213,#47214,
#47215,#47216,#47217,#47218,#47219,#47220,#47221,#47222,#47223,#47224,#47225,
#47226,#47227,#47228,#47229,#47230,#47231,#47232,#47233,#47234,#47235,#47236,
#47237,#47238,#47239,#47240,#47241,#47242,#47243,#47244,#47245,#47246,#47247,
#47248,#47249,#47250,#47251,#47252,#47253,#47254,#47255,#47256,#47257,#47258,
#47259,#47260,#47261,#47262,#47263,#47264,#47265,#47266,#47267,#47268,#47269,
#47270,#47271,#47272,#47273,#47274,#47275,#47276,#47277,#47278,#47279,#47280,
#47281,#47282,#47283,#47284,#47285,#47286,#47287,#47288,#47289,#47290,#47291,
#47292,#47293,#47294,#47295,#47296,#47297,#47298,#47299,#47300,#47301,#47302,
#47303,#47304,#47305,#47306,#47307,#47308,#47309,#47310,#47311,#47312,#47313,
#47314,#47315,#47316,#47317,#47318,#47319,#47320,#47321,#47322,#47323,#47324,
#47325,#47326,#47327,#47328,#47329,#47330,#47331,#47332,#47333,#47334,#47335,
#47336,#47337,#47338,#47339,#47340,#47341,#47342,#47343,#47344,#47345,#47346,
#47347,#47348,#47349,#47350,#47351,#47352,#47353,#47354,#47355,#47356,#47357,
#47358,#47359,#47360,#47361,#47362,#47363,#47364,#47365,#47366,#47367,#47368,
#47369,#47370,#47371,#47372,#47373,#47374,#47375,#47376,#47377,#47378,#47379,
#47380,#47381,#47382,#47383),.UNSPECIFIED.,.F.,.F.,(4,3,3,3,3,3,3,3,3,3,
3,3,3,3,3,3,3,3,3,3,3,3,3,3,3,3,3,3,3,3,3,3,3,3,3,3,3,3,3,3,3,3,3,3,3,3,
3,3,3,3,3,3,3,3,3,3,3,3,3,3,3,3,3,3,3,3,3,3,3,3,3,3,3,3,3,3,3,3,3,3,3,3,
3,3,3,3,3,4),(1.12364870625865,1.19799676400753,1.27229201830982,1.3465483781602,
1.42077972594984,1.49501440487335,1.5692543466832,1.64351211019356,1.71780026139656,
1.7921745179453,1.86659479891783,1.94112608036292,1.99950722273875,2.07326886306519,
2.14694154485294,2.22053985865856,2.29407833719155,2.36757146738224,2.44103370143537,
2.51449117423725,2.5879495180571,2.6614217918124,2.73492106084282,2.80849966885792,
2.88212232271905,2.9558467552384,2.99926083410811,3.07392477490812,3.1485076667527,
3.22302332634866,3.29748552634202,3.37190800412445,3.44630447027535,3.52070089524939,
3.59510114765806,3.66951762969037,3.74396274972424,3.81848536363884,3.89305240626076,
3.96771417016438,3.99901444547747,4.07305531525637,4.14701541720727,4.22090907995211,
4.2947505848787,4.36855417637488,4.44233407140981,4.51611917832578,4.5899113847781,
4.66372355262109,4.73756855269211,4.81150023318393,4.8854806822806,4.95956736916572,
4.99876805684683,5.07323997833421,5.14762491351672,5.22193690173382,5.29618993338574,
5.37039795939829,5.44457490016529,5.51874487792235,5.59291439456977,5.66709603139468,
5.7413023738179,5.81558137441948,5.88990170993551,5.96431394950146,5.99852166821619,
6.07699584702591,6.1553719672994,6.23365495938674,6.31181720086211,6.38990543199449,
6.46790051375185,6.49839847390087,6.57628401760595,6.65423975186325,6.73227087791391,
6.81043242117976,6.88866516313746,6.96701851048475,6.99827527958555,7.07919527083627,
7.16110495645824,7.24163505948288,7.32423453640351,7.40683401332414),
 .UNSPECIFIED.);
#422=B_SPLINE_CURVE_WITH_KNOTS('',3,(#47385,#47386,#47387,#47388,#47389,
#47390,#47391,#47392,#47393,#47394,#47395,#47396,#47397,#47398,#47399,#47400,
#47401,#47402),.UNSPECIFIED.,.F.,.F.,(4,2,2,2,2,2,2,2,4),(7.40683401332414,
8.241750925219,9.07666783711385,9.91158474900871,10.7465016609036,11.5814185727984,
12.4163354846933,13.2512523965881,13.6900193205037),.UNSPECIFIED.);
#423=B_SPLINE_CURVE_WITH_KNOTS('',3,(#47404,#47405,#47406,#47407,#47408,
#47409,#47410,#47411,#47412,#47413,#47414,#47415,#47416,#47417,#47418,#47419,
#47420,#47421,#47422,#47423,#47424,#47425,#47426,#47427,#47428,#47429,#47430,
#47431,#47432,#47433,#47434,#47435,#47436,#47437,#47438,#47439,#47440,#47441,
#47442,#47443,#47444,#47445,#47446,#47447,#47448,#47449,#47450,#47451,#47452,
#47453,#47454,#47455,#47456,#47457,#47458,#47459,#47460,#47461,#47462,#47463,
#47464,#47465,#47466,#47467,#47468,#47469,#47470,#47471,#47472,#47473,#47474,
#47475,#47476,#47477,#47478,#47479,#47480,#47481,#47482,#47483,#47484,#47485,
#47486,#47487,#47488,#47489,#47490,#47491,#47492,#47493,#47494,#47495,#47496,
#47497,#47498,#47499,#47500,#47501,#47502,#47503,#47504,#47505,#47506,#47507,
#47508,#47509,#47510,#47511,#47512,#47513,#47514,#47515,#47516,#47517,#47518,
#47519,#47520,#47521,#47522,#47523,#47524,#47525,#47526,#47527,#47528,#47529,
#47530,#47531,#47532,#47533,#47534,#47535,#47536,#47537,#47538,#47539,#47540,
#47541,#47542,#47543,#47544,#47545,#47546,#47547,#47548,#47549,#47550,#47551,
#47552,#47553,#47554,#47555,#47556,#47557,#47558,#47559,#47560,#47561,#47562,
#47563,#47564,#47565,#47566,#47567,#47568,#47569,#47570,#47571,#47572,#47573,
#47574,#47575,#47576,#47577,#47578,#47579,#47580,#47581,#47582,#47583,#47584,
#47585,#47586,#47587,#47588,#47589,#47590,#47591,#47592,#47593,#47594,#47595,
#47596,#47597,#47598,#47599,#47600,#47601,#47602,#47603,#47604,#47605,#47606,
#47607,#47608,#47609,#47610,#47611,#47612,#47613,#47614,#47615,#47616,#47617,
#47618,#47619,#47620,#47621,#47622,#47623,#47624,#47625,#47626,#47627,#47628,
#47629,#47630,#47631,#47632,#47633,#47634,#47635,#47636,#47637,#47638,#47639,
#47640,#47641,#47642,#47643,#47644,#47645,#47646,#47647,#47648,#47649,#47650,
#47651,#47652,#47653,#47654,#47655,#47656,#47657,#47658,#47659,#47660,#47661,
#47662,#47663,#47664,#47665,#47666,#47667,#47668),.UNSPECIFIED.,.F.,.F.,
(4,3,3,3,3,3,3,3,3,3,3,3,3,3,3,3,3,3,3,3,3,3,3,3,3,3,3,3,3,3,3,3,3,3,3,
3,3,3,3,3,3,3,3,3,3,3,3,3,3,3,3,3,3,3,3,3,3,3,3,3,3,3,3,3,3,3,3,3,3,3,3,
3,3,3,3,3,3,3,3,3,3,3,3,3,3,3,3,3,4),(13.6900193205037,13.7765255706091,
13.8633932766764,13.9506752568707,13.9965505591712,14.0710975762786,14.1455689584512,
14.2199785786351,14.2943402690552,14.3686678299873,14.4429750381826,14.5172909187391,
14.591616066856,14.6659629543546,14.7403440621851,14.8148113990801,14.8893280793008,
14.963947418968,14.9963041705405,15.0702098251051,15.1440284619494,15.2177745535932,
15.291462518635,15.3651067329712,15.4387215401563,15.5123334218691,15.5859473338826,
15.6595762406573,15.7332331132438,15.8069700911002,15.880751806945,15.9546350665569,
15.9960577819099,16.0706066884839,16.1450745481074,16.2194752868081,16.2938227862065,
16.3681308925289,16.4424134252073,16.5166969310457,16.5909849118941,16.6652898684778,
16.739624308151,16.8140380543639,16.8884971160856,16.9630531267513,16.9958113932792,
17.070360098545,17.144827784559,17.2192283772757,17.293575758261,17.3678837737038,
17.442166243016,17.516449726734,17.5907377111628,17.6650426970596,17.7393771918239,
17.8137910318318,17.8882502095728,17.9628063694821,17.9955650046486,18.0694442284512,
18.1432406348715,18.2169686795501,18.2906427675944,18.3642772645184,18.4378865063978,
18.5114990681443,18.5851175300349,18.658754858199,18.7324240275983,18.8061791702291,
18.8799823888292,18.9538922452339,18.9953186160179,19.0696902346647,19.143976089157,
19.2181903048216,19.2923469582718,19.3664600870775,19.4422813918206,19.516359529082,
19.5904390461399,19.6645326051933,19.7416570851506,19.8158504501171,19.8900876218651,
19.9644090480309,19.9730305250225),.UNSPECIFIED.);
#424=B_SPLINE_CURVE_WITH_KNOTS('',3,(#47670,#47671,#47672,#47673,#47674,
#47675,#47676,#47677,#47678,#47679,#47680,#47681,#47682,#47683,#47684,#47685,
#47686,#47687),.UNSPECIFIED.,.F.,.F.,(4,2,2,2,2,2,2,2,4),(19.973267472803,
20.8081215395782,21.643038451473,22.4779553633679,23.3128722752627,24.1477891871576,
24.9827060990525,25.8176230109473,26.2563899348629),.UNSPECIFIED.);
#425=B_SPLINE_CURVE_WITH_KNOTS('',3,(#47689,#47690,#47691,#47692,#47693,
#47694,#47695,#47696,#47697,#47698,#47699,#47700,#47701,#47702,#47703,#47704,
#47705,#47706),.UNSPECIFIED.,.F.,.F.,(4,2,2,2,2,2,2,2,4),(26.2563899348629,
27.0913068467578,27.9262237586526,28.7611406705475,29.5960575824423,30.4309744943372,
31.265891406232,32.1008083181269,32.5395752420425),.UNSPECIFIED.);
#426=B_SPLINE_CURVE_WITH_KNOTS('',3,(#47708,#47709,#47710,#47711,#47712,
#47713,#47714,#47715,#47716,#47717,#47718),.UNSPECIFIED.,.F.,.F.,(4,1,1,
1,1,1,1,1,4),(32.5395752420425,32.9918691751891,33.9916227865585,34.4914995922432,
34.9913763979279,35.9911300092972,36.9908836206666,37.990637232036,38.8223131615157),
 .UNSPECIFIED.);
#427=B_SPLINE_CURVE_WITH_KNOTS('',3,(#47720,#47721,#47722,#47723,#47724,
#47725,#47726,#47727,#47728,#47729,#47730,#47731,#47732,#47733,#47734,#47735,
#47736,#47737),.UNSPECIFIED.,.F.,.F.,(4,2,2,2,2,2,2,2,4),(38.8230221691357,
39.6576774611169,40.4925943730118,41.3275112849067,42.1624281968015,42.9973451086964,
43.8322620205912,44.6671789324861,45.105699052741),.UNSPECIFIED.);
#428=B_SPLINE_CURVE_WITH_KNOTS('',3,(#47739,#47740,#47741,#47742,#47743,
#47744,#47745,#47746,#47747,#47748,#47749),.UNSPECIFIED.,.F.,.F.,(4,1,1,
1,1,1,1,1,4),(45.1063437169403,45.9886661229909,46.9884197343603,47.9881733457296,
48.4880501514143,48.987926957099,49.9876805684683,50.9874341798377,51.3891311635813),
 .UNSPECIFIED.);
#429=B_SPLINE_CURVE_WITH_KNOTS('',3,(#47751,#47752,#47753,#47754,#47755,
#47756,#47757,#47758,#47759,#47760,#47761,#47762,#47763,#47764,#47765,#47766,
#47767,#47768),.UNSPECIFIED.,.F.,.F.,(4,2,2,2,2,2,2,2,4),(51.3891311635813,
52.2240480754761,53.058964987371,53.8938818992658,54.7287988111607,55.5637157230555,
56.3986326349504,57.2335495468452,57.6723164707609),.UNSPECIFIED.);
#430=B_SPLINE_CURVE_WITH_KNOTS('',3,(#47770,#47771,#47772,#47773,#47774,
#47775,#47776,#47777,#47778,#47779,#47780,#47781,#47782,#47783,#47784,#47785,
#47786,#47787),.UNSPECIFIED.,.F.,.F.,(4,2,2,2,2,2,2,2,4),(57.6723164707609,
58.5072333826557,59.3421502945506,60.1770672064454,61.0119841183403,61.8469010302351,
62.68181794213,63.5167348540249,63.9555017779405),.UNSPECIFIED.);
#431=B_SPLINE_CURVE_WITH_KNOTS('',3,(#47789,#47790,#47791,#47792,#47793,
#47794,#47795,#47796,#47797,#47798,#47799,#47800,#47801,#47802,#47803,#47804,
#47805,#47806),.UNSPECIFIED.,.F.,.F.,(4,2,2,2,2,2,2,2,4),(63.9555017779405,
64.7904186898353,65.6253356017302,66.4602525136251,67.29516942552,68.1300863374149,
68.9650032493097,69.7999201612046,70.23868708512),.UNSPECIFIED.);
#432=B_SPLINE_CURVE_WITH_KNOTS('',3,(#47808,#47809,#47810,#47811,#47812,
#47813,#47814,#47815,#47816,#47817,#47818,#47819,#47820,#47821,#47822,#47823,
#47824,#47825),.UNSPECIFIED.,.F.,.F.,(4,2,2,2,2,2,2,2,4),(70.23868708512,
71.0736039970149,71.9085209089098,72.7434378208046,73.5783547326995,74.4132716445944,
75.2481885564892,76.0831054683841,76.5218723922996),.UNSPECIFIED.);
#433=B_SPLINE_CURVE_WITH_KNOTS('',3,(#47827,#47828,#47829,#47830,#47831,
#47832,#47833,#47834,#47835,#47836),.UNSPECIFIED.,.F.,.F.,(4,1,1,1,1,1,
1,4),(76.5218723922996,76.9810280754412,77.9807816868106,78.98053529818,
79.9802889095494,80.9800425209187,81.9797961322881,82.8044636853364),
 .UNSPECIFIED.);
#434=B_SPLINE_CURVE_WITH_KNOTS('',3,(#47838,#47839,#47840,#47841,#47842,
#47843,#47844,#47845,#47846,#47847,#47848,#47849,#47850,#47851,#47852,#47853,
#47854,#47855),.UNSPECIFIED.,.F.,.F.,(4,2,2,2,2,2,2,2,4),(82.8052344214521,
83.6399746113741,84.474891523269,85.3098084351638,86.1447253470587,86.9796422589535,
87.8145591708484,88.6494760827433,89.088071555534),.UNSPECIFIED.);
#435=B_SPLINE_CURVE_WITH_KNOTS('',3,(#47857,#47858,#47859,#47860,#47861,
#47862,#47863,#47864,#47865,#47866,#47867,#47868,#47869,#47870,#47871,#47872,
#47873,#47874,#47875,#47876,#47877,#47878,#47879,#47880,#47881,#47882,#47883,
#47884,#47885,#47886,#47887,#47888,#47889,#47890,#47891,#47892,#47893,#47894,
#47895,#47896,#47897,#47898,#47899,#47900,#47901,#47902,#47903,#47904,#47905,
#47906,#47907,#47908,#47909,#47910,#47911,#47912,#47913,#47914,#47915,#47916,
#47917,#47918,#47919,#47920,#47921,#47922,#47923,#47924,#47925,#47926,#47927,
#47928,#47929,#47930,#47931,#47932,#47933,#47934,#47935,#47936,#47937,#47938,
#47939,#47940,#47941,#47942,#47943,#47944,#47945,#47946,#47947,#47948,#47949,
#47950,#47951,#47952,#47953,#47954,#47955,#47956,#47957,#47958,#47959,#47960,
#47961,#47962,#47963,#47964,#47965,#47966,#47967,#47968,#47969,#47970,#47971,
#47972,#47973,#47974,#47975,#47976,#47977,#47978,#47979,#47980,#47981,#47982,
#47983,#47984,#47985,#47986,#47987,#47988,#47989,#47990,#47991,#47992,#47993,
#47994,#47995,#47996,#47997,#47998,#47999,#48000,#48001,#48002,#48003,#48004,
#48005,#48006,#48007,#48008,#48009,#48010,#48011,#48012,#48013,#48014,#48015,
#48016,#48017,#48018,#48019,#48020,#48021,#48022,#48023,#48024,#48025,#48026,
#48027,#48028,#48029,#48030,#48031,#48032,#48033,#48034,#48035,#48036,#48037,
#48038,#48039,#48040,#48041,#48042,#48043,#48044,#48045,#48046,#48047,#48048,
#48049,#48050,#48051,#48052,#48053,#48054,#48055,#48056,#48057,#48058,#48059,
#48060,#48061,#48062,#48063,#48064,#48065,#48066,#48067,#48068,#48069,#48070,
#48071,#48072,#48073,#48074,#48075,#48076,#48077,#48078,#48079,#48080,#48081,
#48082,#48083,#48084,#48085,#48086,#48087,#48088,#48089,#48090,#48091,#48092,
#48093,#48094,#48095,#48096,#48097,#48098,#48099,#48100,#48101,#48102,#48103,
#48104,#48105,#48106,#48107,#48108,#48109,#48110,#48111,#48112,#48113,#48114,
#48115,#48116,#48117,#48118),.UNSPECIFIED.,.F.,.F.,(4,3,3,3,3,3,3,3,3,3,
3,3,3,3,3,3,3,3,3,3,3,3,3,3,3,3,3,3,3,3,3,3,3,3,3,3,3,3,3,3,3,3,3,3,3,3,
3,3,3,3,3,3,3,3,3,3,3,3,3,3,3,3,3,3,3,3,3,3,3,3,3,3,3,3,3,3,3,3,3,3,3,3,
3,3,3,3,3,4),(89.0885712435139,89.1619820578451,89.2353150691934,89.3085850276093,
89.3818066297448,89.456308928932,89.5294867054481,89.6026631980976,89.6758516412752,
89.7513449867672,89.8246300636465,89.9012275434448,89.977825023243,90.0561884454774,
90.1344550144504,90.2126300235391,90.2906873249174,90.3686726422253,90.4465682640788,
90.4777018289277,90.5556078870461,90.63358400619,90.7116353212181,90.7898165900036,
90.8680687618362,90.9464409348866,90.9775786346124,91.0521258301107,91.1265973938455,
91.2010071985689,91.2753690763153,91.3496968271721,91.4240042277022,91.4983203035823,
91.5726456488703,91.6469927352241,91.7213740434306,91.7958415820151,91.8703584649683,
91.9449780072942,91.9773322459818,92.0512378361067,92.1250564079675,92.1988024341337,
92.2724903332518,92.3461344812655,92.4197492217753,92.4933610364573,92.5669748812107,
92.6406037205372,92.7142605255286,92.7879974358707,92.8617790841371,92.93566227663,
92.9770858573511,93.0516347582909,93.1261026120739,93.2005033447333,93.2748508378962,
93.3491589377945,93.4234414638657,93.4977249628424,93.5720129366706,93.6463178860809,
93.7206523184315,93.7950660571295,93.8695251112157,93.9440811141211,93.9768394687205,
94.0513881942245,94.1258559007383,94.2002565141958,94.2746039161441,94.3489119527517,
94.4231944434118,94.4974779486874,94.5717659548025,94.6460709624977,94.7204054791555,
94.7948193410972,94.8692785408261,94.9438347226313,94.9765930800899,95.0589235913551,
95.1409198345418,95.2227089608825,95.3041468250003,95.3714283138384),
 .UNSPECIFIED.);
#436=B_SPLINE_CURVE_WITH_KNOTS('',3,(#48120,#48121,#48122,#48123,#48124,
#48125,#48126,#48127,#48128,#48129,#48130,#48131,#48132,#48133,#48134,#48135,
#48136,#48137),.UNSPECIFIED.,.F.,.F.,(4,2,2,2,2,2,2,2,4),(95.3714283138384,
96.2063452257333,97.0412621376282,97.876179049523,98.7110959614179,99.5460128733127,
100.380929785208,101.215846697102,101.654613621018),.UNSPECIFIED.);
#437=B_SPLINE_CURVE_WITH_KNOTS('',3,(#48139,#48140,#48141,#48142,#48143,
#48144,#48145,#48146,#48147,#48148,#48149,#48150,#48151,#48152,#48153,#48154,
#48155,#48156,#48157,#48158,#48159,#48160,#48161,#48162,#48163,#48164,#48165,
#48166,#48167,#48168,#48169,#48170,#48171,#48172,#48173,#48174,#48175,#48176,
#48177,#48178,#48179,#48180,#48181,#48182,#48183,#48184,#48185,#48186,#48187,
#48188,#48189,#48190,#48191,#48192,#48193,#48194,#48195,#48196,#48197,#48198,
#48199,#48200,#48201,#48202,#48203,#48204,#48205,#48206,#48207,#48208,#48209,
#48210,#48211,#48212,#48213,#48214,#48215,#48216,#48217,#48218,#48219,#48220,
#48221,#48222,#48223,#48224,#48225,#48226,#48227,#48228,#48229,#48230,#48231,
#48232,#48233,#48234,#48235,#48236,#48237,#48238,#48239,#48240,#48241,#48242,
#48243,#48244,#48245,#48246,#48247,#48248,#48249,#48250,#48251,#48252,#48253,
#48254,#48255,#48256,#48257,#48258,#48259,#48260,#48261,#48262,#48263,#48264,
#48265,#48266,#48267,#48268,#48269,#48270,#48271,#48272,#48273,#48274,#48275,
#48276,#48277,#48278,#48279,#48280,#48281,#48282,#48283,#48284,#48285,#48286,
#48287,#48288,#48289,#48290,#48291,#48292,#48293,#48294,#48295,#48296,#48297,
#48298,#48299,#48300,#48301,#48302,#48303,#48304,#48305,#48306,#48307,#48308,
#48309,#48310,#48311,#48312,#48313,#48314,#48315,#48316,#48317,#48318,#48319,
#48320,#48321,#48322,#48323,#48324,#48325,#48326,#48327,#48328,#48329,#48330,
#48331,#48332,#48333,#48334,#48335,#48336,#48337,#48338,#48339,#48340,#48341,
#48342,#48343,#48344,#48345,#48346,#48347,#48348,#48349,#48350,#48351,#48352,
#48353,#48354,#48355,#48356,#48357,#48358,#48359,#48360,#48361,#48362,#48363,
#48364,#48365,#48366,#48367,#48368,#48369,#48370,#48371,#48372,#48373,#48374,
#48375,#48376,#48377,#48378,#48379,#48380,#48381,#48382,#48383,#48384,#48385,
#48386,#48387,#48388,#48389,#48390,#48391,#48392,#48393,#48394,#48395,#48396,
#48397,#48398,#48399,#48400),.UNSPECIFIED.,.F.,.F.,(4,3,3,3,3,3,3,3,3,3,
3,3,3,3,3,3,3,3,3,3,3,3,3,3,3,3,3,3,3,3,3,3,3,3,3,3,3,3,3,3,3,3,3,3,3,3,
3,3,3,3,3,3,3,3,3,3,3,3,3,3,3,3,3,3,3,3,3,3,3,3,3,3,3,3,3,3,3,3,3,3,3,3,
3,3,3,3,3,4),(101.654613621018,101.743105911189,101.832203522192,101.922010479699,
101.974868359675,102.048747574089,102.122543971047,102.196272006199,102.269946084656,
102.343580571941,102.417189804136,102.490802356154,102.564420808288,102.638058126672,
102.711727286275,102.785482419128,102.859285627944,102.933195474639,102.974621971045,
103.049233451952,103.123758975888,103.198212451839,103.272607741207,103.346958666929,
103.42127902215,103.495592766087,103.569906252374,103.644231949046,103.718582328249,
103.793004671757,103.867468148569,103.942022108588,103.974375582414,104.052739004648,
104.131005573621,104.209180582708,104.287237884086,104.365223201394,104.443118823247,
104.474252388099,104.552158446218,104.630134565364,104.708185880393,104.786367149179,
104.864619321013,104.942991494064,104.974129193784,105.048676389282,105.123147953016,
105.19755775774,105.271919635486,105.346247386342,105.420554786872,105.494870862752,
105.56919620804,105.643543294394,105.7179246026,105.792392141185,105.866909024138,
105.941528566463,105.973882805153,106.047788395278,106.121606967139,106.195352993305,
106.269040892423,106.342685040436,106.416299780946,106.489911595628,106.563525440381,
106.637154279708,106.710811084699,106.784547995041,106.858329643307,106.9322128358,
106.973636416522,107.047773512522,107.121829677063,107.195819190245,107.269756285376,
107.343655159005,107.417923130154,107.491800560376,107.565684533812,107.639587867914,
107.714140632985,107.788154539542,107.86297673387,107.937798928198),
 .UNSPECIFIED.);
#438=B_SPLINE_CURVE_WITH_KNOTS('',3,(#48402,#48403,#48404,#48405,#48406,
#48407,#48408,#48409,#48410,#48411,#48412,#48413,#48414),.UNSPECIFIED.,
 .F.,.F.,(4,2,1,1,1,1,1,1,1,4),(107.937798928198,107.973390027892,108.973143639261,
109.97289725063,110.972650862,111.472527667684,111.972404473369,112.972158084738,
113.971911696108,114.220984235377),.UNSPECIFIED.);
#439=B_SPLINE_CURVE_WITH_KNOTS('',3,(#48416,#48417,#48418,#48419,#48420,
#48421,#48422,#48423,#48424,#48425,#48426,#48427,#48428,#48429,#48430,#48431,
#48432,#48433),.UNSPECIFIED.,.F.,.F.,(4,2,2,2,2,2,2,2,4),(114.220984235377,
115.055901147272,115.890818059167,116.725734971062,117.560651882957,118.395568794852,
119.230485706746,120.065402618641,120.504169542557),.UNSPECIFIED.);
#440=B_SPLINE_CURVE_WITH_KNOTS('',3,(#48435,#48436,#48437,#48438,#48439,
#48440,#48441,#48442,#48443,#48444,#48445,#48446,#48447,#48448,#48449,#48450,
#48451,#48452),.UNSPECIFIED.,.F.,.F.,(4,2,2,2,2,2,2,2,4),(120.504169542557,
121.339086454452,122.174003366346,123.008920278241,123.843837190136,124.678754102031,
125.513671013926,126.348587925821,126.787354849736),.UNSPECIFIED.);
#441=B_SPLINE_CURVE_WITH_KNOTS('',3,(#48454,#48455,#48456,#48457,#48458,
#48459,#48460,#48461,#48462,#48463,#48464,#48465,#48466,#48467,#48468,#48469,
#48470,#48471),.UNSPECIFIED.,.F.,.F.,(4,2,2,2,2,2,2,2,4),(126.787354849736,
127.622271761631,128.457188673526,129.292105585421,130.127022497316,130.961939409211,
131.796856321106,132.631773233001,133.070254297904),.UNSPECIFIED.);
#442=B_SPLINE_CURVE_WITH_KNOTS('',3,(#48473,#48474,#48475,#48476,#48477,
#48478,#48479,#48480,#48481,#48482,#48483,#48484,#48485,#48486,#48487,#48488,
#48489,#48490,#48491,#48492,#48493,#48494,#48495,#48496,#48497,#48498,#48499,
#48500,#48501,#48502,#48503,#48504,#48505,#48506,#48507,#48508,#48509,#48510,
#48511,#48512,#48513,#48514,#48515,#48516,#48517,#48518,#48519,#48520,#48521,
#48522,#48523,#48524,#48525,#48526,#48527,#48528,#48529,#48530,#48531,#48532,
#48533,#48534,#48535,#48536,#48537,#48538,#48539,#48540,#48541,#48542,#48543,
#48544,#48545,#48546,#48547,#48548,#48549,#48550,#48551,#48552,#48553,#48554,
#48555,#48556,#48557,#48558,#48559,#48560,#48561,#48562,#48563,#48564,#48565,
#48566,#48567,#48568,#48569,#48570,#48571,#48572,#48573,#48574,#48575,#48576,
#48577,#48578,#48579,#48580,#48581,#48582,#48583,#48584,#48585,#48586,#48587,
#48588,#48589,#48590,#48591,#48592,#48593,#48594,#48595,#48596,#48597,#48598,
#48599,#48600,#48601,#48602,#48603,#48604,#48605,#48606,#48607,#48608,#48609,
#48610,#48611,#48612,#48613,#48614,#48615,#48616,#48617,#48618,#48619,#48620,
#48621,#48622,#48623,#48624,#48625,#48626,#48627,#48628,#48629,#48630,#48631,
#48632,#48633,#48634,#48635,#48636,#48637,#48638,#48639,#48640,#48641,#48642,
#48643,#48644,#48645,#48646,#48647,#48648,#48649,#48650,#48651,#48652,#48653,
#48654,#48655,#48656,#48657,#48658,#48659,#48660,#48661,#48662,#48663,#48664,
#48665,#48666,#48667,#48668,#48669,#48670,#48671,#48672,#48673,#48674,#48675,
#48676,#48677,#48678,#48679,#48680,#48681,#48682,#48683,#48684,#48685,#48686,
#48687,#48688,#48689,#48690,#48691,#48692,#48693,#48694,#48695,#48696,#48697,
#48698,#48699,#48700,#48701,#48702,#48703,#48704,#48705,#48706,#48707,#48708,
#48709,#48710,#48711,#48712,#48713,#48714,#48715,#48716,#48717,#48718,#48719,
#48720,#48721,#48722,#48723,#48724,#48725,#48726,#48727,#48728,#48729,#48730,
#48731,#48732,#48733,#48734,#48735,#48736,#48737),.UNSPECIFIED.,.F.,.F.,
(4,3,3,3,3,3,3,3,3,3,3,3,3,3,3,3,3,3,3,3,3,3,3,3,3,3,3,3,3,3,3,3,3,3,3,
3,3,3,3,3,3,3,3,3,3,3,3,3,3,3,3,3,3,3,3,3,3,3,3,3,3,3,3,3,3,3,3,3,3,3,3,
3,3,3,3,3,3,3,3,3,3,3,3,3,3,3,3,3,4),(133.070847371309,133.144566118881,
133.218218486221,133.291818954969,133.365381967648,133.440582212129,133.51412749122,
133.587681041332,133.661255902816,133.737687907986,133.811382350179,133.885127816936,
133.958967914573,133.966983923495,134.04088951362,134.114708085481,134.188454111648,
134.262142010766,134.33578615878,134.40940089929,134.483012713973,134.556626558726,
134.630255398053,134.703912203045,134.777649113387,134.851430761653,134.925313954147,
134.966737534865,135.041286435805,135.115754289588,135.190155022248,135.264502515411,
135.338810615309,135.413093141381,135.487376640357,135.561664614186,135.635969563595,
135.710303995946,135.784717734645,135.859176788731,135.933732791636,135.966491146234,
136.041039871738,136.115507578251,136.189908191709,136.264255593657,136.338563630264,
136.412846120925,136.4871296262,136.561417632315,136.63572264001,136.710057156668,
136.784471018609,136.858930218338,136.933486400143,136.966244757603,137.040123972016,
137.113920368974,137.187648404125,137.261322482583,137.334956969868,137.408566202062,
137.48217875408,137.555797206213,137.629434524597,137.703103684199,137.776858817052,
137.850662025868,137.924571872562,137.965998368973,138.04060984988,138.115135373816,
138.189588849767,138.263984139136,138.338335064857,138.412655420078,138.486969164016,
138.561282650302,138.635608346975,138.709958726178,138.784381069686,138.858844546498,
138.933398506517,138.965751980342,139.048167245346,139.130346340956,139.212370217371,
139.294128390232,139.353725464096),.UNSPECIFIED.);
#443=B_SPLINE_CURVE_WITH_KNOTS('',3,(#48739,#48740,#48741,#48742,#48743,
#48744,#48745,#48746,#48747,#48748,#48749,#48750,#48751,#48752,#48753,#48754,
#48755,#48756),.UNSPECIFIED.,.F.,.F.,(4,2,2,2,2,2,2,2,4),(139.353725464096,
140.18864237599,141.023559287885,141.85847619978,142.693393111675,143.52831002357,
144.363226935464,145.198143847359,145.636910771275),.UNSPECIFIED.);
#444=B_SPLINE_CURVE_WITH_KNOTS('',3,(#48758,#48759,#48760,#48761,#48762,
#48763,#48764,#48765,#48766,#48767,#48768),.UNSPECIFIED.,.F.,.F.,(4,1,1,
1,1,1,1,1,4),(145.636910771275,145.964027259928,146.463904065612,146.963780871297,
147.963534482666,148.963288094036,149.963041705405,150.962795316774,151.919720738554),
 .UNSPECIFIED.);
#445=B_SPLINE_CURVE_WITH_KNOTS('',3,(#48770,#48771,#48772,#48773,#48774,
#48775,#48776,#48777,#48778,#48779,#48780,#48781,#48782,#48783,#48784,#48785,
#48786,#48787),.UNSPECIFIED.,.F.,.F.,(4,2,2,2,2,2,2,2,4),(151.920234954538,
152.75501299035,153.589929902244,154.424846814139,155.259763726034,156.094680637929,
156.929597549824,157.764514461719,158.203281385634),.UNSPECIFIED.);
#446=B_SPLINE_CURVE_WITH_KNOTS('',3,(#48789,#48790,#48791,#48792,#48793,
#48794,#48795,#48796,#48797,#48798,#48799,#48800,#48801,#48802,#48803,#48804,
#48805,#48806),.UNSPECIFIED.,.F.,.F.,(4,2,2,2,2,2,2,2,4),(158.203281385634,
159.038198297529,159.873115209424,160.708032121319,161.542949033214,162.377865945108,
163.212782857003,164.047699768898,164.486466692814),.UNSPECIFIED.);
#447=B_SPLINE_CURVE_WITH_KNOTS('',3,(#48808,#48809,#48810,#48811,#48812,
#48813,#48814,#48815,#48816,#48817,#48818),.UNSPECIFIED.,.F.,.F.,(4,1,1,
1,1,1,1,1,4),(164.486466692814,164.959345875946,165.959099487315,166.958853098684,
167.458729904369,167.958606710054,168.958360321423,169.958113932792,170.769651999993),
 .UNSPECIFIED.);
#448=B_SPLINE_CURVE_WITH_KNOTS('',3,(#48820,#48821,#48822,#48823,#48824,
#48825,#48826,#48827,#48828,#48829,#48830,#48831),.UNSPECIFIED.,.F.,.F.,
(4,1,1,1,1,1,1,1,1,4),(170.769651999993,170.957867544162,171.957621155531,
172.957374766901,173.95712837827,174.457005183955,174.956881989639,175.956635601009,
176.956389212378,177.052837307173),.UNSPECIFIED.);
#449=B_SPLINE_CURVE_WITH_KNOTS('',3,(#48833,#48834,#48835,#48836,#48837,
#48838,#48839,#48840,#48841,#48842,#48843,#48844,#48845,#48846,#48847,#48848,
#48849,#48850,#48851,#48852,#48853,#48854,#48855,#48856,#48857,#48858,#48859,
#48860,#48861,#48862,#48863,#48864,#48865,#48866,#48867,#48868,#48869,#48870,
#48871,#48872,#48873,#48874,#48875,#48876,#48877,#48878,#48879,#48880,#48881,
#48882,#48883,#48884,#48885,#48886,#48887,#48888,#48889,#48890,#48891,#48892,
#48893,#48894,#48895,#48896,#48897,#48898,#48899,#48900,#48901,#48902,#48903,
#48904,#48905,#48906,#48907,#48908,#48909,#48910,#48911,#48912,#48913,#48914,
#48915,#48916,#48917,#48918,#48919,#48920,#48921,#48922,#48923,#48924,#48925,
#48926,#48927,#48928,#48929,#48930,#48931,#48932,#48933,#48934,#48935,#48936,
#48937,#48938,#48939,#48940,#48941,#48942,#48943,#48944,#48945,#48946,#48947,
#48948,#48949,#48950,#48951,#48952,#48953,#48954,#48955,#48956,#48957,#48958,
#48959,#48960,#48961,#48962,#48963,#48964,#48965,#48966,#48967,#48968,#48969,
#48970,#48971,#48972,#48973,#48974,#48975,#48976,#48977,#48978,#48979,#48980,
#48981,#48982,#48983,#48984,#48985,#48986,#48987,#48988,#48989,#48990,#48991,
#48992,#48993,#48994,#48995,#48996,#48997,#48998,#48999,#49000,#49001,#49002,
#49003,#49004,#49005,#49006,#49007,#49008,#49009,#49010,#49011,#49012,#49013,
#49014,#49015,#49016,#49017,#49018,#49019,#49020,#49021,#49022,#49023,#49024,
#49025,#49026,#49027,#49028,#49029,#49030,#49031,#49032,#49033,#49034,#49035,
#49036,#49037,#49038,#49039,#49040,#49041,#49042,#49043,#49044,#49045,#49046,
#49047,#49048,#49049,#49050,#49051,#49052,#49053,#49054,#49055,#49056,#49057,
#49058,#49059,#49060,#49061,#49062,#49063,#49064,#49065,#49066,#49067,#49068,
#49069,#49070,#49071,#49072,#49073,#49074,#49075,#49076,#49077,#49078,#49079,
#49080,#49081,#49082,#49083,#49084,#49085,#49086,#49087,#49088,#49089,#49090,
#49091,#49092,#49093,#49094,#49095,#49096,#49097),.UNSPECIFIED.,.F.,.F.,
(4,3,3,3,3,3,3,3,3,3,3,3,3,3,3,3,3,3,3,3,3,3,3,3,3,3,3,3,3,3,3,3,3,3,3,
3,3,3,3,3,3,3,3,3,3,3,3,3,3,3,3,3,3,3,3,3,3,3,3,3,3,3,3,3,3,3,3,3,3,3,3,
3,3,3,3,3,3,3,3,3,3,3,3,3,3,3,3,3,4),(177.052837307173,177.126386915977,
177.199862112356,177.273277544079,177.346647810911,177.422834687515,177.496169099228,
177.569505281043,177.642856392112,177.716235599099,177.789691194626,177.863192111524,
177.936785246187,177.956142823747,178.030691549251,178.105159255765,178.179559869223,
178.253907271172,178.32821530778,178.40249779844,178.476781303716,178.551069309832,
178.625374317527,178.699708834184,178.774122696126,178.848581895855,178.923138077661,
178.955896435117,179.02977564953,179.103572046488,179.177300081639,179.250974160096,
179.324608647381,179.398217879575,179.471830431593,179.545448883726,179.61908620211,
179.692755361712,179.766510494565,179.840313703381,179.914223550075,179.955650046486,
180.030261527392,180.104787051329,180.17924052728,180.253635816648,180.32798674237,
180.402307097591,180.476620841528,180.550934327815,180.625260024487,180.699610403689,
180.774032747197,180.848496224009,180.923050184028,180.955403657855,181.03376708009,
181.112033649062,181.190208658151,181.268265959529,181.346251276837,181.424146898691,
181.45528046354,181.533186521659,181.611162640805,181.689213955835,181.767395224621,
181.845647396454,181.924019569505,181.955157269225,182.029704464723,182.104176028457,
182.17858583318,182.252947710927,182.327275461783,182.401582862314,182.475898938194,
182.550224283482,182.624571369835,182.698952678042,182.773420216626,182.847937099579,
182.922556641905,182.954910880594,183.038351025582,183.121389391934,183.204171436094,
183.286528896845,183.336022614352),.UNSPECIFIED.);
#450=B_SPLINE_CURVE_WITH_KNOTS('',3,(#49099,#49100,#49101,#49102,#49103,
#49104,#49105,#49106,#49107,#49108,#49109,#49110,#49111,#49112,#49113,#49114,
#49115,#49116),.UNSPECIFIED.,.F.,.F.,(4,2,2,2,2,2,2,2,4),(183.336022614352,
184.170939526247,185.005856438142,185.840773350037,186.675690261932,187.510607173827,
188.345524085721,189.180440997616,189.619207921532),.UNSPECIFIED.);
#451=B_SPLINE_CURVE_WITH_KNOTS('',3,(#49118,#49119,#49120,#49121,#49122,
#49123,#49124,#49125,#49126,#49127,#49128,#49129,#49130,#49131,#49132,#49133,
#49134,#49135,#49136,#49137,#49138,#49139,#49140,#49141,#49142,#49143,#49144,
#49145,#49146,#49147,#49148,#49149,#49150,#49151,#49152,#49153,#49154,#49155,
#49156,#49157,#49158,#49159,#49160,#49161,#49162,#49163,#49164,#49165,#49166,
#49167,#49168,#49169,#49170,#49171,#49172,#49173,#49174,#49175,#49176,#49177,
#49178,#49179,#49180,#49181,#49182,#49183,#49184,#49185,#49186,#49187,#49188,
#49189,#49190,#49191,#49192,#49193,#49194,#49195,#49196,#49197,#49198,#49199,
#49200,#49201,#49202,#49203,#49204,#49205,#49206,#49207,#49208,#49209,#49210,
#49211,#49212,#49213,#49214,#49215,#49216,#49217,#49218,#49219,#49220,#49221,
#49222,#49223,#49224,#49225,#49226,#49227,#49228,#49229,#49230,#49231,#49232,
#49233,#49234,#49235,#49236,#49237,#49238,#49239,#49240,#49241,#49242,#49243,
#49244,#49245,#49246,#49247,#49248,#49249,#49250,#49251,#49252,#49253,#49254,
#49255,#49256,#49257,#49258,#49259,#49260,#49261,#49262,#49263,#49264,#49265,
#49266,#49267,#49268,#49269,#49270,#49271,#49272,#49273,#49274,#49275,#49276,
#49277,#49278,#49279,#49280,#49281,#49282,#49283,#49284,#49285,#49286,#49287,
#49288,#49289,#49290,#49291,#49292,#49293,#49294,#49295,#49296,#49297,#49298,
#49299,#49300,#49301,#49302,#49303,#49304,#49305,#49306,#49307,#49308,#49309,
#49310,#49311,#49312,#49313,#49314,#49315,#49316,#49317,#49318,#49319,#49320,
#49321,#49322,#49323,#49324,#49325,#49326,#49327,#49328,#49329,#49330,#49331,
#49332,#49333,#49334,#49335,#49336,#49337,#49338,#49339,#49340,#49341,#49342,
#49343,#49344,#49345,#49346,#49347,#49348,#49349,#49350,#49351,#49352,#49353,
#49354,#49355,#49356,#49357,#49358,#49359,#49360,#49361,#49362,#49363,#49364,
#49365,#49366,#49367,#49368,#49369,#49370,#49371,#49372,#49373,#49374,#49375,
#49376,#49377,#49378,#49379),.UNSPECIFIED.,.F.,.F.,(4,3,3,3,3,3,3,3,3,3,
3,3,3,3,3,3,3,3,3,3,3,3,3,3,3,3,3,3,3,3,3,3,3,3,3,3,3,3,3,3,3,3,3,3,3,3,
3,3,3,3,3,3,3,3,3,3,3,3,3,3,3,3,3,3,3,3,3,3,3,3,3,3,3,3,3,3,3,3,3,3,3,3,
3,3,3,3,3,4),(189.619207921532,189.707929985649,189.797307795922,189.887481770886,
189.95318616018,190.027091750305,190.100910322165,190.174656348331,190.248344247449,
190.321988395462,190.395603135972,190.469214950654,190.542828795407,190.616457634733,
190.690114439724,190.763851350066,190.837632998332,190.911516190825,190.952939771549,
191.027488672489,191.101956526272,191.176357258931,191.250704752094,191.325012851992,
191.399295378063,191.47357887704,191.547866850868,191.622171800277,191.696506232628,
191.770919971326,191.845379025412,191.919935028318,191.952693382918,192.027242108422,
192.101709814936,192.176110428394,192.250457830343,192.324765866951,192.399048357611,
192.473331862887,192.547619869003,192.621924876698,192.696259393356,192.770673255297,
192.845132455027,192.919688636832,192.952446994288,193.026326208701,193.100122605659,
193.17385064081,193.247524719267,193.321159206551,193.394768438745,193.468380990763,
193.541999442896,193.61563676128,193.689305920882,193.763061053734,193.83686426255,
193.910774109244,193.952200605657,194.026812086564,194.1013376105,194.175791086452,
194.25018637582,194.324537301542,194.398857656763,194.473171400701,194.547484886987,
194.62181058366,194.696160962863,194.770583306371,194.845046783183,194.919600743203,
194.951954217027,195.030317639261,195.108584208233,195.186759217321,195.264816518699,
195.342801836007,195.42069745786,195.451831022711,195.527956948324,195.604128185549,
195.680403324837,195.756732301348,195.833183010997,195.902314075429),
 .UNSPECIFIED.);
#452=B_SPLINE_CURVE_WITH_KNOTS('',3,(#49381,#49382,#49383,#49384,#49385,
#49386,#49387,#49388,#49389,#49390,#49391,#49392,#49393,#49394,#49395,#49396,
#49397,#49398),.UNSPECIFIED.,.F.,.F.,(4,2,2,2,2,2,2,2,4),(195.902435354633,
196.737310140606,197.572227052501,198.407143964396,199.242060876291,200.076977788186,
200.911894700081,201.746811611976,202.185578535891),.UNSPECIFIED.);
#453=B_SPLINE_CURVE_WITH_KNOTS('',3,(#49400,#49401,#49402,#49403,#49404,
#49405,#49406,#49407,#49408,#49409,#49410,#49411,#49412,#49413,#49414,#49415,
#49416,#49417),.UNSPECIFIED.,.F.,.F.,(4,2,2,2,2,2,2,2,4),(202.185578535891,
203.020495447786,203.855412359681,204.690329271576,205.525246183471,206.360163095366,
207.19508000726,208.029996919155,208.468725328098),.UNSPECIFIED.);
#454=B_SPLINE_CURVE_WITH_KNOTS('',3,(#49419,#49420,#49421,#49422,#49423,
#49424,#49425,#49426,#49427,#49428,#49429,#49430,#49431,#49432,#49433,#49434,
#49435,#49436,#49437,#49438,#49439,#49440,#49441,#49442,#49443,#49444,#49445,
#49446,#49447,#49448,#49449,#49450,#49451,#49452,#49453,#49454,#49455,#49456,
#49457,#49458,#49459,#49460,#49461,#49462,#49463,#49464,#49465,#49466,#49467,
#49468,#49469,#49470,#49471,#49472,#49473,#49474,#49475,#49476,#49477,#49478,
#49479,#49480,#49481,#49482,#49483,#49484,#49485,#49486,#49487,#49488,#49489,
#49490,#49491,#49492,#49493,#49494,#49495,#49496,#49497,#49498,#49499,#49500,
#49501,#49502,#49503,#49504,#49505,#49506,#49507,#49508,#49509,#49510,#49511,
#49512,#49513,#49514,#49515,#49516,#49517,#49518,#49519,#49520,#49521,#49522,
#49523,#49524,#49525,#49526,#49527,#49528,#49529,#49530,#49531,#49532,#49533,
#49534,#49535,#49536,#49537,#49538,#49539,#49540,#49541,#49542,#49543,#49544,
#49545,#49546,#49547,#49548,#49549,#49550,#49551,#49552,#49553,#49554,#49555,
#49556,#49557,#49558,#49559,#49560,#49561,#49562,#49563,#49564,#49565,#49566,
#49567,#49568,#49569,#49570,#49571,#49572,#49573,#49574,#49575,#49576,#49577,
#49578,#49579,#49580,#49581,#49582,#49583,#49584,#49585,#49586,#49587,#49588,
#49589,#49590,#49591,#49592,#49593,#49594,#49595,#49596,#49597,#49598,#49599,
#49600,#49601,#49602,#49603,#49604,#49605,#49606,#49607,#49608,#49609,#49610,
#49611,#49612,#49613,#49614,#49615,#49616,#49617,#49618,#49619,#49620,#49621,
#49622,#49623,#49624,#49625,#49626,#49627,#49628,#49629,#49630,#49631,#49632,
#49633,#49634,#49635,#49636,#49637,#49638,#49639,#49640,#49641,#49642,#49643,
#49644,#49645,#49646,#49647,#49648,#49649,#49650,#49651,#49652,#49653,#49654,
#49655,#49656,#49657,#49658,#49659,#49660,#49661,#49662,#49663,#49664,#49665,
#49666,#49667,#49668,#49669,#49670,#49671,#49672,#49673,#49674,#49675,#49676,
#49677,#49678,#49679,#49680,#49681,#49682,#49683),.UNSPECIFIED.,.F.,.F.,
(4,3,3,3,3,3,3,3,3,3,3,3,3,3,3,3,3,3,3,3,3,3,3,3,3,3,3,3,3,3,3,3,3,3,3,
3,3,3,3,3,3,3,3,3,3,3,3,3,3,3,3,3,3,3,3,3,3,3,3,3,3,3,3,3,3,3,3,3,3,3,3,
3,3,3,3,3,3,3,3,3,3,3,3,3,3,3,3,3,4),(208.468825252627,208.546305652904,
208.623865211108,208.70502510238,208.78281664577,208.860690344446,208.938691508124,
208.948504776198,209.026868198431,209.105134767403,209.18330977649,209.261367077867,
209.339352395175,209.417248017027,209.448381581882,209.526287640001,209.604263759147,
209.682315074175,209.760496342961,209.838748514795,209.917120687846,209.948258387567,
210.022805583065,210.0972771468,210.171686951523,210.246048829269,210.320376580125,
210.394683980656,210.469000056536,210.543325401824,210.617672488177,210.692053796385,
210.766521334969,210.841038217922,210.915657760248,210.948011998936,211.021917589061,
211.095736160922,211.169482187088,211.243170086206,211.316814234219,211.390428974729,
211.464040789411,211.537654634165,211.611283473491,211.684940278482,211.758677188824,
211.83245883709,211.906342029583,211.947765610306,212.022314511246,212.096782365029,
212.171183097688,212.245530590852,212.31983869075,212.39412121682,212.468404715797,
212.542692689625,212.616997639035,212.691332071385,212.765745810084,212.84020486417,
212.914760867076,212.947519221675,213.02206794718,213.096535653694,213.170936267153,
213.245283669102,213.319591705711,213.393874196372,213.468157701649,213.542445707765,
213.61675071546,213.691085232118,213.76549909406,213.83995829379,213.914514475596,
213.947272833045,214.020064922963,214.092774329337,214.165416148347,214.238628258955,
214.311180237154,214.383713826874,214.45624252789,214.52996015422,214.602544126439,
214.676828579826,214.751113033212),.UNSPECIFIED.);
#455=B_SPLINE_CURVE_WITH_KNOTS('',3,(#49685,#49686,#49687,#49688,#49689,
#49690,#49691,#49692,#49693,#49694,#49695,#49696,#49697,#49698,#49699,#49700,
#49701,#49702),.UNSPECIFIED.,.F.,.F.,(4,2,2,2,2,2,2,2,4),(214.752284980915,
215.586866062145,216.42178297404,217.256699885935,218.091616797829,218.926533709724,
219.761450621619,220.596367533514,221.03492900151),.UNSPECIFIED.);
#456=B_SPLINE_CURVE_WITH_KNOTS('',3,(#49704,#49705,#49706,#49707,#49708,
#49709,#49710,#49711,#49712,#49713,#49714),.UNSPECIFIED.,.F.,.F.,(4,1,1,
1,1,1,1,1,4),(221.035575607579,221.945301723999,222.945055335369,223.444932141054,
223.944808946738,224.944562558108,225.944316169477,226.944069780846,227.31831244083),
 .UNSPECIFIED.);
#457=B_SPLINE_CURVE_WITH_KNOTS('',3,(#49716,#49717,#49718,#49719,#49720,
#49721,#49722,#49723,#49724,#49725,#49726,#49727,#49728,#49729,#49730,#49731,
#49732,#49733,#49734,#49735,#49736,#49737,#49738,#49739,#49740,#49741,#49742,
#49743,#49744,#49745,#49746,#49747,#49748,#49749,#49750,#49751,#49752,#49753,
#49754,#49755,#49756,#49757,#49758,#49759,#49760,#49761,#49762,#49763,#49764,
#49765,#49766,#49767,#49768,#49769,#49770,#49771,#49772,#49773,#49774,#49775,
#49776,#49777,#49778,#49779,#49780,#49781,#49782,#49783,#49784,#49785,#49786,
#49787,#49788,#49789,#49790,#49791,#49792,#49793,#49794,#49795,#49796,#49797,
#49798,#49799,#49800,#49801,#49802,#49803,#49804,#49805,#49806,#49807,#49808,
#49809,#49810,#49811,#49812,#49813,#49814,#49815,#49816,#49817,#49818,#49819,
#49820,#49821,#49822,#49823,#49824,#49825,#49826,#49827,#49828,#49829,#49830,
#49831,#49832,#49833,#49834,#49835,#49836,#49837,#49838,#49839,#49840,#49841,
#49842,#49843,#49844,#49845,#49846,#49847,#49848,#49849,#49850,#49851,#49852,
#49853,#49854,#49855,#49856,#49857,#49858,#49859,#49860,#49861,#49862,#49863,
#49864,#49865,#49866,#49867,#49868,#49869,#49870,#49871,#49872,#49873,#49874,
#49875,#49876,#49877,#49878,#49879,#49880,#49881,#49882,#49883,#49884,#49885,
#49886,#49887,#49888,#49889,#49890,#49891,#49892,#49893,#49894,#49895,#49896,
#49897,#49898,#49899,#49900,#49901,#49902,#49903,#49904,#49905,#49906,#49907,
#49908,#49909,#49910,#49911,#49912,#49913,#49914,#49915,#49916,#49917,#49918,
#49919,#49920,#49921,#49922,#49923,#49924,#49925,#49926,#49927,#49928,#49929,
#49930,#49931,#49932,#49933,#49934,#49935,#49936,#49937,#49938,#49939,#49940,
#49941,#49942,#49943,#49944,#49945,#49946,#49947,#49948,#49949,#49950,#49951,
#49952,#49953,#49954,#49955,#49956,#49957,#49958,#49959,#49960,#49961,#49962,
#49963,#49964,#49965,#49966,#49967,#49968,#49969,#49970,#49971,#49972,#49973,
#49974,#49975,#49976,#49977,#49978,#49979,#49980),.UNSPECIFIED.,.F.,.F.,
(4,3,3,3,3,3,3,3,3,3,3,3,3,3,3,3,3,3,3,3,3,3,3,3,3,3,3,3,3,3,3,3,3,3,3,
3,3,3,3,3,3,3,3,3,3,3,3,3,3,3,3,3,3,3,3,3,3,3,3,3,3,3,3,3,3,3,3,3,3,3,3,
3,3,3,3,3,3,3,3,3,3,3,3,3,3,3,3,3,4),(227.318319764609,227.39650771806,
227.471543782346,227.546599761227,227.621687259185,227.696817895653,227.77204346651,
227.847324610728,227.922710233808,227.943823392216,228.017702618196,228.091499026789,
228.165227073635,228.238901163838,228.312535662911,228.386144906928,228.459757470789,
228.533375934779,228.607013265027,228.680682436492,228.754437581151,228.828240801762,
228.902150660132,228.943577003585,229.018188418569,229.092713876678,229.167167286956,
229.241562510868,229.315913371408,229.390233661785,229.464547341577,229.538860764164,
229.613186397638,229.687536714199,229.761958996198,229.836422412068,229.91097631249,
229.943330614954,230.021694416695,230.099961360367,230.178136738113,230.256194396734,
230.334180063789,230.412076022717,230.443207420639,230.521112991988,230.599088615937,
230.677139428993,230.755320190006,230.833571851398,230.911943514346,230.943084226324,
231.017631417776,231.09210297716,231.166512777232,231.240874650033,231.315202395656,
231.389509790671,231.463825860633,231.538151199751,231.612498279687,231.686879581235,
231.761347112827,231.835863988587,231.91048352347,231.942837837693,232.016743903266,
232.090562951536,232.164309454742,232.237997831207,232.311642456557,232.385257674078,
232.45886996407,232.532484283145,232.606113595521,232.679770872006,232.753508249349,
232.827290362845,232.90117401393,232.942591449063,233.017415057715,233.09212234723,
233.166761385776,233.24134449427,233.315883961881,233.390394708471,233.464887403442,
233.539388711099,233.601505071789),.UNSPECIFIED.);
#458=B_SPLINE_CURVE_WITH_KNOTS('',3,(#49982,#49983,#49984,#49985,#49986,
#49987,#49988,#49989,#49990,#49991,#49992),.UNSPECIFIED.,.F.,.F.,(4,1,1,
1,1,1,1,1,4),(233.60151247774,233.942345060432,234.942098671801,235.941852283171,
236.94160589454,237.441482700225,237.941359505909,238.941113117279,239.884394119578),
 .UNSPECIFIED.);
#459=B_SPLINE_CURVE_WITH_KNOTS('',3,(#49994,#49995,#49996,#49997,#49998,
#49999,#50000,#50001,#50002,#50003,#50004,#50005,#50006,#50007,#50008,#50009,
#50010,#50011),.UNSPECIFIED.,.F.,.F.,(4,2,2,2,2,2,2,2,4),(239.884829668747,
240.719607290863,241.554524202758,242.389441114653,243.224358026548,244.059274938443,
244.894191850337,245.729108762232,246.167875686148),.UNSPECIFIED.);
#460=B_SPLINE_CURVE_WITH_KNOTS('',3,(#50013,#50014,#50015,#50016,#50017,
#50018,#50019,#50020,#50021,#50022,#50023,#50024,#50025,#50026,#50027,#50028,
#50029,#50030),.UNSPECIFIED.,.F.,.F.,(4,2,2,2,2,2,2,2,4),(246.167875686148,
247.002792598043,247.837709509938,248.672626421833,249.507543333728,250.342460245622,
251.177377157517,252.012294069412,252.451060993328),.UNSPECIFIED.);
#461=B_SPLINE_CURVE_WITH_KNOTS('',3,(#50032,#50033,#50034,#50035,#50036,
#50037,#50038,#50039,#50040,#50041,#50042),.UNSPECIFIED.,.F.,.F.,(4,1,1,
1,1,1,1,1,4),(252.451060993328,252.93766367645,253.937417287819,254.937170899189,
255.437047704873,255.936924510558,256.936678121927,257.936431733297,258.734246300507),
 .UNSPECIFIED.);
#462=B_SPLINE_CURVE_WITH_KNOTS('',3,(#50044,#50045,#50046,#50047,#50048,
#50049,#50050,#50051,#50052,#50053,#50054,#50055),.UNSPECIFIED.,.F.,.F.,
(4,1,1,1,1,1,1,1,1,4),(258.734246300507,258.936185344666,259.935938956035,
260.935692567405,261.935446178774,262.435322984459,262.935199790143,263.934953401513,
264.934707012882,265.017431607687),.UNSPECIFIED.);
#463=B_SPLINE_CURVE_WITH_KNOTS('',3,(#50057,#50058,#50059,#50060,#50061,
#50062,#50063,#50064,#50065,#50066,#50067,#50068,#50069,#50070,#50071,#50072,
#50073,#50074,#50075,#50076,#50077,#50078,#50079,#50080,#50081,#50082,#50083,
#50084,#50085,#50086,#50087,#50088,#50089,#50090,#50091,#50092,#50093,#50094,
#50095,#50096,#50097,#50098,#50099,#50100,#50101,#50102,#50103,#50104,#50105,
#50106,#50107,#50108,#50109,#50110,#50111,#50112,#50113,#50114,#50115,#50116,
#50117,#50118,#50119,#50120,#50121,#50122,#50123,#50124,#50125,#50126,#50127,
#50128,#50129,#50130,#50131,#50132,#50133,#50134,#50135,#50136,#50137,#50138,
#50139,#50140,#50141,#50142,#50143,#50144,#50145,#50146,#50147,#50148,#50149,
#50150,#50151,#50152,#50153,#50154,#50155,#50156,#50157,#50158,#50159,#50160,
#50161,#50162,#50163,#50164,#50165,#50166,#50167,#50168,#50169,#50170,#50171,
#50172,#50173,#50174,#50175,#50176,#50177,#50178,#50179,#50180,#50181,#50182,
#50183,#50184,#50185,#50186,#50187,#50188,#50189,#50190,#50191,#50192,#50193,
#50194,#50195,#50196,#50197,#50198,#50199,#50200,#50201,#50202,#50203,#50204,
#50205,#50206,#50207,#50208,#50209,#50210,#50211,#50212,#50213,#50214,#50215,
#50216,#50217,#50218,#50219,#50220,#50221,#50222,#50223,#50224,#50225,#50226,
#50227,#50228,#50229,#50230,#50231,#50232,#50233,#50234,#50235,#50236,#50237,
#50238,#50239,#50240,#50241,#50242,#50243,#50244,#50245,#50246,#50247,#50248,
#50249,#50250,#50251,#50252,#50253,#50254,#50255,#50256,#50257,#50258,#50259,
#50260,#50261,#50262,#50263,#50264,#50265,#50266,#50267,#50268,#50269,#50270,
#50271,#50272,#50273,#50274,#50275,#50276,#50277,#50278,#50279,#50280,#50281,
#50282,#50283,#50284,#50285,#50286,#50287,#50288,#50289,#50290,#50291,#50292,
#50293,#50294,#50295,#50296,#50297,#50298,#50299,#50300,#50301,#50302,#50303,
#50304,#50305,#50306,#50307,#50308,#50309,#50310,#50311,#50312,#50313,#50314,
#50315,#50316,#50317,#50318,#50319,#50320,#50321),.UNSPECIFIED.,.F.,.F.,
(4,3,3,3,3,3,3,3,3,3,3,3,3,3,3,3,3,3,3,3,3,3,3,3,3,3,3,3,3,3,3,3,3,3,3,
3,3,3,3,3,3,3,3,3,3,3,3,3,3,3,3,3,3,3,3,3,3,3,3,3,3,3,3,3,3,3,3,3,3,3,3,
3,3,3,3,3,3,3,3,3,3,3,3,3,3,3,3,3,4),(265.017431607687,265.091080802675,
265.164653880563,265.238165437093,265.311630019861,265.385062139806,265.458486881744,
265.531911102537,265.605347910285,265.678810418899,265.752348714647,265.825930080803,
265.899607635631,265.934460624252,266.009009349721,266.083477056199,266.15787766962,
266.232225071532,266.306533108104,266.380815598728,266.455099103966,266.529387110045,
266.603692117703,266.678026634324,266.752440496229,266.826899695921,266.90145587769,
266.934214235621,267.008093450029,267.081889846982,267.155617882127,267.229291960579,
267.302926447858,267.376535680046,267.450148232058,267.523766684185,267.597404002563,
267.671073162159,267.744828295005,267.818631503815,267.892541350503,267.93396784699,
268.008579327914,268.083104851867,268.157558327836,268.231953617221,268.306304542961,
268.380624898199,268.454938642154,268.529252128458,268.603577825149,268.677928204369,
268.752350547895,268.826814024724,268.901367984761,268.93372145836,269.012084880565,
269.090351449508,269.168526458566,269.246583759916,269.324569077196,269.402464699021,
269.433598264044,269.511504322176,269.589480441333,269.667531756376,269.745713025176,
269.823965197022,269.902337370087,269.933475069729,270.008022265226,270.08249382896,
270.156903633683,270.23126551143,270.305593262286,270.379900662817,270.454216738696,
270.528542083984,270.602889170337,270.677270478544,270.751738017127,270.82625490008,
270.900874442405,270.933228681098,271.017597248774,271.101519179819,271.185146260055,
271.268299188405,271.300616914866),.UNSPECIFIED.);
#464=B_SPLINE_CURVE_WITH_KNOTS('',3,(#50323,#50324,#50325,#50326,#50327,
#50328,#50329,#50330,#50331,#50332,#50333,#50334,#50335,#50336,#50337,#50338,
#50339,#50340),.UNSPECIFIED.,.F.,.F.,(4,2,2,2,2,2,2,2,4),(271.300616914866,
272.135533826761,272.970450738656,273.805367650551,274.640284562446,275.47520147434,
276.310118386235,277.14503529813,277.583802222046),.UNSPECIFIED.);
#465=B_SPLINE_CURVE_WITH_KNOTS('',3,(#50342,#50343,#50344,#50345,#50346,
#50347,#50348,#50349,#50350,#50351,#50352,#50353,#50354,#50355,#50356,#50357,
#50358,#50359,#50360,#50361,#50362,#50363,#50364,#50365,#50366,#50367,#50368,
#50369,#50370,#50371,#50372,#50373,#50374,#50375,#50376,#50377,#50378,#50379,
#50380,#50381,#50382,#50383,#50384,#50385,#50386,#50387,#50388,#50389,#50390,
#50391,#50392,#50393,#50394,#50395,#50396,#50397,#50398,#50399,#50400,#50401,
#50402,#50403,#50404,#50405,#50406,#50407,#50408,#50409,#50410,#50411,#50412,
#50413,#50414,#50415,#50416,#50417,#50418,#50419,#50420,#50421,#50422,#50423,
#50424,#50425,#50426,#50427,#50428,#50429,#50430,#50431,#50432,#50433,#50434,
#50435,#50436,#50437,#50438,#50439,#50440,#50441,#50442,#50443,#50444,#50445,
#50446,#50447,#50448,#50449,#50450,#50451,#50452,#50453,#50454,#50455,#50456,
#50457,#50458,#50459,#50460,#50461,#50462,#50463,#50464,#50465,#50466,#50467,
#50468,#50469,#50470,#50471,#50472,#50473,#50474,#50475,#50476,#50477,#50478,
#50479,#50480,#50481,#50482,#50483,#50484,#50485,#50486,#50487,#50488,#50489,
#50490,#50491,#50492,#50493,#50494,#50495,#50496,#50497,#50498,#50499,#50500,
#50501,#50502,#50503,#50504,#50505,#50506,#50507,#50508,#50509,#50510,#50511,
#50512,#50513,#50514,#50515,#50516,#50517,#50518,#50519,#50520,#50521,#50522,
#50523,#50524,#50525,#50526,#50527,#50528,#50529,#50530,#50531,#50532,#50533,
#50534,#50535,#50536,#50537,#50538,#50539,#50540,#50541,#50542,#50543,#50544,
#50545,#50546,#50547,#50548,#50549,#50550,#50551,#50552,#50553,#50554,#50555,
#50556,#50557,#50558,#50559,#50560,#50561,#50562,#50563,#50564,#50565,#50566,
#50567,#50568,#50569,#50570,#50571,#50572,#50573,#50574,#50575,#50576,#50577,
#50578,#50579,#50580,#50581,#50582,#50583,#50584,#50585,#50586,#50587,#50588,
#50589,#50590,#50591,#50592,#50593,#50594,#50595,#50596,#50597,#50598,#50599,
#50600,#50601,#50602,#50603),.UNSPECIFIED.,.F.,.F.,(4,3,3,3,3,3,3,3,3,3,
3,3,3,3,3,3,3,3,3,3,3,3,3,3,3,3,3,3,3,3,3,3,3,3,3,3,3,3,3,3,3,3,3,3,3,3,
3,3,3,3,3,3,3,3,3,3,3,3,3,3,3,3,3,3,3,3,3,3,3,3,3,3,3,3,3,3,3,3,3,3,3,3,
3,3,3,3,3,4),(277.583802222046,277.671324648983,277.759399580832,277.848188702518,
277.931503960684,278.005409550809,278.07922812267,278.152974148836,278.226662047954,
278.300306195967,278.373920936477,278.447532751159,278.521146595912,278.594775435239,
278.66843224023,278.742169150572,278.815950798838,278.889833991331,278.931257572053,
279.005806472993,279.080274326776,279.154675059436,279.229022552599,279.303330652497,
279.377613178569,279.451896677546,279.526184651374,279.600489600784,279.674824033135,
279.749237771833,279.82369682592,279.898252828826,279.931011183423,280.005559908927,
280.080027615441,280.154428228898,280.228775630846,280.303083667454,280.377366158114,
280.45164966339,280.525937669505,280.6002426772,280.674577193858,280.748991055799,
280.823450255528,280.898006437333,280.930764794792,281.004644009205,281.078440406163,
281.152168441314,281.225842519772,281.299477007056,281.37308623925,281.446698791268,
281.520317243401,281.593954561785,281.667623721387,281.74137885424,281.815182063056,
281.88909190975,281.930518406162,282.005129887069,282.079655411005,282.154108886956,
282.228504176325,282.302855102047,282.377175457268,282.451489201205,282.525802687492,
282.600128384164,282.674478763367,282.748901106875,282.823364583687,282.897918543707,
282.930272017531,283.008635439765,283.086902008738,283.165077017826,283.243134319204,
283.321119636513,283.399015258366,283.430148823216,283.505844145459,283.581580018405,
283.657412021233,283.73329529232,283.80929223256,283.866858317111),
 .UNSPECIFIED.);
#466=B_SPLINE_CURVE_WITH_KNOTS('',3,(#50605,#50606,#50607,#50608,#50609,
#50610,#50611,#50612,#50613,#50614,#50615,#50616,#50617,#50618,#50619,#50620,
#50621,#50622),.UNSPECIFIED.,.F.,.F.,(4,2,2,2,2,2,2,2,4),(283.86704461747,
284.70190444112,285.536821353015,286.37173826491,287.206655176805,288.0415720887,
288.876489000595,289.71140591249,290.150065821723),.UNSPECIFIED.);
#467=B_SPLINE_CURVE_WITH_KNOTS('',3,(#50624,#50625,#50626,#50627,#50628,
#50629,#50630,#50631,#50632,#50633,#50634),.UNSPECIFIED.,.F.,.F.,(4,1,1,
1,1,1,1,1,4),(290.150710098352,290.428424102801,290.928300908486,291.928054519855,
292.927808131225,293.927561742594,294.927315353963,295.927068965333,296.433358143585),
 .UNSPECIFIED.);
#468=B_SPLINE_CURVE_WITH_KNOTS('',3,(#50636,#50637,#50638,#50639,#50640,
#50641,#50642,#50643,#50644,#50645,#50646,#50647,#50648,#50649,#50650,#50651,
#50652,#50653,#50654,#50655,#50656,#50657,#50658,#50659,#50660,#50661,#50662,
#50663,#50664,#50665,#50666,#50667,#50668,#50669,#50670,#50671,#50672,#50673,
#50674,#50675,#50676,#50677,#50678,#50679,#50680,#50681,#50682,#50683,#50684,
#50685,#50686,#50687,#50688,#50689,#50690,#50691,#50692,#50693,#50694,#50695,
#50696,#50697,#50698,#50699,#50700,#50701,#50702,#50703,#50704,#50705,#50706,
#50707,#50708,#50709,#50710,#50711,#50712,#50713,#50714,#50715,#50716,#50717,
#50718,#50719,#50720,#50721,#50722,#50723,#50724,#50725,#50726,#50727,#50728,
#50729,#50730,#50731,#50732,#50733,#50734,#50735,#50736,#50737,#50738,#50739,
#50740,#50741,#50742,#50743,#50744,#50745,#50746,#50747,#50748,#50749,#50750,
#50751,#50752,#50753,#50754,#50755,#50756,#50757,#50758,#50759,#50760,#50761,
#50762,#50763,#50764,#50765,#50766,#50767,#50768,#50769,#50770,#50771,#50772,
#50773,#50774,#50775,#50776,#50777,#50778,#50779,#50780,#50781,#50782,#50783,
#50784,#50785,#50786,#50787,#50788,#50789,#50790,#50791,#50792,#50793,#50794,
#50795,#50796,#50797,#50798,#50799,#50800,#50801,#50802,#50803,#50804,#50805,
#50806,#50807,#50808,#50809,#50810,#50811,#50812,#50813,#50814,#50815,#50816,
#50817,#50818,#50819,#50820,#50821,#50822,#50823,#50824,#50825,#50826,#50827,
#50828,#50829,#50830,#50831,#50832,#50833,#50834,#50835,#50836,#50837,#50838,
#50839,#50840,#50841,#50842,#50843,#50844,#50845,#50846,#50847,#50848,#50849,
#50850,#50851,#50852,#50853,#50854,#50855,#50856,#50857,#50858,#50859,#50860,
#50861,#50862,#50863,#50864,#50865,#50866,#50867,#50868,#50869,#50870,#50871,
#50872,#50873,#50874,#50875,#50876),.UNSPECIFIED.,.F.,.F.,(4,3,3,3,3,3,
3,3,3,3,3,3,3,3,3,3,3,3,3,3,3,3,3,3,3,3,3,3,3,3,3,3,3,3,3,3,3,3,3,3,3,3,
3,3,3,3,3,3,3,3,3,3,3,3,3,3,3,3,3,3,3,3,3,3,3,3,3,3,3,3,3,3,3,3,3,3,3,3,
3,3,4),(296.433358143585,296.434193060497,296.523956293231,296.614011153268,
296.704010814826,296.793789611572,296.883272238627,296.926528890094,297.01529525035,
297.099635862482,297.167580580846,297.235456726032,297.268275055479,297.382618098477,
297.42642079471,297.541622636865,297.656981219889,297.77192883493,297.885910137167,
297.926022241522,298.037858647557,298.103191967374,298.182740066896,298.263144315382,
298.344595510271,298.394132693929,298.497551064862,298.604682910693,298.708091670656,
298.810098624463,298.908937059926,298.926078448187,298.938108879269,299.030135983696,
299.125844824944,299.222631746954,299.319787584731,299.355567335217,299.444448596844,
299.532532628507,299.619446836151,299.704089682706,299.773025791164,299.874821328605,
299.926497576467,300.029786969446,300.133648052168,300.238063752412,300.342340556559,
300.445603442629,300.517740448889,300.579586297339,300.607942703059,300.691865816354,
300.775475710615,300.858356472804,300.925694146258,301.00908707239,301.092604811342,
301.175646167532,301.189824156169,301.261772092477,301.334262910277,301.407337213651,
301.442859614954,301.526505427215,301.610283810116,301.69393111864,301.777377253097,
301.860593466713,301.925033158613,302.009335075365,302.093636992117,302.176114359061,
302.260572822167,302.277776526849,302.367060174878,302.45682417766,302.545782218094,
302.632284231065,302.716543450764),.UNSPECIFIED.);
#469=B_SPLINE_CURVE_WITH_KNOTS('',3,(#50878,#50879,#50880,#50881,#50882,
#50883,#50884,#50885,#50886,#50887,#50888,#50889,#50890,#50891,#50892,#50893,
#50894,#50895),.UNSPECIFIED.,.F.,.F.,(4,2,2,2,2,2,2,2,4),(302.716543450764,
303.551460362659,304.386377274554,305.221294186449,306.056211098343,306.891128010238,
307.726044922133,308.560961834028,308.999527974429),.UNSPECIFIED.);
#470=B_SPLINE_CURVE_WITH_KNOTS('',3,(#50897,#50898,#50899,#50900,#50901,
#50902,#50903,#50904,#50905,#50906,#50907),.UNSPECIFIED.,.F.,.F.,(4,1,1,
1,1,1,1,1,4),(309.000107393854,309.923619524504,310.923373135873,311.423249941558,
311.923126747242,312.922880358612,313.922633969981,314.922387581351,315.282906571436),
 .UNSPECIFIED.);
#471=B_SPLINE_CURVE_WITH_KNOTS('',3,(#50909,#50910,#50911,#50912,#50913,
#50914,#50915,#50916,#50917,#50918,#50919,#50920,#50921,#50922,#50923,#50924,
#50925,#50926,#50927,#50928,#50929,#50930,#50931,#50932,#50933,#50934,#50935,
#50936,#50937,#50938,#50939,#50940,#50941,#50942,#50943,#50944,#50945,#50946,
#50947,#50948,#50949,#50950,#50951,#50952,#50953,#50954,#50955,#50956,#50957,
#50958,#50959,#50960,#50961,#50962,#50963,#50964,#50965,#50966,#50967,#50968,
#50969,#50970,#50971,#50972,#50973,#50974,#50975,#50976,#50977,#50978,#50979,
#50980,#50981,#50982,#50983,#50984,#50985,#50986,#50987,#50988,#50989,#50990,
#50991,#50992,#50993,#50994,#50995,#50996,#50997,#50998,#50999,#51000,#51001,
#51002,#51003,#51004,#51005,#51006,#51007,#51008,#51009,#51010,#51011,#51012,
#51013,#51014,#51015,#51016,#51017,#51018,#51019,#51020,#51021,#51022,#51023,
#51024,#51025,#51026,#51027,#51028,#51029,#51030,#51031,#51032,#51033,#51034,
#51035,#51036,#51037,#51038,#51039,#51040,#51041,#51042,#51043,#51044,#51045,
#51046,#51047,#51048,#51049,#51050,#51051,#51052,#51053,#51054,#51055,#51056,
#51057,#51058,#51059,#51060,#51061,#51062,#51063,#51064,#51065,#51066,#51067,
#51068,#51069,#51070,#51071,#51072,#51073,#51074,#51075,#51076,#51077,#51078,
#51079,#51080,#51081,#51082,#51083,#51084,#51085,#51086,#51087,#51088,#51089,
#51090,#51091,#51092,#51093,#51094,#51095,#51096,#51097,#51098,#51099,#51100,
#51101,#51102,#51103,#51104,#51105,#51106,#51107,#51108,#51109,#51110,#51111,
#51112,#51113,#51114,#51115,#51116,#51117,#51118,#51119,#51120,#51121,#51122,
#51123,#51124,#51125,#51126,#51127,#51128,#51129,#51130,#51131,#51132,#51133,
#51134,#51135,#51136,#51137,#51138,#51139,#51140,#51141,#51142,#51143,#51144,
#51145,#51146,#51147,#51148,#51149,#51150,#51151,#51152,#51153,#51154,#51155,
#51156,#51157,#51158,#51159,#51160,#51161,#51162,#51163,#51164,#51165,#51166,
#51167,#51168,#51169,#51170,#51171,#51172,#51173),.UNSPECIFIED.,.F.,.F.,
(4,3,3,3,3,3,3,3,3,3,3,3,3,3,3,3,3,3,3,3,3,3,3,3,3,3,3,3,3,3,3,3,3,3,3,
3,3,3,3,3,3,3,3,3,3,3,3,3,3,3,3,3,3,3,3,3,3,3,3,3,3,3,3,3,3,3,3,3,3,3,3,
3,3,3,3,3,3,3,3,3,3,3,3,3,3,3,3,3,4),(315.282914065123,315.357699868323,
315.432502268467,315.507318293193,315.582159837218,315.657038806598,315.73200888131,
315.807030003138,315.882158767803,315.92214119272,315.996020407133,316.069816804091,
316.143544839241,316.217218917699,316.290853404983,316.364462637177,316.438075189195,
316.511693641327,316.585330959711,316.659000119313,316.732755252165,316.806558460981,
316.880468307675,316.921894804089,316.996506284996,317.071031808932,317.145485284884,
317.219880574253,317.294231499975,317.368551855196,317.442865599134,317.517179085421,
317.591504782093,317.665855161296,317.740277504804,317.814740981616,317.889294941636,
317.921648415459,318.000011837693,318.078278406666,318.156453415754,318.234510717131,
318.31249603444,318.390391656292,318.421525221143,318.499431279262,318.577407398407,
318.655458713436,318.733639982222,318.811892154054,318.890264327105,318.921402026828,
318.995949222326,319.070420786061,319.144830590784,319.21919246853,319.293520219386,
319.367827619918,319.442143695798,319.516469041086,319.590816127439,319.665197435647,
319.739664974231,319.814181857185,319.88880139951,319.921155638197,319.995061228322,
320.068879800183,320.142625826349,320.216313725467,320.289957873481,320.363572613991,
320.437184428674,320.510798273427,320.584427112754,320.658083917746,320.731820828088,
320.805602476354,320.879485668847,320.920909249567,320.995954235749,321.070880525398,
321.145736706182,321.220534877864,321.295287107226,321.370005534557,321.44470364888,
321.51940290023,321.566099372303),.UNSPECIFIED.);
#472=B_SPLINE_CURVE_WITH_KNOTS('',3,(#51175,#51176,#51177,#51178,#51179,
#51180,#51181,#51182,#51183,#51184,#51185),.UNSPECIFIED.,.F.,.F.,(4,1,1,
1,1,1,1,1,4),(321.566106881173,321.920662860936,322.920416472305,323.920170083675,
324.919923695044,325.419800500729,325.919677306414,326.919430917783,327.848964379533),
 .UNSPECIFIED.);
#473=B_SPLINE_CURVE_WITH_KNOTS('',3,(#51187,#51188,#51189,#51190,#51191,
#51192,#51193,#51194,#51195,#51196,#51197,#51198,#51199,#51200,#51201,#51202,
#51203,#51204),.UNSPECIFIED.,.F.,.F.,(4,2,2,2,2,2,2,2,4),(327.849512828964,
328.684201591377,329.519118503272,330.354035415167,331.188952327061,332.023869238956,
332.858786150851,333.693703062746,334.132469986662),.UNSPECIFIED.);
#474=B_SPLINE_CURVE_WITH_KNOTS('',3,(#51206,#51207,#51208,#51209,#51210,
#51211,#51212,#51213,#51214,#51215,#51216,#51217,#51218,#51219,#51220,#51221,
#51222,#51223),.UNSPECIFIED.,.F.,.F.,(4,2,2,2,2,2,2,2,4),(334.132469986662,
334.967386898557,335.802303810452,336.637220722347,337.472137634242,338.307054546136,
339.141971458031,339.976888369926,340.415655293842),.UNSPECIFIED.);
#475=B_SPLINE_CURVE_WITH_KNOTS('',3,(#51225,#51226,#51227,#51228,#51229,
#51230,#51231,#51232,#51233,#51234,#51235,#51236,#51237,#51238,#51239,#51240,
#51241,#51242,#51243,#51244,#51245,#51246,#51247,#51248,#51249,#51250,#51251,
#51252,#51253,#51254,#51255,#51256,#51257,#51258,#51259,#51260,#51261,#51262,
#51263,#51264,#51265,#51266,#51267,#51268,#51269,#51270,#51271,#51272,#51273,
#51274,#51275,#51276,#51277,#51278,#51279,#51280,#51281,#51282,#51283,#51284,
#51285,#51286,#51287,#51288,#51289,#51290,#51291,#51292,#51293,#51294,#51295,
#51296,#51297,#51298,#51299,#51300,#51301,#51302,#51303,#51304,#51305,#51306,
#51307,#51308,#51309,#51310,#51311,#51312,#51313,#51314,#51315,#51316,#51317,
#51318,#51319,#51320,#51321,#51322,#51323,#51324,#51325,#51326,#51327,#51328,
#51329,#51330,#51331,#51332,#51333,#51334,#51335,#51336,#51337,#51338,#51339,
#51340,#51341,#51342,#51343,#51344,#51345,#51346,#51347,#51348,#51349,#51350,
#51351,#51352,#51353,#51354,#51355,#51356,#51357,#51358,#51359,#51360,#51361,
#51362,#51363,#51364,#51365,#51366,#51367,#51368,#51369,#51370,#51371,#51372,
#51373,#51374,#51375,#51376,#51377,#51378,#51379,#51380,#51381,#51382,#51383,
#51384,#51385,#51386,#51387,#51388,#51389,#51390,#51391,#51392,#51393,#51394,
#51395,#51396,#51397,#51398,#51399,#51400,#51401,#51402,#51403,#51404,#51405,
#51406,#51407,#51408,#51409,#51410,#51411,#51412,#51413,#51414,#51415,#51416,
#51417,#51418,#51419,#51420,#51421,#51422,#51423,#51424,#51425,#51426,#51427,
#51428,#51429,#51430,#51431,#51432,#51433,#51434,#51435,#51436,#51437,#51438,
#51439,#51440,#51441,#51442,#51443,#51444,#51445,#51446,#51447,#51448,#51449,
#51450,#51451,#51452,#51453,#51454,#51455,#51456,#51457,#51458,#51459,#51460,
#51461,#51462,#51463,#51464,#51465,#51466,#51467,#51468,#51469,#51470,#51471,
#51472,#51473,#51474,#51475,#51476,#51477,#51478,#51479,#51480,#51481,#51482,
#51483,#51484,#51485,#51486,#51487,#51488,#51489),.UNSPECIFIED.,.F.,.F.,
(4,3,3,3,3,3,3,3,3,3,3,3,3,3,3,3,3,3,3,3,3,3,3,3,3,3,3,3,3,3,3,3,3,3,3,
3,3,3,3,3,3,3,3,3,3,3,3,3,3,3,3,3,3,3,3,3,3,3,3,3,3,3,3,3,3,3,3,3,3,3,3,
3,3,3,3,3,3,3,3,3,3,3,3,3,3,3,3,3,4),(340.415655293842,340.494481417605,
340.573436456946,340.65252149617,340.731807374889,340.81120335182,340.890766323486,
340.915981476954,340.989887067079,341.063705638941,341.137451665107,341.211139564226,
341.284783712239,341.35839845275,341.432010267432,341.505624112186,341.579252951513,
341.652909756505,341.726646666847,341.800428315114,341.874311507607,341.915735088324,
341.990283989264,342.064751843047,342.139152575706,342.213500068869,342.287808168767,
342.362090694839,342.436374193815,342.510662167644,342.584967117054,342.659301549404,
342.733715288102,342.808174342189,342.882730345094,342.915488699693,342.990037425197,
343.06450513171,343.138905745168,343.213253147116,343.287561183724,343.361843674384,
343.436127179659,343.510415185774,343.584720193469,343.659054710126,343.733468572068,
343.807927771797,343.882483953602,343.915242311062,343.989121525475,344.062917922434,
344.136645957585,344.210320036042,344.283954523327,344.357563755521,344.431176307539,
344.504794759672,344.578432078057,344.652101237659,344.725856370512,344.799659579328,
344.873569426022,344.914995922432,344.989607403339,345.064132927275,345.138586403226,
345.212981692595,345.287332618317,345.361652973537,345.435966717475,345.510280203761,
345.584605900434,345.658956279637,345.733378623144,345.807842099956,345.882396059976,
345.914749533801,345.993112956036,346.071379525009,346.149554534097,346.227611835475,
346.305597152784,346.383492774638,346.414626339486,346.486996405416,346.559377940755,
346.631822367735,346.698290813016),.UNSPECIFIED.);
#476=B_SPLINE_CURVE_WITH_KNOTS('',3,(#51491,#51492,#51493,#51494,#51495,
#51496,#51497,#51498,#51499,#51500,#51501,#51502,#51503,#51504,#51505,#51506,
#51507,#51508),.UNSPECIFIED.,.F.,.F.,(4,2,2,2,2,2,2,2,4),(346.698927745726,
347.533757512916,348.368674424811,349.203591336705,350.0385082486,350.873425160495,
351.70834207239,352.543258984284,352.981965591049),.UNSPECIFIED.);
#477=B_SPLINE_CURVE_WITH_KNOTS('',3,(#51510,#51511,#51512,#51513,#51514,
#51515,#51516,#51517,#51518,#51519,#51520,#51521,#51522,#51523,#51524,#51525,
#51526,#51527,#51528,#51529,#51530,#51531,#51532,#51533,#51534,#51535,#51536,
#51537,#51538,#51539,#51540,#51541,#51542,#51543,#51544,#51545,#51546,#51547,
#51548,#51549,#51550,#51551,#51552,#51553,#51554,#51555,#51556,#51557,#51558,
#51559,#51560,#51561,#51562,#51563,#51564,#51565,#51566,#51567,#51568,#51569,
#51570,#51571,#51572,#51573,#51574,#51575,#51576,#51577,#51578,#51579,#51580,
#51581,#51582,#51583,#51584,#51585,#51586,#51587,#51588,#51589,#51590,#51591,
#51592,#51593,#51594,#51595,#51596,#51597,#51598,#51599,#51600,#51601,#51602,
#51603,#51604,#51605,#51606,#51607,#51608,#51609,#51610,#51611,#51612,#51613,
#51614,#51615,#51616,#51617,#51618,#51619,#51620,#51621,#51622,#51623,#51624,
#51625,#51626,#51627,#51628,#51629,#51630,#51631,#51632,#51633,#51634,#51635,
#51636,#51637,#51638,#51639,#51640,#51641,#51642,#51643,#51644,#51645,#51646,
#51647,#51648,#51649,#51650,#51651,#51652,#51653,#51654,#51655,#51656,#51657,
#51658,#51659,#51660,#51661,#51662,#51663,#51664,#51665,#51666,#51667,#51668,
#51669,#51670,#51671,#51672,#51673,#51674,#51675,#51676,#51677,#51678,#51679,
#51680,#51681,#51682,#51683,#51684,#51685,#51686,#51687,#51688,#51689,#51690,
#51691,#51692,#51693,#51694,#51695,#51696,#51697,#51698,#51699,#51700,#51701,
#51702,#51703,#51704,#51705,#51706,#51707,#51708,#51709,#51710,#51711,#51712,
#51713,#51714,#51715,#51716,#51717,#51718,#51719,#51720,#51721,#51722,#51723,
#51724,#51725,#51726,#51727,#51728,#51729,#51730,#51731,#51732,#51733,#51734,
#51735,#51736,#51737,#51738,#51739,#51740,#51741,#51742,#51743,#51744,#51745,
#51746,#51747,#51748,#51749,#51750,#51751,#51752,#51753,#51754,#51755,#51756,
#51757,#51758,#51759,#51760,#51761,#51762,#51763,#51764,#51765,#51766,#51767,
#51768,#51769,#51770,#51771),.UNSPECIFIED.,.F.,.F.,(4,3,3,3,3,3,3,3,3,3,
3,3,3,3,3,3,3,3,3,3,3,3,3,3,3,3,3,3,3,3,3,3,3,3,3,3,3,3,3,3,3,3,3,3,3,3,
3,3,3,3,3,3,3,3,3,3,3,3,3,3,3,3,3,3,3,3,3,3,3,3,3,3,3,3,3,3,3,3,3,3,3,3,
3,3,3,3,3,4),(352.982179302569,353.057997125252,353.133729911659,353.209366840018,
353.284948102799,353.360473781065,353.412901619071,353.490807677191,353.568783796336,
353.646835111366,353.725016380152,353.803268551986,353.881640725038,353.912778424756,
353.987325620254,354.061797183988,354.136206988712,354.210568866458,354.284896617314,
354.359204017844,354.433520093724,354.507845439012,354.582192525365,354.656573833573,
354.731041372157,354.80555825511,354.880177797435,354.912532036125,354.98643762625,
355.060256198111,355.134002224277,355.207690123395,355.281334271409,355.354949011919,
355.428560826601,355.502174671355,355.575803510682,355.649460315673,355.723197226015,
355.796978874282,355.870862066775,355.912285647495,355.986834548435,356.061302402218,
356.135703134878,356.210050628041,356.284358727939,356.358641254011,356.432924752988,
356.507212726816,356.581517676226,356.655852108576,356.730265847275,356.804724901361,
356.879280904267,356.912039258864,356.986587984368,357.061055690881,357.135456304339,
357.209803706287,357.284111742895,357.358394233555,357.43267773883,357.506965744945,
357.58127075264,357.655605269297,357.730019131239,357.804478330968,357.879034512773,
357.911792870233,357.985672084646,358.059468481605,358.133196516756,358.206870595213,
358.280505082497,358.354114314692,358.427726866709,358.501345318843,358.574982637227,
358.64865179683,358.722406929682,358.796210138499,358.870119985193,358.911546481603,
358.999962665047,359.087819325262,359.176515270321,359.26521121538),
 .UNSPECIFIED.);
#478=B_SPLINE_CURVE_WITH_KNOTS('',3,(#51773,#51774,#51775,#51776,#51777,
#51778,#51779,#51780,#51781,#51782,#51783,#51784,#51785,#51786,#51787,#51788,
#51789,#51790),.UNSPECIFIED.,.F.,.F.,(4,2,2,2,2,2,2,2,4),(359.26521121538,
360.100128127275,360.93504503917,361.769961951065,362.60487886296,363.439795774855,
364.27471268675,365.109629598645,365.54839652256),.UNSPECIFIED.);
#479=B_SPLINE_CURVE_WITH_KNOTS('',3,(#51792,#51793,#51794,#51795,#51796,
#51797,#51798,#51799,#51800,#51801,#51802,#51803,#51804,#51805,#51806,#51807,
#51808,#51809,#51810,#51811,#51812,#51813,#51814,#51815,#51816,#51817,#51818,
#51819,#51820,#51821,#51822,#51823,#51824,#51825,#51826,#51827,#51828,#51829,
#51830,#51831,#51832,#51833,#51834,#51835,#51836,#51837,#51838,#51839,#51840,
#51841,#51842,#51843,#51844,#51845,#51846,#51847,#51848,#51849,#51850,#51851,
#51852,#51853,#51854,#51855,#51856,#51857,#51858,#51859,#51860,#51861,#51862,
#51863,#51864,#51865,#51866,#51867,#51868,#51869,#51870,#51871,#51872,#51873,
#51874,#51875,#51876,#51877,#51878,#51879,#51880,#51881,#51882,#51883,#51884,
#51885,#51886,#51887,#51888,#51889,#51890,#51891,#51892,#51893,#51894,#51895,
#51896,#51897,#51898,#51899,#51900,#51901,#51902,#51903,#51904,#51905,#51906,
#51907,#51908,#51909,#51910,#51911,#51912,#51913,#51914,#51915,#51916,#51917,
#51918,#51919,#51920,#51921,#51922,#51923,#51924,#51925,#51926,#51927,#51928,
#51929,#51930,#51931,#51932,#51933,#51934,#51935,#51936,#51937,#51938,#51939,
#51940,#51941,#51942,#51943,#51944,#51945,#51946,#51947,#51948,#51949,#51950,
#51951,#51952,#51953,#51954,#51955,#51956,#51957,#51958,#51959,#51960,#51961,
#51962,#51963,#51964,#51965,#51966,#51967,#51968,#51969,#51970,#51971,#51972,
#51973,#51974,#51975,#51976,#51977,#51978,#51979,#51980,#51981,#51982,#51983,
#51984,#51985,#51986,#51987,#51988,#51989,#51990,#51991,#51992,#51993,#51994,
#51995,#51996,#51997,#51998,#51999,#52000,#52001,#52002,#52003,#52004,#52005,
#52006,#52007,#52008,#52009,#52010,#52011,#52012,#52013,#52014,#52015,#52016,
#52017,#52018,#52019,#52020,#52021,#52022,#52023,#52024,#52025,#52026,#52027,
#52028,#52029,#52030,#52031,#52032,#52033,#52034,#52035,#52036,#52037,#52038,
#52039,#52040,#52041,#52042,#52043,#52044,#52045,#52046,#52047,#52048,#52049,
#52050,#52051,#52052,#52053,#52054,#52055,#52056),.UNSPECIFIED.,.F.,.F.,
(4,3,3,3,3,3,3,3,3,3,3,3,3,3,3,3,3,3,3,3,3,3,3,3,3,3,3,3,3,3,3,3,3,3,3,
3,3,3,3,3,3,3,3,3,3,3,3,3,3,3,3,3,3,3,3,3,3,3,3,3,3,3,3,3,3,3,3,3,3,3,3,
3,3,3,3,3,3,3,3,3,3,3,3,3,3,3,3,3,4),(365.54839652256,365.631859157807,
365.715917223977,365.800285132278,365.885043684889,365.909821761188,365.984433242095,
366.058958766032,366.133412241984,366.207807531353,366.282158457075,366.356478812296,
366.430792556234,366.505106042521,366.579431739194,366.653782118398,366.728204461906,
366.802667938719,366.877221898739,366.909575372558,366.987938794792,367.066205363764,
367.144380372852,367.222437674229,367.300422991537,367.37831861339,367.409452178242,
367.487358236361,367.565334355506,367.643385670535,367.72156693932,367.799819111153,
367.878191284204,367.909328983927,367.983876179425,368.05834774316,368.132757547883,
368.207119425629,368.281447176486,368.355754577016,368.430070652896,368.504395998184,
368.578743084538,368.653124392745,368.727591931329,368.802108814283,368.876728356608,
368.909082595296,368.982988185421,369.056806757282,369.130552783448,369.204240682566,
369.27788483058,369.35149957109,369.425111385772,369.498725230526,369.572354069853,
369.646010874844,369.719747785186,369.793529433453,369.867412625946,369.908836206666,
369.983385107606,370.057852961389,370.132253694048,370.206601187211,370.28090928711,
370.355191813181,370.429475312158,370.503763285986,370.578068235396,370.652402667747,
370.726816406445,370.801275460532,370.875831463437,370.908589818035,370.982308882286,
371.055947327308,371.129519736888,371.203040643532,371.276524540064,371.349994411399,
371.423459498714,371.496932884262,371.570427653428,371.643992705792,371.717597033695,
371.791294373935,371.831581829739),.UNSPECIFIED.);
#480=B_SPLINE_CURVE_WITH_KNOTS('',3,(#52058,#52059,#52060,#52061,#52062,
#52063,#52064,#52065,#52066,#52067,#52068,#52069,#52070),.UNSPECIFIED.,
 .F.,.F.,(4,2,1,1,1,1,1,1,1,4),(371.831581829739,371.908343429405,372.908097040774,
373.907850652143,374.407727457828,374.907604263513,375.907357874882,376.907111486251,
377.906865097621,378.114767136919),.UNSPECIFIED.);
#481=B_SPLINE_CURVE_WITH_KNOTS('',3,(#52072,#52073,#52074,#52075,#52076,
#52077,#52078,#52079,#52080,#52081,#52082),.UNSPECIFIED.,.F.,.F.,(4,1,1,
1,1,1,1,1,4),(378.114767136919,378.90661870899,379.906372320359,380.906125931729,
381.406002737414,381.905879543098,382.905633154468,383.905386765837,384.397952444099),
 .UNSPECIFIED.);
#482=B_SPLINE_CURVE_WITH_KNOTS('',3,(#52084,#52085,#52086,#52087,#52088,
#52089,#52090,#52091,#52092,#52093,#52094,#52095,#52096,#52097,#52098,#52099,
#52100,#52101),.UNSPECIFIED.,.F.,.F.,(4,2,2,2,2,2,2,2,4),(384.397952444099,
385.232869355993,386.067786267888,386.902703179783,387.737620091678,388.572537003573,
389.407453915467,390.242370827362,390.681137751278),.UNSPECIFIED.);
#483=B_SPLINE_CURVE_WITH_KNOTS('',3,(#52103,#52104,#52105,#52106,#52107,
#52108,#52109,#52110,#52111,#52112,#52113,#52114,#52115,#52116,#52117,#52118,
#52119,#52120),.UNSPECIFIED.,.F.,.F.,(4,2,2,2,2,2,2,2,4),(390.681137751278,
391.516054663173,392.350971575068,393.185888486963,394.020805398858,394.855722310753,
395.690639222648,396.525556134543,396.964110947501),.UNSPECIFIED.);
#484=B_SPLINE_CURVE_WITH_KNOTS('',3,(#52122,#52123,#52124,#52125,#52126,
#52127,#52128,#52129,#52130,#52131,#52132),.UNSPECIFIED.,.F.,.F.,(4,1,1,
1,1,1,1,1,4),(396.964751450397,397.901937325008,398.901690936378,399.901444547747,
400.901198159116,401.900951770486,402.40082857617,402.900705381855,403.247508365637),
 .UNSPECIFIED.);
#485=B_SPLINE_CURVE_WITH_KNOTS('',3,(#52134,#52135,#52136,#52137,#52138,
#52139,#52140,#52141,#52142,#52143,#52144,#52145,#52146,#52147,#52148,#52149,
#52150,#52151),.UNSPECIFIED.,.F.,.F.,(4,2,2,2,2,2,2,2,4),(403.247508365637,
404.082425277532,404.917342189427,405.752259101322,406.587176013217,407.422092925111,
408.257009837006,409.091926748901,409.530693672817),.UNSPECIFIED.);
#486=B_SPLINE_CURVE_WITH_KNOTS('',3,(#52153,#52154,#52155,#52156,#52157,
#52158,#52159,#52160,#52161,#52162,#52163,#52164,#52165,#52166,#52167,#52168,
#52169,#52170,#52171,#52172,#52173,#52174,#52175,#52176,#52177,#52178,#52179,
#52180,#52181,#52182,#52183,#52184,#52185,#52186,#52187,#52188,#52189,#52190,
#52191,#52192,#52193,#52194,#52195,#52196,#52197,#52198,#52199,#52200,#52201,
#52202,#52203,#52204,#52205,#52206,#52207,#52208,#52209,#52210,#52211,#52212,
#52213,#52214,#52215,#52216,#52217,#52218,#52219,#52220,#52221,#52222,#52223,
#52224,#52225,#52226,#52227,#52228,#52229,#52230,#52231,#52232,#52233,#52234,
#52235,#52236,#52237,#52238,#52239,#52240,#52241,#52242,#52243,#52244,#52245,
#52246,#52247,#52248,#52249,#52250,#52251,#52252,#52253,#52254,#52255,#52256,
#52257,#52258,#52259,#52260,#52261,#52262,#52263,#52264,#52265,#52266,#52267,
#52268,#52269,#52270,#52271,#52272,#52273,#52274,#52275,#52276,#52277,#52278,
#52279,#52280,#52281,#52282,#52283,#52284,#52285,#52286,#52287,#52288,#52289,
#52290,#52291,#52292,#52293,#52294,#52295,#52296,#52297,#52298,#52299,#52300,
#52301,#52302,#52303,#52304,#52305,#52306,#52307,#52308,#52309,#52310,#52311,
#52312,#52313,#52314,#52315,#52316,#52317,#52318,#52319,#52320,#52321,#52322,
#52323,#52324,#52325,#52326,#52327,#52328,#52329,#52330,#52331,#52332,#52333,
#52334,#52335,#52336,#52337,#52338,#52339,#52340,#52341,#52342,#52343,#52344,
#52345,#52346,#52347,#52348,#52349,#52350,#52351,#52352,#52353,#52354,#52355,
#52356,#52357,#52358,#52359,#52360,#52361,#52362,#52363,#52364,#52365,#52366,
#52367,#52368,#52369,#52370,#52371,#52372,#52373,#52374,#52375,#52376,#52377,
#52378,#52379,#52380,#52381,#52382,#52383,#52384,#52385,#52386,#52387,#52388,
#52389,#52390,#52391,#52392,#52393,#52394,#52395,#52396,#52397,#52398,#52399,
#52400,#52401,#52402,#52403,#52404,#52405,#52406,#52407,#52408,#52409,#52410,
#52411,#52412,#52413,#52414,#52415,#52416,#52417),.UNSPECIFIED.,.F.,.F.,
(4,3,3,3,3,3,3,3,3,3,3,3,3,3,3,3,3,3,3,3,3,3,3,3,3,3,3,3,3,3,3,3,3,3,3,
3,3,3,3,3,3,3,3,3,3,3,3,3,3,3,3,3,3,3,3,3,3,3,3,3,3,3,3,3,3,3,3,3,3,3,3,
3,3,3,3,3,3,3,3,3,3,3,3,3,3,3,3,3,4),(409.530693672817,409.613310095046,
409.696287231429,409.779442667476,409.862825827951,409.898980661441,409.973527856939,
410.047999420673,410.122409225397,410.196771103143,410.271098853999,410.34540625453,
410.419722330409,410.494047675697,410.568394762051,410.642776070258,410.717243608842,
410.791760491795,410.86638003412,410.89873427281,410.972639862935,411.046458434796,
411.120204460962,411.19389236008,411.267536508093,411.341151248603,411.414763063285,
411.488376908039,411.562005747365,411.635662552356,411.709399462699,411.783181110965,
411.857064303458,411.898487884179,411.973036785119,412.047504638902,412.121905371562,
412.196252864725,412.270560964623,412.344843490695,412.419126989672,412.4934149635,
412.56771991291,412.642054345261,412.71646808396,412.790927138046,412.865483140952,
412.898241495549,412.972790221053,413.047257927567,413.121658541024,413.196005942973,
413.270313979581,413.344596470241,413.418879975516,413.493167981632,413.567472989327,
413.641807505984,413.716221367926,413.790680567655,413.86523674946,413.897995106918,
413.971874321331,414.045670718289,414.11939875344,414.193072831897,414.266707319181,
414.340316551375,414.413929103393,414.487547555526,414.561184873909,414.634854033511,
414.708609166364,414.78241237518,414.856322221874,414.897748718287,414.971657525898,
415.045480993506,415.119233611503,415.192929817296,415.266584006522,415.340215986607,
415.413838250846,415.487463784416,415.56110557239,415.634807941336,415.708545074942,
415.782363994766,415.813507283438),.UNSPECIFIED.);
#487=B_SPLINE_CURVE_WITH_KNOTS('',3,(#52419,#52420,#52421,#52422,#52423,
#52424,#52425,#52426,#52427,#52428,#52429,#52430,#52431,#52432,#52433,#52434,
#52435,#52436),.UNSPECIFIED.,.F.,.F.,(4,2,2,2,2,2,2,2,4),(415.814026695158,
416.648795891891,417.483712803786,418.318629715681,419.153546627576,419.988463539471,
420.823380451366,421.658297363261,422.097064287176),.UNSPECIFIED.);
#488=B_SPLINE_CURVE_WITH_KNOTS('',3,(#52438,#52439,#52440,#52441,#52442,
#52443,#52444,#52445,#52446,#52447,#52448,#52449,#52450,#52451,#52452,#52453,
#52454,#52455),.UNSPECIFIED.,.F.,.F.,(4,2,2,2,2,2,2,2,4),(422.097064287176,
422.931981199071,423.766898110966,424.601815022861,425.436731934755,426.27164884665,
427.106565758545,427.94148267044,428.380249594356),.UNSPECIFIED.);
#489=B_SPLINE_CURVE_WITH_KNOTS('',3,(#52457,#52458,#52459,#52460,#52461,
#52462,#52463,#52464,#52465,#52466,#52467,#52468,#52469,#52470,#52471,#52472,
#52473,#52474),.UNSPECIFIED.,.F.,.F.,(4,2,2,2,2,2,2,2,4),(428.380249594356,
429.21516650625,430.050083418145,430.88500033004,431.719917241935,432.55483415383,
433.389751065724,434.224667977619,434.663434901535),.UNSPECIFIED.);
#490=B_SPLINE_CURVE_WITH_KNOTS('',3,(#52476,#52477,#52478,#52479,#52480,
#52481,#52482,#52483,#52484,#52485,#52486,#52487),.UNSPECIFIED.,.F.,.F.,
(4,1,1,1,1,1,1,1,1,4),(434.663434901535,434.892820945675,435.892574557044,
436.892328168413,437.392204974098,437.892081779783,438.891835391152,439.891589002521,
440.891342613891,440.946620208715),.UNSPECIFIED.);
#491=B_SPLINE_CURVE_WITH_KNOTS('',3,(#52489,#52490,#52491,#52492,#52493,
#52494,#52495,#52496,#52497,#52498,#52499,#52500,#52501,#52502,#52503,#52504,
#52505,#52506,#52507,#52508,#52509,#52510,#52511,#52512,#52513,#52514,#52515,
#52516,#52517,#52518,#52519,#52520,#52521,#52522,#52523,#52524,#52525,#52526,
#52527,#52528,#52529,#52530,#52531,#52532,#52533,#52534,#52535,#52536,#52537,
#52538,#52539,#52540,#52541,#52542,#52543,#52544,#52545,#52546,#52547,#52548,
#52549,#52550,#52551,#52552,#52553,#52554,#52555,#52556,#52557,#52558,#52559,
#52560,#52561,#52562,#52563,#52564,#52565,#52566,#52567,#52568,#52569,#52570,
#52571,#52572,#52573,#52574,#52575,#52576,#52577,#52578,#52579,#52580,#52581,
#52582,#52583,#52584,#52585,#52586,#52587,#52588,#52589,#52590,#52591,#52592,
#52593,#52594,#52595,#52596,#52597,#52598,#52599,#52600,#52601,#52602,#52603,
#52604,#52605,#52606,#52607,#52608,#52609,#52610,#52611,#52612,#52613,#52614,
#52615,#52616,#52617,#52618,#52619,#52620,#52621,#52622,#52623,#52624,#52625,
#52626,#52627,#52628,#52629,#52630,#52631,#52632,#52633,#52634,#52635,#52636,
#52637,#52638,#52639,#52640,#52641,#52642,#52643,#52644,#52645,#52646,#52647,
#52648,#52649,#52650,#52651,#52652,#52653,#52654,#52655,#52656,#52657,#52658,
#52659,#52660,#52661,#52662,#52663,#52664,#52665,#52666,#52667,#52668,#52669,
#52670,#52671,#52672,#52673,#52674,#52675,#52676,#52677,#52678,#52679,#52680,
#52681,#52682,#52683,#52684,#52685,#52686,#52687,#52688,#52689,#52690,#52691,
#52692,#52693,#52694,#52695,#52696,#52697,#52698,#52699,#52700,#52701,#52702,
#52703,#52704,#52705,#52706,#52707,#52708,#52709,#52710,#52711,#52712,#52713,
#52714,#52715,#52716,#52717,#52718,#52719,#52720,#52721,#52722,#52723,#52724,
#52725,#52726,#52727,#52728,#52729,#52730,#52731,#52732,#52733,#52734,#52735,
#52736,#52737,#52738,#52739,#52740,#52741,#52742,#52743,#52744,#52745,#52746,
#52747,#52748,#52749,#52750),.UNSPECIFIED.,.F.,.F.,(4,3,3,3,3,3,3,3,3,3,
3,3,3,3,3,3,3,3,3,3,3,3,3,3,3,3,3,3,3,3,3,3,3,3,3,3,3,3,3,3,3,3,3,3,3,3,
3,3,3,3,3,3,3,3,3,3,3,3,3,3,3,3,3,3,3,3,3,3,3,3,3,3,3,3,3,3,3,3,3,3,3,3,
3,3,3,3,3,4),(440.946620208715,441.020560156546,441.09442187872,441.168219784299,
441.241968235874,441.315681560049,441.389384092514,441.463083360364,441.536792301702,
441.61052385813,441.684330832929,441.758177779877,441.832127614359,441.89109622526,
441.964975439673,442.038771836632,442.112499871783,442.18617395024,442.259808437525,
442.333417669719,442.407030221737,442.48064867387,442.554285992254,442.627955151857,
442.701710284709,442.775513493525,442.84942334022,442.89084983663,442.965461317537,
443.039986841473,443.114440317424,443.188835606793,443.263186532514,443.337506887736,
443.411820631673,443.486134117959,443.560459814632,443.634810193835,443.709232537343,
443.783696014155,443.858249974174,443.890603447999,443.968966870234,444.047233439207,
444.125408448295,444.203465749673,444.281451066982,444.359346688836,444.390480253684,
444.468386311802,444.546362430945,444.624413745972,444.702595014756,444.780847186587,
444.859219359637,444.890357059368,444.964904254867,445.039375818601,445.113785623325,
445.188147501072,445.262475251928,445.336782652459,445.41109872834,445.485424073628,
445.559771159982,445.634152468189,445.708620006774,445.783136889728,445.857756432054,
445.890110670738,445.964016260863,446.037834832724,446.11158085889,446.185268758008,
446.258912906021,446.332527646531,446.406139461213,446.479753305967,446.553382145294,
446.627038950284,446.700775860626,446.774557508893,446.848440701386,446.889864282107,
446.977735760725,447.065254939028,447.152031804136,447.229805515894),
 .UNSPECIFIED.);
#492=B_SPLINE_CURVE_WITH_KNOTS('',3,(#52752,#52753,#52754,#52755,#52756,
#52757,#52758,#52759,#52760,#52761,#52762,#52763,#52764,#52765,#52766,#52767,
#52768,#52769),.UNSPECIFIED.,.F.,.F.,(4,2,2,2,2,2,2,2,4),(447.229805515894,
448.064722427789,448.899639339684,449.734556251579,450.569473163474,451.404390075369,
452.239306987263,453.074223899158,453.512990823074),.UNSPECIFIED.);
#493=B_SPLINE_CURVE_WITH_KNOTS('',3,(#52771,#52772,#52773,#52774,#52775,
#52776,#52777,#52778,#52779,#52780,#52781),.UNSPECIFIED.,.F.,.F.,(4,1,1,
1,1,1,1,1,4),(453.512990823074,453.888139561693,454.887893173062,455.887646784431,
456.887400395801,457.88715400717,458.387030812855,458.886907618539,459.795912565867),
 .UNSPECIFIED.);
#494=B_SPLINE_CURVE_WITH_KNOTS('',3,(#52783,#52784,#52785,#52786,#52787,
#52788,#52789,#52790,#52791,#52792,#52793,#52794,#52795,#52796,#52797,#52798,
#52799,#52800),.UNSPECIFIED.,.F.,.F.,(4,2,2,2,2,2,2,2,4),(459.796309024329,
460.631093042148,461.466009954043,462.300926865938,463.135843777833,463.970760689728,
464.805677601623,465.640594513517,466.079185816377),.UNSPECIFIED.);
#495=B_SPLINE_CURVE_WITH_KNOTS('',3,(#52802,#52803,#52804,#52805,#52806,
#52807,#52808,#52809,#52810,#52811,#52812,#52813,#52814,#52815,#52816,#52817,
#52818,#52819,#52820,#52821,#52822,#52823,#52824,#52825,#52826,#52827,#52828,
#52829,#52830,#52831,#52832,#52833,#52834,#52835,#52836,#52837,#52838,#52839,
#52840,#52841,#52842,#52843,#52844,#52845,#52846,#52847,#52848,#52849,#52850,
#52851,#52852,#52853,#52854,#52855,#52856,#52857,#52858,#52859,#52860,#52861,
#52862,#52863,#52864,#52865,#52866,#52867,#52868,#52869,#52870,#52871,#52872,
#52873,#52874,#52875,#52876,#52877,#52878,#52879,#52880,#52881,#52882,#52883,
#52884,#52885,#52886,#52887,#52888,#52889,#52890,#52891,#52892,#52893,#52894,
#52895,#52896,#52897,#52898,#52899,#52900,#52901,#52902,#52903,#52904,#52905,
#52906,#52907,#52908,#52909,#52910,#52911,#52912,#52913,#52914,#52915,#52916,
#52917,#52918,#52919,#52920,#52921,#52922,#52923,#52924,#52925,#52926,#52927,
#52928,#52929,#52930,#52931,#52932,#52933,#52934,#52935,#52936,#52937,#52938,
#52939,#52940,#52941,#52942,#52943,#52944,#52945,#52946,#52947,#52948,#52949,
#52950,#52951,#52952,#52953,#52954,#52955,#52956,#52957,#52958,#52959,#52960,
#52961,#52962,#52963,#52964,#52965,#52966,#52967,#52968,#52969,#52970,#52971,
#52972,#52973,#52974,#52975,#52976,#52977,#52978,#52979,#52980,#52981,#52982,
#52983,#52984,#52985,#52986,#52987,#52988,#52989,#52990,#52991,#52992,#52993,
#52994,#52995,#52996,#52997,#52998,#52999,#53000,#53001,#53002,#53003,#53004,
#53005,#53006,#53007,#53008,#53009,#53010,#53011,#53012,#53013,#53014,#53015,
#53016,#53017,#53018,#53019,#53020,#53021,#53022,#53023,#53024,#53025,#53026,
#53027,#53028,#53029,#53030,#53031,#53032,#53033,#53034,#53035,#53036,#53037,
#53038,#53039,#53040,#53041,#53042,#53043,#53044,#53045,#53046,#53047,#53048,
#53049,#53050,#53051,#53052,#53053,#53054,#53055,#53056,#53057,#53058,#53059,
#53060,#53061,#53062,#53063),.UNSPECIFIED.,.F.,.F.,(4,3,3,3,3,3,3,3,3,3,
3,3,3,3,3,3,3,3,3,3,3,3,3,3,3,3,3,3,3,3,3,3,3,3,3,3,3,3,3,3,3,3,3,3,3,3,
3,3,3,3,3,3,3,3,3,3,3,3,3,3,3,3,3,3,3,3,3,3,3,3,3,3,3,3,3,3,3,3,3,3,3,3,
3,3,3,3,3,4),(466.079976970098,466.153619284154,466.227213255373,466.300773314523,
466.374325227318,466.447875280061,466.521436506691,466.595021945881,466.668687639501,
466.742394771962,466.816212680748,466.884936509494,466.958842109278,467.032660690828,
467.106406726706,467.180094635551,467.253738793301,467.32735354355,467.400965367951,
467.474579222412,467.548208071428,467.621864886085,467.695601806015,467.76938346384,
467.843266665768,467.884690120864,467.959239000019,468.033706832004,468.108107542872,
468.182455014268,468.256763092443,468.331045596854,468.405329074328,468.479617026755,
468.55392195488,468.628256366081,468.702670083932,468.777129117314,468.851685099901,
468.884443732233,468.958992465446,469.033460179542,469.107860800451,469.182208209713,
469.256516253494,469.33079875118,469.405082263242,469.479370275996,469.553675290175,
469.628009813158,469.702423681156,469.776882886798,469.851439074247,469.884197343602,
469.958076624804,470.031873088724,470.105601190962,470.179275336584,470.252909891066,
470.326519190445,470.400131809449,470.473750328456,470.547387713562,470.621056939692,
470.694812138466,470.768615412974,470.842525324438,470.883950954972,470.958562234393,
471.033087557408,471.107540833182,471.181935923298,471.256286650874,471.330606809237,
471.404920358837,471.479233652386,471.553559158087,471.62790934825,471.70233150652,
471.776794800021,471.851348581114,471.883704566341,471.96265957517,472.041511482441,
472.121770297984,472.200388734976,472.281467739794,472.362546744612),
 .UNSPECIFIED.);
#496=B_SPLINE_CURVE_WITH_KNOTS('',3,(#53065,#53066,#53067,#53068,#53069,
#53070,#53071,#53072,#53073,#53074,#53075,#53076,#53077,#53078,#53079,#53080,
#53081,#53082),.UNSPECIFIED.,.F.,.F.,(4,2,2,2,2,2,2,2,4),(472.362546744612,
473.197463656507,474.032380568402,474.867297480297,475.702214392192,476.537131304087,
477.372048215982,478.206965127877,478.645732051792),.UNSPECIFIED.);
#497=B_SPLINE_CURVE_WITH_KNOTS('',3,(#53084,#53085,#53086,#53087,#53088,
#53089,#53090,#53091),.UNSPECIFIED.,.F.,.F.,(4,1,1,1,1,4),(478.645732051792,
478.881979845927,479.381856651612,479.881733457296,480.881487068666,480.943277745408),
 .UNSPECIFIED.);
#498=B_SPLINE_CURVE_WITH_KNOTS('',3,(#53095,#53096,#53097,#53098,#53099,
#53100),.UNSPECIFIED.,.F.,.F.,(4,2,4),(-483.018264218093,-482.185091679657,
-481.615013765778),.UNSPECIFIED.);
#499=B_SPLINE_CURVE_WITH_KNOTS('',3,(#53102,#53103,#53104,#53105,#53106,
#53107,#53108,#53109,#53110,#53111,#53112),.UNSPECIFIED.,.F.,.F.,(4,1,1,
1,1,1,1,1,4),(-481.615013765778,-481.232659880542,-480.234251872491,-479.23584386444,
-478.237435856389,-477.738231852364,-477.239027848338,-476.240619840287,
-475.332179850449),.UNSPECIFIED.);
#500=B_SPLINE_CURVE_WITH_KNOTS('',3,(#53114,#53115,#53116,#53117,#53118,
#53119,#53120,#53121,#53122,#53123,#53124,#53125,#53126,#53127,#53128,#53129,
#53130,#53131,#53132,#53133,#53134,#53135,#53136,#53137,#53138,#53139,#53140,
#53141,#53142,#53143,#53144,#53145,#53146,#53147,#53148,#53149,#53150,#53151,
#53152,#53153,#53154,#53155,#53156,#53157,#53158,#53159,#53160,#53161,#53162,
#53163,#53164,#53165,#53166,#53167,#53168,#53169,#53170,#53171,#53172,#53173,
#53174,#53175,#53176,#53177,#53178,#53179,#53180,#53181,#53182,#53183,#53184,
#53185,#53186,#53187,#53188,#53189,#53190,#53191,#53192,#53193,#53194,#53195,
#53196,#53197,#53198,#53199,#53200,#53201,#53202,#53203,#53204,#53205,#53206,
#53207,#53208,#53209,#53210,#53211,#53212,#53213,#53214,#53215,#53216,#53217,
#53218,#53219,#53220,#53221,#53222,#53223,#53224,#53225,#53226,#53227,#53228,
#53229,#53230,#53231,#53232,#53233,#53234,#53235,#53236,#53237,#53238,#53239,
#53240,#53241,#53242,#53243,#53244,#53245,#53246,#53247,#53248,#53249,#53250,
#53251,#53252,#53253,#53254,#53255,#53256,#53257,#53258,#53259,#53260,#53261,
#53262,#53263,#53264,#53265,#53266,#53267,#53268,#53269,#53270,#53271,#53272,
#53273,#53274,#53275,#53276,#53277,#53278,#53279,#53280,#53281,#53282,#53283,
#53284,#53285,#53286,#53287,#53288,#53289,#53290,#53291,#53292,#53293,#53294,
#53295,#53296,#53297,#53298,#53299,#53300,#53301,#53302,#53303,#53304,#53305,
#53306,#53307,#53308,#53309,#53310,#53311,#53312,#53313,#53314,#53315,#53316,
#53317,#53318,#53319,#53320,#53321,#53322,#53323,#53324,#53325,#53326,#53327,
#53328,#53329,#53330,#53331,#53332,#53333,#53334,#53335,#53336,#53337,#53338,
#53339,#53340,#53341,#53342,#53343,#53344,#53345,#53346,#53347,#53348,#53349,
#53350,#53351,#53352,#53353,#53354,#53355,#53356,#53357,#53358,#53359,#53360,
#53361,#53362,#53363,#53364,#53365,#53366,#53367,#53368,#53369,#53370,#53371,
#53372,#53373,#53374,#53375,#53376,#53377,#53378,#53379,#53380,#53381,#53382,
#53383,#53384,#53385,#53386,#53387,#53388,#53389,#53390,#53391,#53392,#53393,
#53394,#53395,#53396,#53397,#53398,#53399,#53400,#53401,#53402,#53403,#53404,
#53405,#53406,#53407,#53408,#53409,#53410,#53411,#53412,#53413,#53414,#53415,
#53416,#53417,#53418,#53419,#53420,#53421,#53422,#53423,#53424,#53425,#53426,
#53427,#53428,#53429,#53430,#53431,#53432,#53433,#53434,#53435,#53436,#53437,
#53438,#53439,#53440,#53441,#53442,#53443,#53444,#53445,#53446,#53447,#53448,
#53449,#53450,#53451,#53452,#53453,#53454,#53455,#53456,#53457,#53458,#53459,
#53460,#53461,#53462,#53463,#53464,#53465,#53466,#53467,#53468,#53469,#53470,
#53471,#53472,#53473,#53474,#53475,#53476,#53477,#53478,#53479,#53480,#53481,
#53482,#53483,#53484,#53485,#53486,#53487,#53488,#53489,#53490,#53491,#53492,
#53493,#53494,#53495,#53496,#53497,#53498,#53499,#53500,#53501,#53502,#53503,
#53504,#53505,#53506,#53507,#53508,#53509,#53510,#53511,#53512,#53513,#53514,
#53515,#53516,#53517,#53518,#53519,#53520,#53521,#53522,#53523,#53524,#53525,
#53526,#53527,#53528,#53529,#53530,#53531,#53532,#53533,#53534,#53535,#53536,
#53537,#53538,#53539,#53540,#53541,#53542,#53543,#53544,#53545,#53546,#53547,
#53548,#53549,#53550,#53551,#53552,#53553,#53554,#53555,#53556,#53557,#53558,
#53559,#53560,#53561,#53562,#53563,#53564,#53565,#53566,#53567,#53568,#53569,
#53570,#53571,#53572,#53573,#53574,#53575,#53576,#53577,#53578,#53579,#53580,
#53581,#53582,#53583,#53584,#53585,#53586,#53587,#53588,#53589,#53590,#53591,
#53592,#53593,#53594,#53595,#53596,#53597,#53598,#53599,#53600,#53601,#53602,
#53603,#53604,#53605,#53606,#53607,#53608,#53609,#53610,#53611,#53612,#53613,
#53614,#53615,#53616,#53617,#53618,#53619,#53620,#53621,#53622,#53623,#53624,
#53625,#53626,#53627,#53628,#53629,#53630,#53631,#53632,#53633,#53634,#53635,
#53636,#53637,#53638,#53639,#53640,#53641,#53642,#53643,#53644,#53645,#53646,
#53647,#53648,#53649,#53650,#53651,#53652,#53653,#53654,#53655,#53656,#53657,
#53658,#53659,#53660,#53661,#53662,#53663,#53664,#53665,#53666,#53667,#53668,
#53669,#53670,#53671,#53672,#53673,#53674,#53675,#53676,#53677,#53678,#53679,
#53680,#53681,#53682,#53683,#53684,#53685,#53686,#53687,#53688,#53689,#53690,
#53691,#53692,#53693,#53694,#53695,#53696,#53697,#53698,#53699,#53700,#53701),
 .UNSPECIFIED.,.F.,.F.,(4,2,2,2,2,2,2,2,2,2,2,2,2,2,2,2,2,2,2,2,2,2,2,2,
2,2,2,2,2,2,2,2,2,2,2,2,2,2,2,2,2,2,2,2,2,2,2,2,2,2,2,2,2,2,2,2,2,2,2,2,
2,2,2,2,2,2,2,2,2,2,2,2,2,2,2,2,2,2,2,2,2,2,2,2,2,2,2,2,2,2,2,2,2,2,2,2,
2,2,2,2,2,2,2,2,2,2,2,2,2,2,2,2,2,2,2,2,2,2,2,2,2,2,2,2,2,2,2,2,2,2,2,2,
2,2,2,2,2,2,2,2,2,2,2,2,2,2,2,2,2,2,2,2,2,2,2,2,2,2,2,2,2,2,2,2,2,2,2,2,
2,2,2,2,2,2,2,2,2,2,2,2,2,2,2,2,2,2,2,2,2,2,2,2,2,2,2,2,2,2,2,2,2,2,2,2,
2,2,2,2,2,2,2,2,2,2,2,2,2,2,2,2,2,2,2,2,2,2,2,2,2,2,2,2,2,2,2,2,2,2,2,2,
2,2,2,2,2,2,2,2,2,2,2,2,2,2,2,2,2,2,2,2,2,2,2,2,2,2,2,2,2,2,2,2,2,2,2,2,
2,2,2,2,2,2,2,2,2,2,2,2,2,2,2,2,2,4),(0.00198539612204261,0.0695281946069639,
0.0716483733971968,0.072969179381184,0.073972076551303,0.0749290983747497,
0.0758740341322982,0.0771441643805482,0.0802753384618654,0.11032324343002,
0.120039710884885,0.130454021338825,0.144461220265735,0.151158722935033,
0.363084719465787,0.454778594390875,0.4681349076702,0.471634360179192,0.473707948100735,
0.475542044892056,0.477833097855689,0.481371568867902,0.497446719655115,
0.778439388533868,0.818672492655279,0.846116047052023,0.855305827777556,
0.859172379250651,0.862094882651062,0.863455907775944,0.864442270617736,
0.865420353844057,0.866764935167273,0.869447100869893,0.892145023370465,
0.979737381538867,1.02398715311802,1.03736197047494,1.05265555968575,1.07043577687286,
1.09161394131366,1.16332718260169,1.21958320072858,1.24587362438719,1.25017773952524,
1.25242763347541,1.25408374066612,1.25587302246596,1.25844960236438,1.26565341123742,
1.27742634412946,1.53673525408729,1.60905511442089,1.63591159939473,1.64467059680943,
1.64838242997261,1.65120040753821,1.65252329121769,1.65348787930181,1.65443968533278,
1.65573652623811,1.65901300331603,1.69843339768578,1.80866273025028,1.98900072378921,
2.03584381354957,2.0446062523711,2.04753298908035,2.04942970210845,2.05122099999774,
2.05358346656273,2.05885699648111,2.10270998483147,2.10509827111799,2.11192125691502,
2.11943545989609,2.34943040262198,2.40685031023406,2.43822380802002,2.44179511876934,
2.44450865366691,2.44578773027049,2.44672257302339,2.44764719220153,2.448923625156,
2.45217539313844,2.49144714050303,2.49424509901302,2.69754764137921,2.71034855786606,
2.72487718823149,2.74179232383359,2.76235660355928,2.84197157690997,2.85423034514522,
2.85755998382333,2.85955673968097,2.86133782859566,2.86358260911417,2.86708760972244,
2.88361159567327,3.14610693198268,3.24739137343347,3.25348739652724,3.25559392926881,
3.25695616155746,3.25824599273288,3.25995271061636,3.26353756875168,3.29018256405163,
3.52810358341072,3.61108786406358,3.62601961855358,3.63080097964562,3.63385139291882,
3.63669002827845,3.64034460711267,3.64635727342268,3.67986555768184,3.88593006169828,
3.94648914665783,3.98693520425236,4.00606493204843,4.00913108619559,4.01072660008559,
4.01189780375313,4.01316011289113,4.01534920240838,4.02148880933641,4.10792534506172,
4.20914719257935,4.31736439579036,4.39842706092587,4.40403001113769,4.40649034009506,
4.40830260895753,4.40997659948598,4.41224826432733,4.41783899261654,4.47485505578666,
4.71800008987412,4.76459046956295,4.81166444119114,4.81855000693929,4.82038732051357,
4.82148241188958,4.82246306437885,4.82371014250117,4.82567954488016,4.8353260630709,
4.98259538975935,5.10994957207873,5.20750417298474,5.21401904105974,5.21643320229296,
5.21813631222369,5.219733861687,5.22193708240645,5.22626596375408,5.25648111595309,
5.3540931619433,5.58989094793188,5.61034088149828,5.61313429810774,5.61443501878184,
5.61545205917001,5.61655956749361,5.61833332045687,5.62416489431458,5.65922682939266,
5.72853199034163,5.78272325039861,5.85882676933152,5.99948411178665,6.00914421916709,
6.01237850579145,6.01419255739285,6.01584468599475,6.01804934296407,6.02213798290247,
6.04391039708453,6.08630957800502,6.13820806342962,6.2634291805327,6.37690477397915,
6.39908779934626,6.40201091950928,6.40338441389774,6.40443156985208,6.40555650373806,
6.40733606605516,6.41300200500401,6.44610734723482,6.51553803595748,6.57704285236464,
6.77430879573317,6.78735855004827,6.79092640313139,6.7930099515496,6.7946604386636,
6.79679336749758,6.80055352716823,6.81708426617341,6.87994192662831,6.93964084240221,
7.17595472550011,7.18930243288312,7.19154848261905,7.19288600902966,7.19390881611454,
7.1950001212912,7.19670600001893,7.20216479228494,7.23418971920697,7.28146810419425,
7.38223505699067,7.47687857406694,7.57869661925009,7.58545388975532,7.58812413296717,
7.58994973998226,7.59155375447143,7.59391316563354,7.59902973940588,7.67476473723677,
7.73426722392563,7.96953266292123,7.98287575677924,7.98507410654613,7.98637641689806,
7.98736832063171,7.98842611346783,7.99009391712742,7.99536731034472,8.02579760533239,
8.09520995465294,8.11571820202984,8.1683012150998,8.18949908798207,8.19744449917702,
8.20499631216658,8.21219193535937,8.29811088745238,8.38991537990947,8.39624932650762,
8.398646408409,8.40035392433461,8.40211252131302,8.4043908237084,8.4068895062419,
8.41098896619806,8.41916679068341,8.50146564518136,8.72278377822303,8.78961082403335,
8.79435638219568,8.79612479563324,8.79737560745655,8.79855126751737,8.80017644872472,
8.80338218776118,8.82624982003937,8.9350949730659,9.09991899962067,9.16097684959328,
9.16316410454399,9.16567212020523,9.16851195537729,9.17233875453396,9.17519046310607,
9.17815568852672,9.18253804083694,9.19443827821552,9.25204240797907,9.30482368907358,
9.528984484792,9.5466216554642,9.54952934708034,9.55125436302401,9.55257011153632,
9.55397084876998,9.55614764342539,9.56277813722868,9.59792562535676,9.64403532935967,
9.93113648162764,9.94273763261307,9.94626463558691,9.94851673288571,9.95021775518271,
9.95188223387109,9.9538123127537,9.95655547365957,9.96456728672837),
 .UNSPECIFIED.);
#501=B_SPLINE_CURVE_WITH_KNOTS('',3,(#53703,#53704,#53705,#53706,#53707,
#53708,#53709,#53710,#53711,#53712,#53713,#53714,#53715,#53716,#53717,#53718,
#53719,#53720,#53721,#53722,#53723,#53724,#53725,#53726,#53727,#53728,#53729,
#53730,#53731,#53732,#53733,#53734,#53735,#53736,#53737,#53738,#53739,#53740,
#53741,#53742,#53743,#53744,#53745,#53746,#53747,#53748,#53749,#53750,#53751,
#53752,#53753,#53754,#53755,#53756,#53757,#53758,#53759,#53760,#53761,#53762,
#53763,#53764,#53765,#53766,#53767,#53768,#53769,#53770,#53771,#53772,#53773,
#53774,#53775,#53776,#53777,#53778,#53779,#53780,#53781,#53782,#53783,#53784,
#53785,#53786,#53787,#53788,#53789,#53790,#53791,#53792,#53793,#53794,#53795,
#53796,#53797,#53798,#53799,#53800,#53801,#53802,#53803,#53804,#53805,#53806,
#53807,#53808,#53809,#53810,#53811,#53812,#53813,#53814,#53815,#53816,#53817,
#53818,#53819,#53820,#53821,#53822,#53823,#53824,#53825,#53826,#53827,#53828,
#53829,#53830,#53831,#53832,#53833,#53834,#53835,#53836,#53837,#53838,#53839,
#53840,#53841,#53842,#53843,#53844,#53845,#53846,#53847,#53848,#53849,#53850,
#53851,#53852,#53853,#53854,#53855,#53856,#53857,#53858,#53859,#53860,#53861,
#53862,#53863,#53864,#53865,#53866,#53867,#53868,#53869,#53870,#53871,#53872,
#53873,#53874,#53875,#53876,#53877,#53878,#53879,#53880,#53881,#53882,#53883,
#53884,#53885,#53886,#53887,#53888,#53889,#53890,#53891,#53892,#53893,#53894,
#53895,#53896,#53897,#53898,#53899,#53900,#53901,#53902,#53903,#53904,#53905,
#53906,#53907,#53908,#53909,#53910,#53911,#53912,#53913,#53914,#53915,#53916,
#53917,#53918,#53919,#53920,#53921,#53922,#53923,#53924,#53925,#53926,#53927,
#53928,#53929,#53930,#53931,#53932,#53933,#53934,#53935,#53936,#53937,#53938,
#53939,#53940,#53941,#53942,#53943,#53944,#53945,#53946,#53947,#53948,#53949,
#53950,#53951,#53952,#53953,#53954,#53955,#53956,#53957,#53958,#53959,#53960,
#53961,#53962,#53963,#53964,#53965,#53966,#53967),.UNSPECIFIED.,.F.,.F.,
(4,3,3,3,3,3,3,3,3,3,3,3,3,3,3,3,3,3,3,3,3,3,3,3,3,3,3,3,3,3,3,3,3,3,3,
3,3,3,3,3,3,3,3,3,3,3,3,3,3,3,3,3,3,3,3,3,3,3,3,3,3,3,3,3,3,3,3,3,3,3,3,
3,3,3,3,3,3,3,3,3,3,3,3,3,3,3,3,3,4),(-462.765457844239,-462.686733707007,
-462.607885241033,-462.528910893298,-462.449739943357,-462.37046153861,
-462.291017515773,-462.262907727575,-462.188987941163,-462.115154965673,
-462.041394339911,-461.96769165625,-461.894032549482,-461.82040268652,-461.746775610712,
-461.673146381543,-461.599502043651,-461.525829635064,-461.452077307501,
-461.378280156542,-461.304382129771,-461.264499719524,-461.189938657776,
-461.115458429897,-461.041045122637,-460.966684866971,-460.892363829109,
-460.818068201927,-460.743771465991,-460.669470136212,-460.595151722648,
-460.52080372868,-460.446376612285,-460.371904105249,-460.297335279547,
-460.266091711473,-460.191530725491,-460.11705056126,-460.042637305573,
-459.968277089437,-459.89395607909,-459.819660467428,-459.74536372908,-459.671062385706,
-459.596743947358,-459.522395917408,-459.447968748305,-459.373496178922,
-459.298927276623,-459.267683703422,-459.193790222148,-459.119979355985,
-459.046236660541,-458.972547741626,-458.89889824438,-458.825273843175,
-458.751645996229,-458.678012130141,-458.604359287906,-458.530674503678,
-458.456903950761,-458.383085240126,-458.30916058924,-458.269275695371,
-458.194652629911,-458.120115300983,-458.045649812182,-457.971242314493,
-457.896878997203,-457.822546079253,-457.74821961661,-457.673893284606,
-457.599554625761,-457.525191178434,-457.450755921203,-457.376279447764,
-457.301713075574,-457.27086768732,-457.1925020134,-457.114232844084,-457.036054897808,
-456.957994125735,-456.880005063599,-456.802105210717,-456.771663683295,
-456.699193493567,-456.626711514643,-456.55416419583,-456.482828943308),
 .UNSPECIFIED.);
#502=B_SPLINE_CURVE_WITH_KNOTS('',3,(#53969,#53970,#53971,#53972,#53973,
#53974,#53975,#53976,#53977,#53978,#53979,#53980,#53981,#53982,#53983,#53984,
#53985,#53986),.UNSPECIFIED.,.F.,.F.,(4,2,2,2,2,2,2,2,4),(-456.482201859304,
-455.647355625165,-454.81243871327,-453.977521801375,-453.14260488948,-452.307687977585,
-451.472771065691,-450.637854153796,-450.199157428511),.UNSPECIFIED.);
#503=B_SPLINE_CURVE_WITH_KNOTS('',3,(#53988,#53989,#53990,#53991,#53992,
#53993,#53994,#53995,#53996,#53997,#53998,#53999,#54000,#54001,#54002,#54003,
#54004,#54005,#54006,#54007,#54008,#54009,#54010,#54011,#54012,#54013,#54014,
#54015,#54016,#54017,#54018,#54019,#54020,#54021,#54022,#54023,#54024,#54025,
#54026,#54027,#54028,#54029,#54030,#54031,#54032,#54033,#54034,#54035,#54036,
#54037,#54038,#54039,#54040,#54041,#54042,#54043,#54044,#54045,#54046,#54047,
#54048,#54049,#54050,#54051,#54052,#54053,#54054,#54055,#54056,#54057,#54058,
#54059,#54060,#54061,#54062,#54063,#54064,#54065,#54066,#54067,#54068,#54069,
#54070,#54071,#54072,#54073,#54074,#54075,#54076,#54077,#54078,#54079,#54080,
#54081,#54082,#54083,#54084,#54085,#54086,#54087,#54088,#54089,#54090,#54091,
#54092,#54093,#54094,#54095,#54096,#54097,#54098,#54099,#54100,#54101,#54102,
#54103,#54104,#54105,#54106,#54107,#54108,#54109,#54110,#54111,#54112,#54113,
#54114,#54115,#54116,#54117,#54118,#54119,#54120,#54121,#54122,#54123,#54124,
#54125,#54126,#54127,#54128,#54129,#54130,#54131,#54132,#54133,#54134,#54135,
#54136,#54137,#54138,#54139,#54140,#54141,#54142,#54143,#54144,#54145,#54146,
#54147,#54148,#54149,#54150,#54151,#54152,#54153,#54154,#54155,#54156,#54157,
#54158,#54159,#54160,#54161,#54162,#54163,#54164,#54165,#54166,#54167,#54168,
#54169,#54170,#54171,#54172,#54173,#54174,#54175,#54176,#54177,#54178,#54179,
#54180,#54181,#54182,#54183,#54184,#54185,#54186,#54187,#54188,#54189,#54190,
#54191,#54192,#54193,#54194,#54195,#54196,#54197,#54198,#54199,#54200,#54201,
#54202,#54203,#54204,#54205,#54206,#54207,#54208,#54209,#54210,#54211,#54212,
#54213,#54214,#54215,#54216,#54217,#54218,#54219,#54220,#54221,#54222,#54223,
#54224,#54225,#54226,#54227,#54228,#54229,#54230,#54231,#54232,#54233,#54234,
#54235,#54236,#54237,#54238,#54239,#54240,#54241,#54242,#54243,#54244,#54245,
#54246,#54247,#54248,#54249,#54250,#54251,#54252),.UNSPECIFIED.,.F.,.F.,
(4,3,3,3,3,3,3,3,3,3,3,3,3,3,3,3,3,3,3,3,3,3,3,3,3,3,3,3,3,3,3,3,3,3,3,
3,3,3,3,3,3,3,3,3,3,3,3,3,3,3,3,3,3,3,3,3,3,3,3,3,3,3,3,3,3,3,3,3,3,3,3,
3,3,3,3,3,3,3,3,3,3,3,3,3,3,3,3,3,4),(-450.198883421911,-450.123484883473,
-450.048167901281,-449.972939821452,-449.897763337677,-449.822635356839,
-449.782807626938,-449.704897038825,-449.626916641923,-449.548861312063,
-449.470676596309,-449.392421216702,-449.314046526066,-449.283603622913,
-449.209044526386,-449.134560876773,-449.060138813668,-448.985764517231,
-448.911424199439,-448.837104095692,-448.762775226533,-448.688436993342,
-448.614076934992,-448.53968258119,-448.465202227618,-448.390672474616,
-448.316040743774,-448.285195614862,-448.211275828585,-448.137442853229,
-448.063682227601,-447.989979544073,-447.916320437438,-447.842690574608,
-447.769063498931,-447.695434269892,-447.621789932128,-447.548117523668,
-447.474365196231,-447.400568045397,-447.326670018748,-447.286787606811,
-447.212226545283,-447.137746317625,-447.063333010591,-446.988972755153,
-446.914651717522,-446.840356090572,-446.766059354873,-446.691758025332,
-446.617439612008,-446.543091618281,-446.468664502128,-446.394191995335,
-446.319623169876,-446.28837959876,-446.213818612626,-446.13933844824,-446.064925192397,
-445.990564976105,-445.9162439656,-445.841948353779,-445.767651615271,-445.693350271735,
-445.619031833226,-445.544683803114,-445.47025663385,-445.395784064305,
-445.321215161845,-445.289971590709,-445.216078109455,-445.142267243313,
-445.06852454789,-444.994835628994,-444.921186131768,-444.847561730584,
-444.773933883658,-444.70030001759,-444.626647175374,-444.552962391166,
-444.479191838268,-444.405373127653,-444.331448476786,-444.291563582658,
-444.205052052495,-444.119026734658,-444.033348198667,-443.94826036848,
-443.915901922701),.UNSPECIFIED.);
#504=B_SPLINE_CURVE_WITH_KNOTS('',3,(#54254,#54255,#54256,#54257,#54258,
#54259,#54260,#54261,#54262,#54263,#54264,#54265,#54266,#54267,#54268,#54269,
#54270,#54271),.UNSPECIFIED.,.F.,.F.,(4,2,2,2,2,2,2,2,4),(-443.915901922701,
-443.080985010806,-442.246068098911,-441.411151187016,-440.576234275121,
-439.741317363226,-438.906400451331,-438.071483539437,-437.632716615521),
 .UNSPECIFIED.);
#505=B_SPLINE_CURVE_WITH_KNOTS('',3,(#54273,#54274,#54275,#54276,#54277,
#54278,#54279,#54280,#54281,#54282,#54283),.UNSPECIFIED.,.F.,.F.,(4,1,1,
1,1,1,1,1,4),(-437.632716615521,-437.302707526302,-436.304299518251,-435.805095514225,
-435.3058915102,-434.307483502149,-433.309075494098,-432.310667486047,-431.349536372118),
 .UNSPECIFIED.);
#506=B_SPLINE_CURVE_WITH_KNOTS('',3,(#54285,#54286,#54287,#54288,#54289,
#54290,#54291,#54292,#54293,#54294,#54295,#54296,#54297,#54298,#54299,#54300,
#54301,#54302,#54303,#54304,#54305,#54306,#54307,#54308,#54309,#54310,#54311,
#54312,#54313,#54314,#54315,#54316,#54317,#54318,#54319,#54320,#54321,#54322,
#54323,#54324,#54325,#54326,#54327,#54328,#54329,#54330,#54331,#54332,#54333,
#54334,#54335,#54336,#54337,#54338,#54339,#54340,#54341,#54342,#54343,#54344,
#54345,#54346,#54347,#54348,#54349,#54350,#54351,#54352,#54353,#54354,#54355,
#54356,#54357,#54358,#54359,#54360,#54361,#54362,#54363,#54364,#54365,#54366,
#54367,#54368,#54369,#54370,#54371,#54372,#54373,#54374,#54375,#54376,#54377,
#54378,#54379,#54380,#54381,#54382,#54383,#54384,#54385,#54386,#54387,#54388,
#54389,#54390,#54391,#54392,#54393,#54394,#54395,#54396,#54397,#54398,#54399,
#54400,#54401,#54402,#54403,#54404,#54405,#54406,#54407,#54408,#54409,#54410,
#54411,#54412,#54413,#54414,#54415,#54416,#54417,#54418,#54419,#54420,#54421,
#54422,#54423,#54424,#54425,#54426,#54427,#54428,#54429,#54430,#54431,#54432,
#54433,#54434,#54435,#54436,#54437,#54438,#54439,#54440,#54441,#54442,#54443,
#54444,#54445,#54446,#54447,#54448,#54449,#54450,#54451,#54452,#54453,#54454,
#54455,#54456,#54457,#54458,#54459,#54460,#54461,#54462,#54463,#54464,#54465,
#54466,#54467,#54468,#54469,#54470,#54471,#54472,#54473,#54474,#54475,#54476,
#54477,#54478,#54479,#54480,#54481,#54482,#54483,#54484,#54485,#54486,#54487,
#54488,#54489,#54490,#54491,#54492,#54493,#54494,#54495,#54496,#54497,#54498,
#54499,#54500,#54501,#54502,#54503,#54504,#54505,#54506,#54507,#54508,#54509,
#54510,#54511,#54512,#54513,#54514,#54515,#54516,#54517,#54518,#54519,#54520,
#54521,#54522,#54523,#54524,#54525,#54526,#54527,#54528,#54529,#54530,#54531,
#54532,#54533,#54534,#54535,#54536,#54537,#54538,#54539,#54540,#54541,#54542,
#54543,#54544,#54545,#54546,#54547,#54548,#54549),.UNSPECIFIED.,.F.,.F.,
(4,3,3,3,3,3,3,3,3,3,3,3,3,3,3,3,3,3,3,3,3,3,3,3,3,3,3,3,3,3,3,3,3,3,3,
3,3,3,3,3,3,3,3,3,3,3,3,3,3,3,3,3,3,3,3,3,3,3,3,3,3,3,3,3,3,3,3,3,3,3,3,
3,3,3,3,3,3,3,3,3,3,3,3,3,3,3,3,3,4),(-431.349531308342,-431.312259477996,
-431.238365996742,-431.1645551306,-431.090812435177,-431.017123516282,-430.943474019055,
-430.869849617871,-430.796221770945,-430.722587904877,-430.648935062662,
-430.575250278454,-430.501479725556,-430.427661014941,-430.353736364073,
-430.313851469945,-430.239228404531,-430.16469107565,-430.090225586897,
-430.015818089256,-429.941454772013,-429.867121854112,-429.792795391517,
-429.718469059562,-429.644130400765,-429.569766953487,-429.495331696304,
-429.420855222913,-429.346288850772,-429.315443461894,-429.237077787853,
-429.158808618415,-429.080630672019,-429.002569899829,-428.924580837576,
-428.846680984581,-428.816239457869,-428.738328869755,-428.660348472851,
-428.58229314299,-428.504108427234,-428.425853047627,-428.347478356989,
-428.317035453843,-428.242476357316,-428.167992707704,-428.093570644599,
-428.019196348161,-427.944856030371,-427.870535926624,-427.796207057465,
-427.721868824275,-427.647508765924,-427.573114412122,-427.498634058549,
-427.424104305548,-427.349472574706,-427.318627445792,-427.244707659515,
-427.170874684159,-427.097114058531,-427.023411375003,-426.949752268368,
-426.876122405539,-426.802495329862,-426.728866100823,-426.65522176306,
-426.5815493546,-426.507797027163,-426.433999876329,-426.36010184968,-426.320219437742,
-426.245658376214,-426.171178148556,-426.096764841523,-426.022404586084,
-425.948083548453,-425.873787921505,-425.799491185805,-425.725189856265,
-425.65087144294,-425.576523449214,-425.50209633306,-425.427623826267,-425.353055000808,
-425.321811429691,-425.226177157113,-425.132161910787,-425.066346090687),
 .UNSPECIFIED.);
#507=B_SPLINE_CURVE_WITH_KNOTS('',3,(#54551,#54552,#54553,#54554,#54555,
#54556,#54557,#54558,#54559,#54560,#54561),.UNSPECIFIED.,.F.,.F.,(4,1,1,
1,1,1,1,1,4),(-425.066346001162,-424.32340342164,-423.324995413589,-422.326587405538,
-421.827383401512,-421.328179397487,-420.329771389436,-419.331363381385,
-418.783351185904),.UNSPECIFIED.);
#508=B_SPLINE_CURVE_WITH_KNOTS('',3,(#54563,#54564,#54565,#54566,#54567,
#54568,#54569,#54570,#54571,#54572,#54573,#54574,#54575,#54576,#54577,#54578,
#54579,#54580,#54581,#54582,#54583,#54584,#54585,#54586,#54587,#54588,#54589,
#54590,#54591,#54592,#54593,#54594,#54595,#54596,#54597,#54598,#54599,#54600,
#54601,#54602,#54603,#54604,#54605,#54606,#54607,#54608,#54609,#54610,#54611,
#54612,#54613,#54614,#54615,#54616,#54617,#54618,#54619,#54620,#54621,#54622,
#54623,#54624,#54625,#54626,#54627,#54628,#54629,#54630,#54631,#54632,#54633,
#54634,#54635,#54636,#54637,#54638,#54639,#54640,#54641,#54642,#54643,#54644,
#54645,#54646,#54647,#54648,#54649,#54650,#54651,#54652,#54653,#54654,#54655,
#54656,#54657,#54658,#54659,#54660,#54661,#54662,#54663,#54664,#54665,#54666,
#54667,#54668,#54669,#54670,#54671,#54672,#54673,#54674,#54675,#54676,#54677,
#54678,#54679,#54680,#54681,#54682,#54683,#54684,#54685,#54686,#54687,#54688,
#54689,#54690,#54691,#54692,#54693,#54694,#54695,#54696,#54697,#54698,#54699,
#54700,#54701,#54702,#54703,#54704,#54705,#54706,#54707,#54708,#54709,#54710,
#54711,#54712,#54713,#54714,#54715,#54716,#54717,#54718,#54719,#54720,#54721,
#54722,#54723,#54724,#54725,#54726,#54727,#54728,#54729,#54730,#54731,#54732,
#54733,#54734,#54735,#54736,#54737,#54738,#54739,#54740,#54741,#54742,#54743,
#54744,#54745,#54746,#54747,#54748,#54749,#54750,#54751,#54752,#54753,#54754,
#54755,#54756,#54757,#54758,#54759,#54760,#54761,#54762,#54763,#54764,#54765,
#54766,#54767,#54768,#54769,#54770,#54771,#54772,#54773,#54774,#54775,#54776,
#54777,#54778,#54779,#54780,#54781,#54782,#54783,#54784,#54785,#54786,#54787,
#54788,#54789,#54790,#54791,#54792,#54793,#54794,#54795,#54796,#54797,#54798,
#54799,#54800,#54801,#54802,#54803,#54804,#54805,#54806,#54807,#54808,#54809,
#54810,#54811,#54812,#54813,#54814,#54815,#54816,#54817,#54818,#54819,#54820,
#54821,#54822,#54823,#54824,#54825,#54826,#54827,#54828,#54829,#54830,#54831,
#54832,#54833,#54834,#54835,#54836,#54837,#54838,#54839,#54840,#54841,#54842,
#54843,#54844,#54845,#54846,#54847,#54848,#54849,#54850,#54851,#54852,#54853,
#54854,#54855,#54856,#54857,#54858,#54859,#54860,#54861,#54862,#54863,#54864,
#54865,#54866,#54867,#54868,#54869,#54870,#54871,#54872,#54873,#54874,#54875,
#54876,#54877,#54878,#54879,#54880,#54881,#54882,#54883,#54884,#54885,#54886,
#54887,#54888,#54889,#54890,#54891,#54892,#54893,#54894,#54895,#54896,#54897,
#54898,#54899,#54900,#54901,#54902,#54903,#54904,#54905,#54906,#54907,#54908,
#54909,#54910,#54911,#54912,#54913,#54914,#54915,#54916,#54917,#54918,#54919,
#54920,#54921,#54922,#54923,#54924,#54925,#54926,#54927,#54928,#54929,#54930,
#54931,#54932,#54933,#54934,#54935,#54936,#54937,#54938,#54939,#54940,#54941,
#54942,#54943,#54944,#54945,#54946,#54947,#54948,#54949,#54950,#54951,#54952,
#54953,#54954,#54955,#54956,#54957,#54958,#54959,#54960,#54961,#54962,#54963,
#54964,#54965,#54966,#54967,#54968,#54969,#54970,#54971,#54972,#54973,#54974,
#54975,#54976,#54977,#54978,#54979,#54980,#54981,#54982,#54983,#54984,#54985,
#54986,#54987,#54988,#54989,#54990,#54991,#54992,#54993,#54994,#54995,#54996,
#54997,#54998,#54999,#55000,#55001,#55002,#55003,#55004,#55005,#55006,#55007,
#55008,#55009,#55010,#55011,#55012,#55013,#55014,#55015,#55016,#55017,#55018,
#55019,#55020,#55021,#55022,#55023,#55024,#55025,#55026,#55027,#55028,#55029,
#55030,#55031,#55032,#55033,#55034,#55035,#55036,#55037,#55038,#55039,#55040,
#55041,#55042,#55043,#55044,#55045,#55046,#55047,#55048,#55049,#55050,#55051,
#55052,#55053,#55054,#55055,#55056,#55057,#55058,#55059,#55060,#55061,#55062,
#55063,#55064,#55065,#55066,#55067,#55068,#55069,#55070,#55071,#55072,#55073,
#55074,#55075,#55076,#55077,#55078,#55079,#55080,#55081,#55082,#55083,#55084,
#55085,#55086,#55087,#55088,#55089,#55090,#55091,#55092,#55093,#55094,#55095,
#55096,#55097,#55098,#55099,#55100,#55101,#55102,#55103,#55104,#55105,#55106,
#55107,#55108,#55109,#55110,#55111,#55112,#55113,#55114,#55115,#55116,#55117,
#55118,#55119,#55120,#55121,#55122,#55123,#55124,#55125,#55126,#55127,#55128,
#55129,#55130,#55131,#55132,#55133,#55134,#55135,#55136,#55137,#55138,#55139,
#55140,#55141,#55142,#55143,#55144,#55145,#55146,#55147,#55148,#55149,#55150,
#55151,#55152,#55153,#55154),.UNSPECIFIED.,.F.,.F.,(4,2,2,2,2,2,2,2,2,2,
2,2,2,2,2,2,2,2,2,2,2,2,2,2,2,2,2,2,2,2,2,2,2,2,2,2,2,2,2,2,2,2,2,2,2,2,
2,2,2,2,2,2,2,2,2,2,2,2,2,2,2,2,2,2,2,2,2,2,2,2,2,2,2,2,2,2,2,2,2,2,2,2,
2,2,2,2,2,2,2,2,2,2,2,2,2,2,2,2,2,2,2,2,2,2,2,2,2,2,2,2,2,2,2,2,2,2,2,2,
2,2,2,2,2,2,2,2,2,2,2,2,2,2,2,2,2,2,2,2,2,2,2,2,2,2,2,2,2,2,2,2,2,2,2,2,
2,2,2,2,2,2,2,2,2,2,2,2,2,2,2,2,2,2,2,2,2,2,2,2,2,2,2,2,2,2,2,2,2,2,2,2,
2,2,2,2,2,2,2,2,2,2,2,2,2,2,2,2,2,2,2,2,2,2,2,2,2,2,2,2,2,2,2,2,2,2,2,2,
2,2,2,2,2,2,2,2,2,2,2,2,2,2,2,2,2,2,2,2,2,2,2,2,2,2,2,2,2,2,2,2,2,2,2,2,
2,2,2,2,2,2,2,2,2,2,2,2,2,2,2,2,2,2,2,2,2,2,2,2,2,2,2,2,2,2,2,2,2,4),(0.0021107734850337,
0.313958519844044,0.35040009996185,0.356414794478,0.358234174092905,0.359367833469475,
0.360411547344041,0.361764528000124,0.364011936012669,0.376799783573237,
0.610136391080713,0.709427024510122,0.730459732642549,0.738807201515291,
0.74300297259584,0.745566374542952,0.747906260804457,0.749718256613466,
0.751482239056741,0.754467720453203,0.76242615398281,0.881084939228714,
0.943057554476376,1.05754177401902,1.10690754537228,1.13994018172288,1.14555813163525,
1.14730694929582,1.14840860341799,1.14942692467963,1.15073853363265,1.15292213128534,
1.16584495672315,1.41761405142509,1.47114434912135,1.50807569858058,1.52754146018385,
1.53534526331003,1.53929710978713,1.54172707645712,1.54395167436626,1.54568969179015,
1.54739382466881,1.54981364562728,1.55636884984881,1.65947926616869,1.71676694856147,
1.80926600952225,1.88350406002921,1.93135050162504,1.93830418565468,1.94015507138977,
1.94125709112926,1.94223511845872,1.94347238781967,1.94589446340493,1.95961792695883,
2.18939210654088,2.28466327834053,2.32641266982843,2.34055748272365,2.34671893492178,
2.35005225632904,2.35292677757035,2.35480362396226,2.35660681880789,2.35897650316781,
2.36298023110404,2.38744458822538,2.56296029065471,2.68577795450005,2.73572196891867,
2.74681664312659,2.74942953153049,2.75092662239325,2.75209028838396,2.75361256664475,
2.75626691324694,2.76663282861866,2.89765207232179,3.01540506199868,3.10413029830975,
3.11969968012748,3.12455575079131,3.12762226235055,3.13039514591027,3.13353090684597,
3.13992000122609,3.15489959781632,3.2387503322446,3.29730431605276,3.49307247223651,
3.5010405471248,3.5033702255634,3.50480406808172,3.5061071054925,3.5077551964859,
3.51040369774838,3.52370596033994,3.74780677769619,3.83375470821287,3.87399720222095,
3.89471535369585,3.8986551141331,3.90078571943595,3.90254130743241,3.90461426504689,
3.90819267942106,3.92175629212439,3.92611242701271,4.18472193881074,4.24569611785408,
4.30426635552552,4.31192408655437,4.31382892776188,4.31493854565035,4.31591604467966,
4.31713831127566,4.31902890203739,4.32764366944064,4.46092035292842,4.5860030993019,
4.64114574747391,4.68308640231368,4.70472185691645,4.70868771916486,4.71081361127814,
4.7124012303178,4.71413897389492,4.71722239298175,4.7263317306843,4.86088035479531,
4.9808557402363,5.07974238317828,5.10279583585837,5.10568588946089,5.10700354057489,
5.10802247424256,5.10912074299932,5.11085560287205,5.1163583990433,5.14832171989804,
5.19498872041594,5.34843151741666,5.4914573274337,5.50056617173629,5.50425602016166,
5.50639445823782,5.50820609593985,5.51040548387486,5.51447478919789,5.53593545284701,
5.57764565809867,5.69335417614501,5.73932978047868,5.79106841834415,5.79704213794616,
5.88710299665648,5.89293648269095,5.89480768164182,5.89583814499682,5.8968610469622,
5.89814341094205,5.90064554655125,5.917417671647,5.95724678085269,6.06865881566324,
6.26562322194229,6.27899833269172,6.28262774946748,6.28475201514421,6.28658169613875,
6.2888049579093,6.29298606283135,6.31661398042449,6.35908644372054,6.40676331601866,
6.48890429532695,6.57109364956328,6.67422177707237,6.68114943143726,6.68310097960942,
6.68414326941422,6.68504850002454,6.68616573584713,6.68806108720513,6.69035183626345,
6.69495640776353,6.74309228077589,6.85939758094755,7.06047579780178,7.07440238761392,
7.0779972087994,7.08006372959954,7.08164562436041,7.08368390545715,7.0872493771952,
7.10250905509153,7.27521357952129,7.40685581788151,7.42664699329201,7.43609456650022,
7.47177256101591,7.4749550738992,7.47622244352291,7.47714701563913,7.47813968857575,
7.47946069698554,7.48209105780349,7.48571292366267,7.51791370995304,7.58070347329138,
7.651120675881,7.72935355111975,7.87443180766461,7.88470691150223,7.88795956147616,
7.88974043937623,7.89133709218482,7.8934315626451,7.89720497949486,7.91513257216186,
7.94858233456759,8.01250701867857,8.04518093084793,8.06746826838991,8.07666828331565,
8.08514756286795,8.24409158714607,8.24937568939075,8.25298852654768,8.28038015810245,
8.28397846039894,8.28566266907478,8.28697065857906,8.28835756373514,8.29048447282631,
8.29300654727658,8.29775442611662,8.30899987232049,8.34497437531431,8.42743360480842,
8.60517709048041,8.65052731091322,8.65787307928605,8.66147492406709,8.6642970083782,
8.66739991386669,8.67242037805708,8.68946802306027,8.75152402116829,8.78755807143131,
8.81316434163601,8.83336111729128,8.85006462654123,8.8875679004826,8.98576628035345,
9.03282087370896,9.03698430486048,9.03865553493356,9.03987964687302,9.0411147379669,
9.04280756699977,9.04628535077753,9.05082977772171,9.06118002366665,9.08542244214113,
9.13110559744123,9.41322450409757,9.42992203620607,9.43343800885111,9.43568510058897,
9.43746498511733,9.43945720287359,9.4427717990269,9.45489497949568,9.53299488055051,
9.74268265674979,9.74993515641069,9.79522814704126,9.80157339631034,9.80832310078216,
9.81131441410182,9.81453324129582,9.8172532933142,9.81983574340087,9.82307430044125,
9.84510581793936,9.84793592067282,9.84922249928725,9.85020888203762,9.85127375306111,
9.85236422937948,9.85394563582332,9.85670926869068,9.95650252222412),
 .UNSPECIFIED.);
#509=B_SPLINE_CURVE_WITH_KNOTS('',3,(#55156,#55157,#55158,#55159,#55160,
#55161,#55162,#55163,#55164,#55165,#55166,#55167,#55168,#55169,#55170,#55171,
#55172,#55173,#55174,#55175,#55176,#55177,#55178,#55179,#55180,#55181,#55182,
#55183,#55184,#55185,#55186,#55187,#55188,#55189,#55190,#55191,#55192,#55193,
#55194,#55195,#55196,#55197,#55198,#55199,#55200,#55201,#55202,#55203,#55204,
#55205,#55206,#55207,#55208,#55209,#55210,#55211,#55212,#55213,#55214,#55215,
#55216,#55217,#55218,#55219,#55220,#55221,#55222,#55223,#55224,#55225,#55226,
#55227,#55228,#55229,#55230,#55231,#55232,#55233,#55234,#55235,#55236,#55237,
#55238,#55239,#55240,#55241,#55242,#55243,#55244,#55245,#55246,#55247,#55248,
#55249,#55250,#55251,#55252,#55253,#55254,#55255,#55256,#55257,#55258,#55259,
#55260,#55261,#55262,#55263,#55264,#55265,#55266,#55267,#55268,#55269,#55270,
#55271,#55272,#55273,#55274,#55275,#55276,#55277,#55278,#55279,#55280,#55281,
#55282,#55283,#55284,#55285,#55286,#55287,#55288,#55289,#55290,#55291,#55292,
#55293,#55294,#55295,#55296,#55297,#55298,#55299,#55300,#55301,#55302,#55303,
#55304,#55305,#55306,#55307,#55308,#55309,#55310,#55311,#55312,#55313,#55314,
#55315,#55316,#55317,#55318,#55319,#55320,#55321,#55322,#55323,#55324,#55325,
#55326,#55327,#55328,#55329,#55330,#55331,#55332,#55333,#55334,#55335,#55336,
#55337,#55338,#55339,#55340,#55341,#55342,#55343,#55344,#55345,#55346,#55347,
#55348,#55349,#55350,#55351,#55352,#55353,#55354,#55355,#55356,#55357,#55358,
#55359,#55360,#55361,#55362,#55363,#55364,#55365,#55366,#55367,#55368,#55369,
#55370,#55371,#55372,#55373,#55374,#55375,#55376,#55377,#55378,#55379,#55380,
#55381,#55382,#55383,#55384,#55385,#55386,#55387,#55388,#55389,#55390,#55391,
#55392,#55393,#55394,#55395,#55396,#55397,#55398,#55399,#55400,#55401,#55402,
#55403,#55404,#55405,#55406,#55407,#55408,#55409,#55410,#55411,#55412,#55413,
#55414,#55415,#55416,#55417,#55418,#55419,#55420),.UNSPECIFIED.,.F.,.F.,
(4,3,3,3,3,3,3,3,3,3,3,3,3,3,3,3,3,3,3,3,3,3,3,3,3,3,3,3,3,3,3,3,3,3,3,
3,3,3,3,3,3,3,3,3,3,3,3,3,3,3,3,3,3,3,3,3,3,3,3,3,3,3,3,3,3,3,3,3,3,3,3,
3,3,3,3,3,3,3,3,3,3,3,3,3,3,3,3,3,4),(-406.216115345406,-406.143347772459,
-406.070651068475,-405.998010215403,-405.925410253742,-405.8528277308,-405.780252578522,
-405.707671314702,-405.635070452466,-405.5623959866,-405.489683307801,-405.41686606389,
-405.353651268672,-405.279090207144,-405.204609979486,-405.130196672452,
-405.055836417014,-404.981515379383,-404.907219752434,-404.832923016735,
-404.758621687194,-404.684303273869,-404.609955280143,-404.53552816399,
-404.461055657197,-404.386486831737,-404.355243260621,-404.280682274487,
-404.206202110101,-404.131788854258,-404.057428637965,-403.983107627461,
-403.908812015639,-403.834515277131,-403.760213933595,-403.685895495086,
-403.611547464975,-403.53712029571,-403.462647726165,-403.388078823705,
-403.35683525257,-403.282941771316,-403.209130905174,-403.135388209751,
-403.061699290857,-402.988049793631,-402.914425392447,-402.840797545522,
-402.767163679453,-402.693510837238,-402.61982605303,-402.546055500133,
-402.472236789517,-402.39831213865,-402.35842724452,-402.283804179106,-402.209266850226,
-402.134801361473,-402.060393863831,-401.986030546589,-401.911697628688,
-401.837371166093,-401.763044834138,-401.688706175342,-401.614342728064,
-401.539907470881,-401.46543099749,-401.390864625349,-401.360019236469,
-401.281653562426,-401.203384392987,-401.12520644659,-401.047145674397,
-400.969156612141,-400.891256759144,-400.860815232443,-400.78290464433,
-400.704924247428,-400.626868917569,-400.548684201815,-400.470428822209,
-400.392054131574,-400.361611228418,-400.281649493689,-400.201825534484,
-400.122201686956,-400.042702288608,-399.963379286285,-399.933604772444),
 .UNSPECIFIED.);
#510=B_SPLINE_CURVE_WITH_KNOTS('',3,(#55422,#55423,#55424,#55425,#55426,
#55427,#55428,#55429,#55430,#55431,#55432,#55433,#55434,#55435,#55436,#55437,
#55438,#55439,#55440,#55441,#55442,#55443,#55444,#55445,#55446,#55447,#55448,
#55449,#55450,#55451,#55452,#55453,#55454,#55455,#55456,#55457,#55458,#55459,
#55460,#55461,#55462,#55463,#55464,#55465,#55466,#55467,#55468,#55469,#55470,
#55471,#55472,#55473,#55474,#55475,#55476,#55477,#55478,#55479,#55480,#55481,
#55482,#55483,#55484,#55485,#55486,#55487,#55488,#55489,#55490,#55491,#55492,
#55493,#55494,#55495,#55496,#55497,#55498,#55499,#55500,#55501,#55502,#55503,
#55504,#55505,#55506,#55507,#55508,#55509,#55510,#55511,#55512,#55513,#55514,
#55515,#55516,#55517,#55518,#55519,#55520,#55521,#55522,#55523,#55524,#55525,
#55526,#55527,#55528,#55529,#55530,#55531,#55532,#55533,#55534,#55535,#55536,
#55537,#55538,#55539,#55540,#55541,#55542,#55543,#55544,#55545,#55546,#55547,
#55548,#55549,#55550,#55551,#55552,#55553,#55554,#55555,#55556,#55557,#55558,
#55559,#55560,#55561,#55562,#55563,#55564,#55565,#55566,#55567,#55568,#55569,
#55570,#55571,#55572,#55573,#55574,#55575,#55576,#55577,#55578,#55579,#55580,
#55581,#55582,#55583,#55584,#55585,#55586,#55587,#55588,#55589,#55590,#55591,
#55592,#55593,#55594,#55595,#55596,#55597,#55598,#55599,#55600,#55601,#55602,
#55603,#55604,#55605,#55606,#55607,#55608,#55609,#55610,#55611,#55612,#55613,
#55614,#55615,#55616,#55617,#55618,#55619,#55620,#55621,#55622,#55623,#55624,
#55625,#55626,#55627,#55628,#55629,#55630,#55631,#55632,#55633,#55634,#55635,
#55636,#55637,#55638,#55639,#55640,#55641,#55642,#55643,#55644,#55645,#55646,
#55647,#55648,#55649,#55650,#55651,#55652,#55653),.UNSPECIFIED.,.F.,.F.,
(4,3,3,3,3,3,3,3,3,3,3,3,3,3,3,3,3,3,3,3,3,3,3,3,3,3,3,3,3,3,3,3,3,3,3,
3,3,3,3,3,3,3,3,3,3,3,3,3,3,3,3,3,3,3,3,3,3,3,3,3,3,3,3,3,3,3,3,3,3,3,3,
3,3,3,3,3,3,4),(-399.933604772444,-399.840724028374,-399.747275322167,-399.651442442894,
-399.558193843029,-399.461068824051,-399.363943805073,-399.272254036915,
-399.189836347056,-399.144188462362,-399.098687860549,-398.993531946425,
-398.88744788438,-398.78060582744,-398.673880337361,-398.568532952472,-398.466721211401,
-398.36490947033,-398.263770948654,-398.169261401944,-398.070080276303,
-397.968351387849,-397.865062762489,-397.76182249299,-397.661460916396,
-397.563608224494,-397.469619049145,-397.428854036759,-397.366376810785,
-397.269810333766,-397.1728740931,-397.075644374962,-397.011395580811,-396.923204173434,
-396.834237371584,-396.745961779209,-396.659945332695,-396.593937124864,
-396.499407545471,-396.40630905662,-396.368017440488,-396.274530703769,
-396.180063933608,-396.085912867677,-396.012055671754,-395.936942422972,
-395.861310605271,-395.78560057235,-395.759020212969,-395.681056354592,
-395.603177911801,-395.525486571131,-395.447574940006,-395.369663308881,
-395.292190873668,-395.215031932995,-395.17713875986,-395.106168378275,
-395.034791684364,-394.962843271554,-394.924103301075,-394.829321125232,
-394.734159677891,-394.638919242863,-394.543896244866,-394.449330934484,
-394.371456442117,-394.27823634382,-394.225892546488,-394.167925634083,
-394.110000407008,-394.08918638918,-393.995395485879,-393.900068996454,
-393.871945671379,-393.776560664005,-393.682731182159,-393.650419465264),
 .UNSPECIFIED.);
#511=B_SPLINE_CURVE_WITH_KNOTS('',3,(#55655,#55656,#55657,#55658,#55659,
#55660,#55661,#55662,#55663,#55664,#55665,#55666,#55667,#55668,#55669,#55670,
#55671,#55672,#55673,#55674,#55675,#55676,#55677,#55678,#55679,#55680,#55681,
#55682,#55683,#55684,#55685,#55686,#55687,#55688,#55689,#55690,#55691,#55692,
#55693,#55694,#55695,#55696,#55697,#55698,#55699,#55700,#55701,#55702,#55703,
#55704,#55705,#55706,#55707,#55708,#55709,#55710,#55711,#55712,#55713,#55714,
#55715,#55716,#55717,#55718,#55719,#55720,#55721,#55722,#55723,#55724,#55725,
#55726,#55727,#55728,#55729,#55730,#55731,#55732,#55733,#55734,#55735,#55736,
#55737,#55738,#55739,#55740,#55741,#55742,#55743,#55744,#55745,#55746,#55747,
#55748,#55749,#55750,#55751,#55752,#55753,#55754,#55755,#55756,#55757,#55758,
#55759,#55760,#55761,#55762,#55763,#55764,#55765,#55766,#55767,#55768,#55769,
#55770,#55771,#55772,#55773,#55774,#55775,#55776,#55777,#55778,#55779,#55780,
#55781,#55782,#55783,#55784,#55785,#55786,#55787,#55788,#55789,#55790,#55791,
#55792,#55793,#55794,#55795,#55796,#55797,#55798,#55799,#55800,#55801,#55802,
#55803,#55804,#55805,#55806,#55807,#55808,#55809,#55810,#55811,#55812,#55813,
#55814,#55815,#55816,#55817,#55818,#55819,#55820,#55821,#55822,#55823,#55824,
#55825,#55826,#55827,#55828,#55829,#55830,#55831,#55832,#55833,#55834,#55835,
#55836,#55837,#55838,#55839,#55840,#55841,#55842,#55843,#55844,#55845,#55846,
#55847,#55848,#55849,#55850,#55851,#55852,#55853,#55854,#55855,#55856,#55857,
#55858,#55859,#55860,#55861,#55862,#55863,#55864,#55865,#55866,#55867,#55868,
#55869,#55870,#55871,#55872,#55873,#55874,#55875,#55876,#55877,#55878,#55879,
#55880,#55881,#55882,#55883,#55884,#55885,#55886,#55887,#55888,#55889,#55890,
#55891,#55892,#55893,#55894,#55895,#55896,#55897,#55898,#55899,#55900,#55901,
#55902,#55903,#55904,#55905,#55906,#55907,#55908,#55909,#55910,#55911,#55912,
#55913,#55914,#55915,#55916,#55917,#55918,#55919,#55920,#55921,#55922,#55923,
#55924,#55925,#55926,#55927,#55928,#55929,#55930,#55931,#55932,#55933,#55934,
#55935,#55936,#55937,#55938,#55939,#55940,#55941,#55942,#55943,#55944,#55945,
#55946,#55947,#55948,#55949,#55950,#55951,#55952,#55953,#55954,#55955,#55956,
#55957,#55958,#55959,#55960,#55961,#55962,#55963,#55964,#55965,#55966,#55967,
#55968,#55969,#55970,#55971,#55972,#55973,#55974,#55975,#55976,#55977,#55978,
#55979,#55980,#55981,#55982,#55983,#55984,#55985,#55986,#55987,#55988,#55989,
#55990,#55991,#55992,#55993,#55994,#55995,#55996,#55997,#55998,#55999,#56000,
#56001,#56002,#56003,#56004,#56005,#56006,#56007,#56008,#56009,#56010,#56011,
#56012,#56013,#56014,#56015,#56016,#56017,#56018,#56019,#56020,#56021,#56022,
#56023,#56024,#56025,#56026,#56027,#56028,#56029,#56030,#56031,#56032,#56033,
#56034,#56035,#56036,#56037,#56038,#56039,#56040,#56041,#56042,#56043,#56044,
#56045,#56046,#56047,#56048,#56049,#56050,#56051,#56052,#56053,#56054,#56055,
#56056,#56057,#56058,#56059,#56060,#56061,#56062,#56063,#56064,#56065,#56066,
#56067,#56068,#56069,#56070,#56071,#56072,#56073,#56074,#56075,#56076,#56077,
#56078,#56079,#56080,#56081,#56082,#56083,#56084,#56085,#56086,#56087,#56088,
#56089,#56090,#56091,#56092,#56093,#56094,#56095,#56096,#56097,#56098,#56099,
#56100,#56101,#56102,#56103,#56104,#56105,#56106,#56107,#56108,#56109,#56110,
#56111,#56112,#56113,#56114,#56115,#56116,#56117,#56118,#56119,#56120,#56121,
#56122,#56123,#56124,#56125,#56126,#56127,#56128,#56129,#56130,#56131,#56132,
#56133,#56134,#56135,#56136,#56137,#56138,#56139,#56140,#56141,#56142,#56143,
#56144,#56145,#56146,#56147,#56148,#56149,#56150,#56151,#56152,#56153,#56154,
#56155,#56156,#56157,#56158,#56159,#56160,#56161,#56162,#56163,#56164,#56165,
#56166,#56167,#56168,#56169,#56170,#56171,#56172,#56173,#56174,#56175,#56176,
#56177,#56178,#56179,#56180,#56181,#56182,#56183,#56184,#56185,#56186,#56187,
#56188,#56189,#56190,#56191,#56192,#56193,#56194,#56195,#56196,#56197,#56198,
#56199,#56200,#56201,#56202,#56203,#56204,#56205,#56206,#56207,#56208,#56209,
#56210,#56211,#56212,#56213,#56214,#56215,#56216,#56217,#56218,#56219,#56220,
#56221,#56222,#56223,#56224,#56225,#56226,#56227,#56228,#56229,#56230,#56231,
#56232,#56233,#56234,#56235,#56236,#56237,#56238,#56239,#56240,#56241,#56242,
#56243,#56244),.UNSPECIFIED.,.F.,.F.,(4,2,2,2,2,2,2,2,2,2,2,2,2,2,2,2,2,
2,2,2,2,2,2,2,2,2,2,2,2,2,2,2,2,2,2,2,2,2,2,2,2,2,2,2,2,2,2,2,2,2,2,2,2,
2,2,2,2,2,2,2,2,2,2,2,2,2,2,2,2,2,2,2,2,2,2,2,2,2,2,2,2,2,2,2,2,2,2,2,2,
2,2,2,2,2,2,2,2,2,2,2,2,2,2,2,2,2,2,2,2,2,2,2,2,2,2,2,2,2,2,2,2,2,2,2,2,
2,2,2,2,2,2,2,2,2,2,2,2,2,2,2,2,2,2,2,2,2,2,2,2,2,2,2,2,2,2,2,2,2,2,2,2,
2,2,2,2,2,2,2,2,2,2,2,2,2,2,2,2,2,2,2,2,2,2,2,2,2,2,2,2,2,2,2,2,2,2,2,2,
2,2,2,2,2,2,2,2,2,2,2,2,2,2,2,2,2,2,2,2,2,2,2,2,2,2,2,2,2,2,2,2,2,2,2,2,
2,2,2,2,2,2,2,2,2,2,2,2,2,2,2,2,2,2,2,2,2,2,2,2,2,2,2,2,2,2,2,2,2,2,2,2,
2,2,2,2,2,2,2,2,2,2,2,2,2,2,2,2,2,2,2,2,2,2,2,2,2,4),(0.00126251356552906,
0.186225059591935,0.193990259317628,0.19760417431679,0.200513629682513,
0.202075751102413,0.203357019082192,0.204863069230799,0.207445693352058,
0.217043998252016,0.363438211244255,0.385024522634687,0.412253677348794,
0.463411052219837,0.589938340080337,0.595362951279272,0.597790581231296,
0.599596968016022,0.601278560374348,0.60358068419683,0.609349117916951,
0.673470367871833,0.815646411707306,0.850951794127492,0.883100220265274,
0.963169023255109,1.00316234601866,1.00941479613643,1.0111898642275,1.01227087534843,
1.01325421597341,1.01452547891397,1.01657474515715,1.02739808771365,1.19545040087695,
1.28545896032165,1.30012866446307,1.31921566201163,1.39961935540532,1.40518634575801,
1.40762792674758,1.40942523852921,1.41108462242251,1.41333526615407,1.41886827989882,
1.47516475895015,1.59923116554963,1.69608774112018,1.77531724775118,1.79240853360536,
1.80162765909149,1.80366953286933,1.80483324203958,1.80573882835393,1.8069250295385,
1.80899669625365,1.81777797401388,1.82144251627647,1.82694939923977,1.82768564840291,
1.8281272919608,1.82846786651528,1.82879097821014,1.82916813151138,1.97959339451667,
2.10481190919764,2.16856630786246,2.19695407305411,2.20134383698661,2.20361162585582,
2.20542782710451,2.20724670270543,2.21050818559859,2.22037974297078,2.37069746840366,
2.46801654513442,2.56231872042902,2.58041103267246,2.59013680425805,2.59228294034795,
2.59348923116391,2.59441703281646,2.59563059322422,2.59775137647423,2.60607319936642,
2.73929801363221,2.88638187638445,2.94784061656243,2.97551697690295,2.97987835971894,
2.98214016573425,2.98397267867294,2.98579897459387,2.98909752837871,2.99924785939877,
3.14531770463246,3.29548641033746,3.34214176984737,3.37410469665941,3.37960816752188,
3.38134334966396,3.38244184976096,3.38346101705703,3.38477899723267,3.38766988365334,
3.41073407474417,3.44353826910841,3.46033621650893,3.48689805699996,3.59984625278181,
3.69377985621534,3.74649184098769,3.77147094980812,3.77559627682108,3.77775641769902,
3.77934798960353,3.78106900517781,3.78406762974939,3.79257334228811,3.92214011435952,
4.08876382243618,4.16885607214697,4.17282109331017,4.17431925568893,4.17534357396199,
4.17634200162114,4.17755046195423,4.18060513669474,4.20944701402957,4.21008013036782,
4.21131496566917,4.21263018757763,4.21590635348096,4.22406982146714,4.23191199517075,
4.25921489352442,4.39448143441191,4.49878153598755,4.57899386313192,4.58466603679844,
4.58713836939801,4.58895236935687,4.59062299209048,4.59288254643806,4.59840607784595,
4.6531828280249,4.69205436451527,4.69627726121,4.72394140779277,4.90593207451306,
4.97864316905341,4.98239412207399,4.98410750791603,4.98542041403811,4.98682383866322,
4.98901660506026,4.99578648733437,5.0349271777167,5.09219180809043,5.33876318346483,
5.35359507428902,5.35854968084249,5.36132921066024,5.36411125609756,5.36756599164354,
5.37419198588687,5.41588391906643,5.51032462913216,5.60195616938288,5.65110888612536,
5.68822270573462,5.73191871970059,5.73600781058292,5.7376663761029,5.738887422315,
5.74020824652171,5.74199993481398,5.74607375590731,5.82727778891642,6.02621304286717,
6.03337671366783,6.06454240512269,6.12570791758827,6.1313948625272,6.13368270076109,
6.13536037415255,6.1371687624287,6.13961002527876,6.14498962286527,6.1521777570633,
6.21763669954722,6.2537116853726,6.37703636536662,6.52067717600832,6.54385969572138,
6.54644599819678,6.54772689175005,6.54865235206963,6.54964535379951,6.55098124091396,
6.55397118779999,6.62022197992257,6.72685954668408,6.87584332601442,6.88227289479219,
6.93579800087975,6.94125595077556,6.94349319513139,6.94514899073363,6.9469485092749,
6.94935474901434,6.9547594861787,6.96201258104655,7.02903448389256,7.14691191469804,
7.27480465632261,7.33517892825819,7.33883721822377,7.34019468783558,7.34116201489244,
7.34207784751574,7.34335428844533,7.3459096666313,7.36561724102622,7.45243821239467,
7.62550618070714,7.67417071886145,7.73084580485863,7.73654600221541,7.73887723907269,
7.74060068810342,7.74247190382012,7.74497089728739,7.75057061015039,7.7908098537416,
7.85992648875509,7.93703573742161,7.99171721680425,8.10653411768252,8.12498075648566,
8.12778318624607,8.1291263341347,8.13016503574707,8.13131385358631,8.13320261284503,
8.13987331763765,8.18297928745175,8.29028902764492,8.39675307603804,8.45614085496303,
8.47734992691092,8.51028366880833,8.51526937847719,8.51763204860301,8.51947969075598,
8.52149221508219,8.52355508731986,8.5300520652502,8.58940030098077,8.6778791210809,
8.90114226955788,8.91417096930859,8.91639817338624,8.9177296525736,8.91875087812554,
8.91984346061239,8.9215576849172,8.9270960936443,8.95988641600577,9.02854047039999,
9.10066765360362,9.13741325629974,9.18282148614484,9.23334694231122,9.23651186310549,
9.30452298112913,9.31033940470826,9.3126387099953,9.31431054129882,9.31609919802679,
9.31785429841102,9.32016630842972,9.33048866102472,9.4142135474803,9.46108141916866,
9.69379765100659,9.70707939134416,9.70927339045581,9.71057395287453,9.71156500734078,
9.71262237429131,9.71429050094163,9.71957287421535,9.75009918684513,9.95560876709398),
 .UNSPECIFIED.);
#512=B_SPLINE_CURVE_WITH_KNOTS('',3,(#56246,#56247,#56248,#56249,#56250,
#56251,#56252,#56253,#56254,#56255,#56256,#56257,#56258,#56259,#56260,#56261,
#56262,#56263),.UNSPECIFIED.,.F.,.F.,(4,2,2,2,2,2,2,2,4),(-381.084048850905,
-380.24913193901,-379.414215027115,-378.579298115221,-377.744381203326,
-376.909464291431,-376.074547379536,-375.239630467641,-374.800863543726),
 .UNSPECIFIED.);
#513=B_SPLINE_CURVE_WITH_KNOTS('',3,(#56265,#56266,#56267,#56268,#56269,
#56270,#56271,#56272,#56273,#56274,#56275,#56276,#56277,#56278,#56279,#56280,
#56281,#56282,#56283,#56284,#56285,#56286,#56287,#56288,#56289,#56290,#56291,
#56292,#56293,#56294,#56295,#56296,#56297,#56298,#56299,#56300,#56301,#56302,
#56303,#56304,#56305,#56306,#56307,#56308,#56309,#56310,#56311,#56312,#56313,
#56314,#56315,#56316,#56317,#56318,#56319,#56320,#56321,#56322,#56323,#56324,
#56325,#56326,#56327,#56328,#56329,#56330,#56331,#56332,#56333,#56334,#56335,
#56336,#56337,#56338,#56339,#56340,#56341,#56342,#56343,#56344,#56345,#56346,
#56347,#56348,#56349,#56350,#56351,#56352,#56353,#56354,#56355,#56356,#56357,
#56358,#56359,#56360,#56361,#56362,#56363,#56364,#56365,#56366,#56367,#56368,
#56369,#56370,#56371,#56372,#56373,#56374,#56375,#56376,#56377,#56378,#56379,
#56380,#56381,#56382,#56383,#56384,#56385,#56386,#56387,#56388,#56389,#56390,
#56391,#56392,#56393,#56394,#56395,#56396,#56397,#56398,#56399,#56400,#56401,
#56402,#56403,#56404,#56405,#56406,#56407,#56408,#56409,#56410,#56411,#56412,
#56413,#56414,#56415,#56416,#56417,#56418,#56419,#56420,#56421,#56422,#56423,
#56424,#56425,#56426,#56427,#56428,#56429,#56430,#56431,#56432,#56433,#56434,
#56435,#56436,#56437,#56438,#56439,#56440,#56441,#56442,#56443,#56444,#56445,
#56446,#56447,#56448,#56449,#56450,#56451,#56452,#56453,#56454,#56455,#56456,
#56457,#56458,#56459,#56460,#56461,#56462,#56463,#56464,#56465,#56466,#56467,
#56468,#56469,#56470,#56471,#56472,#56473,#56474,#56475,#56476,#56477,#56478,
#56479,#56480,#56481,#56482,#56483,#56484,#56485,#56486,#56487,#56488,#56489,
#56490,#56491,#56492,#56493,#56494,#56495,#56496,#56497,#56498,#56499,#56500,
#56501,#56502,#56503,#56504,#56505,#56506,#56507,#56508,#56509,#56510,#56511,
#56512,#56513,#56514,#56515,#56516,#56517,#56518,#56519,#56520,#56521,#56522,
#56523,#56524,#56525,#56526,#56527,#56528,#56529),.UNSPECIFIED.,.F.,.F.,
(4,3,3,3,3,3,3,3,3,3,3,3,3,3,3,3,3,3,3,3,3,3,3,3,3,3,3,3,3,3,3,3,3,3,3,
3,3,3,3,3,3,3,3,3,3,3,3,3,3,3,3,3,3,3,3,3,3,3,3,3,3,3,3,3,3,3,3,3,3,3,3,
3,3,3,3,3,3,3,3,3,3,3,3,3,3,3,3,3,4),(-374.800863543726,-374.719546014481,
-374.637804672318,-374.555849675824,-374.473567339188,-374.403003019094,
-374.32837995368,-374.2538426248,-374.179377136047,-374.104969638405,-374.030606321163,
-373.956273403262,-373.881946940668,-373.807620608713,-373.733281949916,
-373.658918502638,-373.584483245456,-373.510006772065,-373.435440399924,
-373.404595011043,-373.326229337001,-373.247960167562,-373.169782221164,
-373.091721448973,-373.013732386718,-372.935832533722,-372.905391007017,
-372.827480418904,-372.749500022002,-372.671444692142,-372.593259976388,
-372.515004596782,-372.436629906146,-372.406187002992,-372.331627906465,
-372.257144256853,-372.182722193748,-372.10834789731,-372.034007579519,
-371.959687475773,-371.885358606614,-371.811020373423,-371.736660315073,
-371.66226596127,-371.587785607698,-371.513255854697,-371.438624123855,
-371.407778994941,-371.333859208664,-371.260026233307,-371.186265607679,
-371.112562924151,-371.038903817516,-370.965273954686,-370.891646879009,
-370.818017649969,-370.744373312206,-370.670700903746,-370.596948576309,
-370.523151425474,-370.449253398825,-370.40937098689,-370.334809925361,
-370.260329697704,-370.18591639067,-370.111556135232,-370.0372350976,-369.962939470652,
-369.888642734953,-369.814341405412,-369.740022992087,-369.66567499836,
-369.591247882207,-369.516775375414,-369.442206549955,-369.410962978839,
-369.337414086104,-369.263945524044,-369.190542599154,-369.117190671653,
-369.042251617264,-368.968950350266,-368.895652939365,-368.822346207468,
-368.746179214737,-368.672781983367,-368.599343700407,-368.525824158253,
-368.517678236546),.UNSPECIFIED.);
#514=B_SPLINE_CURVE_WITH_KNOTS('',3,(#56531,#56532,#56533,#56534,#56535,
#56536,#56537,#56538,#56539,#56540,#56541,#56542,#56543,#56544,#56545,#56546,
#56547,#56548,#56549,#56550,#56551,#56552,#56553,#56554,#56555,#56556,#56557,
#56558,#56559,#56560,#56561,#56562,#56563,#56564,#56565,#56566,#56567,#56568,
#56569,#56570,#56571,#56572,#56573,#56574,#56575,#56576,#56577,#56578,#56579,
#56580,#56581,#56582,#56583,#56584,#56585,#56586,#56587,#56588,#56589,#56590,
#56591,#56592,#56593,#56594,#56595,#56596,#56597,#56598,#56599,#56600,#56601,
#56602,#56603,#56604,#56605,#56606,#56607,#56608,#56609,#56610,#56611,#56612,
#56613,#56614,#56615,#56616,#56617,#56618,#56619,#56620,#56621,#56622,#56623,
#56624,#56625,#56626,#56627,#56628,#56629,#56630,#56631,#56632,#56633,#56634,
#56635,#56636,#56637,#56638,#56639,#56640,#56641,#56642,#56643,#56644,#56645,
#56646,#56647,#56648,#56649,#56650,#56651,#56652,#56653,#56654,#56655,#56656,
#56657,#56658,#56659,#56660,#56661,#56662,#56663,#56664,#56665,#56666,#56667,
#56668,#56669,#56670,#56671,#56672,#56673,#56674,#56675,#56676,#56677,#56678,
#56679,#56680,#56681,#56682,#56683,#56684,#56685,#56686,#56687,#56688,#56689,
#56690,#56691,#56692,#56693,#56694,#56695,#56696,#56697,#56698,#56699,#56700,
#56701,#56702,#56703,#56704,#56705,#56706,#56707,#56708,#56709,#56710,#56711,
#56712,#56713,#56714,#56715,#56716,#56717,#56718,#56719,#56720,#56721,#56722,
#56723,#56724,#56725,#56726,#56727,#56728,#56729,#56730,#56731,#56732,#56733,
#56734,#56735,#56736,#56737,#56738,#56739,#56740,#56741,#56742,#56743,#56744,
#56745,#56746,#56747,#56748,#56749,#56750,#56751,#56752,#56753,#56754,#56755,
#56756,#56757,#56758,#56759,#56760,#56761,#56762,#56763,#56764,#56765,#56766,
#56767,#56768,#56769,#56770,#56771,#56772,#56773,#56774,#56775,#56776,#56777,
#56778,#56779,#56780,#56781,#56782,#56783,#56784,#56785,#56786,#56787,#56788,
#56789,#56790,#56791,#56792,#56793,#56794,#56795,#56796,#56797,#56798,#56799,
#56800,#56801,#56802,#56803,#56804,#56805,#56806,#56807,#56808,#56809,#56810,
#56811,#56812,#56813,#56814,#56815,#56816,#56817,#56818,#56819,#56820,#56821,
#56822,#56823,#56824,#56825,#56826,#56827,#56828,#56829,#56830,#56831,#56832,
#56833,#56834,#56835,#56836,#56837,#56838,#56839,#56840,#56841,#56842,#56843,
#56844,#56845,#56846,#56847,#56848,#56849,#56850,#56851,#56852,#56853,#56854,
#56855,#56856,#56857,#56858,#56859,#56860,#56861,#56862,#56863,#56864,#56865,
#56866,#56867,#56868,#56869,#56870,#56871,#56872,#56873,#56874,#56875,#56876,
#56877,#56878,#56879,#56880,#56881,#56882,#56883,#56884,#56885,#56886,#56887,
#56888,#56889,#56890,#56891,#56892,#56893,#56894,#56895,#56896,#56897,#56898,
#56899,#56900,#56901,#56902,#56903,#56904,#56905,#56906,#56907,#56908,#56909,
#56910,#56911,#56912,#56913,#56914,#56915,#56916,#56917,#56918,#56919,#56920,
#56921,#56922,#56923,#56924,#56925,#56926,#56927,#56928,#56929,#56930,#56931,
#56932,#56933,#56934,#56935,#56936,#56937,#56938,#56939,#56940,#56941,#56942,
#56943,#56944,#56945,#56946,#56947,#56948,#56949,#56950,#56951,#56952,#56953,
#56954,#56955,#56956,#56957,#56958,#56959,#56960,#56961,#56962,#56963,#56964,
#56965,#56966,#56967,#56968,#56969,#56970,#56971,#56972,#56973,#56974,#56975,
#56976,#56977,#56978,#56979,#56980,#56981,#56982,#56983,#56984,#56985,#56986,
#56987,#56988,#56989,#56990,#56991,#56992,#56993,#56994,#56995,#56996,#56997,
#56998,#56999,#57000,#57001,#57002,#57003,#57004,#57005,#57006,#57007,#57008,
#57009,#57010,#57011,#57012,#57013,#57014,#57015,#57016,#57017,#57018,#57019,
#57020,#57021,#57022,#57023,#57024,#57025,#57026,#57027,#57028,#57029,#57030,
#57031,#57032,#57033,#57034,#57035,#57036,#57037,#57038,#57039,#57040,#57041,
#57042,#57043,#57044,#57045,#57046,#57047,#57048,#57049,#57050,#57051,#57052,
#57053,#57054,#57055,#57056,#57057,#57058,#57059,#57060,#57061,#57062,#57063,
#57064,#57065,#57066,#57067,#57068,#57069,#57070,#57071,#57072,#57073,#57074,
#57075,#57076,#57077,#57078,#57079,#57080,#57081,#57082,#57083,#57084,#57085,
#57086,#57087,#57088,#57089,#57090,#57091,#57092,#57093,#57094,#57095,#57096,
#57097,#57098,#57099,#57100,#57101,#57102,#57103,#57104),.UNSPECIFIED.,
 .F.,.F.,(4,2,2,2,2,2,2,2,2,2,2,2,2,2,2,2,2,2,2,2,2,2,2,2,2,2,2,2,2,2,2,
2,2,2,2,2,2,2,2,2,2,2,2,2,2,2,2,2,2,2,2,2,2,2,2,2,2,2,2,2,2,2,2,2,2,2,2,
2,2,2,2,2,2,2,2,2,2,2,2,2,2,2,2,2,2,2,2,2,2,2,2,2,2,2,2,2,2,2,2,2,2,2,2,
2,2,2,2,2,2,2,2,2,2,2,2,2,2,2,2,2,2,2,2,2,2,2,2,2,2,2,2,2,2,2,2,2,2,2,2,
2,2,2,2,2,2,2,2,2,2,2,2,2,2,2,2,2,2,2,2,2,2,2,2,2,2,2,2,2,2,2,2,2,2,2,2,
2,2,2,2,2,2,2,2,2,2,2,2,2,2,2,2,2,2,2,2,2,2,2,2,2,2,2,2,2,2,2,2,2,2,2,2,
2,2,2,2,2,2,2,2,2,2,2,2,2,2,2,2,2,2,2,2,2,2,2,2,2,2,2,2,2,2,2,2,2,2,2,2,
2,2,2,2,2,2,2,2,2,2,2,2,2,2,2,2,2,2,2,2,2,2,2,2,2,2,2,2,2,2,2,2,2,2,2,2,
2,2,2,4),(0.00175903982440652,0.0619033949982958,0.0773251103339988,0.0793500364310013,
0.0806404128587861,0.0816337458300343,0.0826032683097308,0.0835626793958884,
0.0848899579511312,0.0883523287965929,0.13715083610504,0.157413074338618,
0.164171423162419,0.339089179933081,0.417864966959503,0.464742709937004,
0.47350788403339,0.476434200940765,0.478330286045617,0.480120734003368,
0.482481703792499,0.487750323666294,0.531505480165916,0.534036325308417,
0.540303918898397,0.545528498615362,0.562145795789653,0.780130183370125,
0.835391076207062,0.859452222108224,0.871355019724401,0.873545253277799,
0.874511497419455,0.875447174514417,0.876373425657873,0.877657157433084,
0.880254562304033,0.903782286123755,0.907724907334266,0.937361825917045,
0.948168304158819,1.02756118071958,1.03679852734077,1.04720568688562,1.05901661766314,
1.07253732293115,1.08819529895498,1.10663396019865,1.16988511765201,1.27926667323192,
1.28463039311485,1.28704670078533,1.28885109600663,1.29053551032943,1.29284879527928,
1.29868312701384,1.36607439219648,1.49035282391027,1.60717879828619,1.64604329211697,
1.66788418346017,1.67581966402046,1.67953857275252,1.68166549731746,1.68312526544564,
1.68452927587427,1.68580461329873,1.68746787804002,1.69086477157092,1.71162488274356,
1.84610989817839,2.04056119865127,2.05393970939231,2.05852490886575,2.06153214825909,
2.06438863731001,2.06815180312257,2.07654525239088,2.15045665748907,2.3221263790503,
2.38171141127265,2.41687348194745,2.42789281003331,2.43257060862904,2.43506600303702,
2.43667891686166,2.43818605243424,2.43942716000428,2.44093952712982,2.44354948377633,
2.4534205953433,2.59011544409689,2.68090675441139,2.73966728565225,2.81502691635214,
2.82907683762242,2.83256627392893,2.83459854643679,2.8363746279343,2.83856539076809,
2.84189738186162,2.85627590056278,2.8603892452858,3.13703601602355,3.20541644448914,
3.24039705374321,3.24420575138112,3.24619416785437,3.2478775302273,3.24892895054535,
3.24991464050417,3.25118042953033,3.2532565238506,3.26449720238799,3.44281498087408,
3.5522529640981,3.62823985548881,3.6401125495251,3.64338722574311,3.64536141320717,
3.64712899430856,3.64936570382018,3.65287525861323,3.66970782740594,3.95572751606245,
4.00264534326786,4.03440094833861,4.0398309353522,4.04153329595158,4.04262371744316,
4.04364663764598,4.04498566811218,4.04793243059222,4.07096687403263,4.07601931075552,
4.07801948007068,4.0832477480956,4.08871767295861,4.10029896442959,4.33481028609234,
4.4233746373646,4.43651076981224,4.43999197069271,4.44206254036525,4.44389882548904,
4.44619904581248,4.44976383328471,4.46614762519994,4.74400952150499,4.77572423849033,
4.82225795153851,4.82924474520577,4.83116587782632,4.83232247843113,4.83325197579703,
4.83452850708019,4.8364782614903,4.84499939117204,4.98069672908429,5.160018458876,
5.17487295770866,5.21314063518914,5.21835418281805,5.22076134320313,5.22261669443289,
5.22461075519972,5.22774900273032,5.23761755817871,5.42006113909995,5.60613756515104,
5.60839688187197,5.61806223719701,5.62007415904981,5.6213551636993,5.62236698397053,
5.62349644945202,5.62537809546184,5.63256420611471,5.6831709036341,5.73920533537026,
5.78748703504006,5.88912268771359,6.00592908500263,6.01346612221099,6.01631885317761,
6.01801161062242,6.01961320755682,6.02184384889773,6.02630544781578,6.06073129983565,
6.15390288875623,6.39004414485309,6.41061090996926,6.41339980704797,6.41468471264851,
6.41567369960073,6.41673882154944,6.41844018530934,6.42400253278825,6.4571395404516,
6.53159202589756,6.59237132618945,6.71768849745545,6.81773254002068,6.82440984208749,
6.82686140267966,6.82858365021243,6.83031193086043,6.83253688150836,6.83697302979643,
6.84264203086998,6.88715528697601,6.96510940595954,7.20692725140058,7.22076437161491,
7.22345093128765,7.22512950898651,7.22643411553023,7.22786889930314,7.23019835318589,
7.23814923026575,7.43340579013368,7.58605908205236,7.59624568242833,7.60005874858824,
7.60301523198508,7.60586806609863,7.60966441949961,7.61800433433649,7.80136421371316,
7.93302758586372,7.97373420887745,7.97783600506985,7.97945435497719,7.98066614718158,
7.98199698234236,7.98383866049691,7.98818978065292,8.09208681021082,8.18490874218475,
8.3150025855144,8.36800820606732,8.37303973938585,8.37546000281852,8.3771739963735,
8.37889618165677,8.38113941090526,8.38532662697681,8.39080289884384,8.40287658238937,
8.43746430230672,8.51477168194802,8.77353773155922,8.78740062702841,8.78983264510202,
8.79107295264083,8.79205234488855,8.7931548385238,8.79500399991749,8.80192305162432,
8.84930216261481,8.92330365192968,9.01454515107542,9.06891042081912,9.17661297365186,
9.18385459680458,9.18638021289148,9.18811494060852,9.18984723203075,9.19200841457564,
9.19434986416638,9.19808861922751,9.20532140466049,9.22289991172767,9.26823496600275,
9.3264499243663,9.56070762949262,9.58073970506991,9.58351779358425,9.58481628221867,
9.58583361657385,9.58694351643894,9.58872561496557,9.59462416432671,9.63031753343889,
9.67840012039954,9.96492602872158),.UNSPECIFIED.);
#515=B_SPLINE_CURVE_WITH_KNOTS('',3,(#57106,#57107,#57108,#57109,#57110,
#57111,#57112,#57113,#57114,#57115,#57116,#57117,#57118,#57119,#57120,#57121,
#57122,#57123),.UNSPECIFIED.,.F.,.F.,(4,2,2,2,2,2,2,2,4),(-355.951307622187,
-355.116390710292,-354.281473798397,-353.446556886502,-352.611639974607,
-351.776723062712,-350.941806150818,-350.106889238923,-349.668122315007),
 .UNSPECIFIED.);
#516=B_SPLINE_CURVE_WITH_KNOTS('',3,(#57125,#57126,#57127,#57128,#57129,
#57130,#57131,#57132,#57133,#57134,#57135,#57136,#57137,#57138,#57139,#57140,
#57141,#57142),.UNSPECIFIED.,.F.,.F.,(4,2,2,2,2,2,2,2,4),(-349.668122315007,
-348.833205403113,-347.998288491218,-347.163371579323,-346.328454667428,
-345.493537755533,-344.658620843639,-343.823703931744,-343.385155491413),
 .UNSPECIFIED.);
#517=B_SPLINE_CURVE_WITH_KNOTS('',3,(#57144,#57145,#57146,#57147,#57148,
#57149,#57150,#57151,#57152,#57153,#57154),.UNSPECIFIED.,.F.,.F.,(4,1,1,
1,1,1,1,1,4),(-343.384486891376,-342.453946761465,-341.455538753414,-340.457130745363,
-339.458722737312,-338.460314729261,-337.961110725235,-337.46190672121,
-337.101751700648),.UNSPECIFIED.);
#518=B_SPLINE_CURVE_WITH_KNOTS('',3,(#57156,#57157,#57158,#57159,#57160,
#57161,#57162,#57163,#57164,#57165,#57166,#57167,#57168,#57169,#57170,#57171,
#57172,#57173),.UNSPECIFIED.,.F.,.F.,(4,2,2,2,2,2,2,2,4),(-337.101751700648,
-336.266834788753,-335.431917876858,-334.597000964964,-333.762084053069,
-332.927167141174,-332.092250229279,-331.257333317384,-330.818566393469),
 .UNSPECIFIED.);
#519=B_SPLINE_CURVE_WITH_KNOTS('',3,(#57175,#57176,#57177,#57178,#57179,
#57180,#57181,#57182,#57183,#57184,#57185,#57186,#57187,#57188,#57189,#57190,
#57191,#57192,#57193,#57194,#57195,#57196,#57197,#57198,#57199,#57200,#57201,
#57202,#57203,#57204,#57205,#57206,#57207,#57208,#57209,#57210,#57211,#57212,
#57213,#57214,#57215,#57216,#57217,#57218,#57219,#57220,#57221,#57222,#57223,
#57224,#57225,#57226,#57227,#57228,#57229,#57230,#57231,#57232,#57233,#57234,
#57235,#57236,#57237,#57238,#57239,#57240,#57241,#57242,#57243,#57244,#57245,
#57246,#57247,#57248,#57249,#57250,#57251,#57252,#57253,#57254,#57255,#57256,
#57257,#57258,#57259,#57260,#57261,#57262,#57263,#57264,#57265,#57266,#57267,
#57268,#57269,#57270,#57271,#57272,#57273,#57274,#57275,#57276,#57277,#57278,
#57279,#57280,#57281,#57282,#57283,#57284,#57285,#57286,#57287,#57288,#57289,
#57290,#57291,#57292,#57293,#57294,#57295,#57296,#57297,#57298,#57299,#57300,
#57301,#57302,#57303,#57304,#57305,#57306,#57307,#57308,#57309,#57310,#57311,
#57312,#57313,#57314,#57315,#57316,#57317,#57318,#57319,#57320,#57321,#57322,
#57323,#57324,#57325,#57326,#57327,#57328,#57329,#57330,#57331,#57332,#57333,
#57334,#57335,#57336,#57337,#57338,#57339,#57340,#57341,#57342,#57343,#57344,
#57345,#57346,#57347,#57348,#57349,#57350,#57351,#57352,#57353,#57354,#57355,
#57356,#57357,#57358,#57359,#57360,#57361,#57362,#57363,#57364,#57365,#57366,
#57367,#57368,#57369,#57370,#57371,#57372,#57373,#57374,#57375,#57376,#57377,
#57378,#57379,#57380,#57381,#57382,#57383,#57384,#57385,#57386,#57387,#57388,
#57389,#57390,#57391,#57392,#57393,#57394,#57395,#57396,#57397,#57398,#57399,
#57400,#57401,#57402,#57403,#57404,#57405,#57406,#57407,#57408,#57409,#57410,
#57411,#57412,#57413,#57414,#57415,#57416,#57417,#57418,#57419,#57420,#57421,
#57422,#57423,#57424,#57425,#57426,#57427,#57428,#57429,#57430,#57431,#57432,
#57433,#57434,#57435,#57436),.UNSPECIFIED.,.F.,.F.,(4,3,3,3,3,3,3,3,3,3,
3,3,3,3,3,3,3,3,3,3,3,3,3,3,3,3,3,3,3,3,3,3,3,3,3,3,3,3,3,3,3,3,3,3,3,3,
3,3,3,3,3,3,3,3,3,3,3,3,3,3,3,3,3,3,3,3,3,3,3,3,3,3,3,3,3,3,3,3,3,3,3,3,
3,3,3,3,3,4),(-330.818566393469,-330.732187461315,-330.647974550361,-330.560512607607,
-330.473050664853,-330.398491568327,-330.324007918715,-330.249585855612,
-330.175211559175,-330.100871241385,-330.026551137639,-329.952222268481,
-329.877884035291,-329.803523976941,-329.72912962314,-329.654649269568,
-329.580119516568,-329.505487785727,-329.474642656803,-329.400722870526,
-329.326889895169,-329.253129269541,-329.179426586013,-329.105767479378,
-329.032137616548,-328.958510540871,-328.884881311831,-328.811236974068,
-328.737564565608,-328.663812238171,-328.590015087337,-328.516117060688,
-328.476234648752,-328.401673587223,-328.327193359566,-328.252780052532,
-328.178419797093,-328.104098759462,-328.029803132513,-327.955506396813,
-327.881205067272,-327.806886653947,-327.732538660221,-327.658111544067,
-327.583639037274,-327.509070211814,-327.477826640701,-327.403265654567,
-327.328785490181,-327.254372234338,-327.180012018046,-327.105691007541,
-327.03139539572,-326.957098657212,-326.882797313677,-326.808478875168,
-326.734130845056,-326.659703675792,-326.585231106247,-326.510662203788,
-326.47941863265,-326.405525151396,-326.331714285254,-326.257971589831,
-326.184282670936,-326.110633173709,-326.037008772525,-325.963380925599,
-325.889747059531,-325.816094217316,-325.742409433107,-325.668638880209,
-325.594820169594,-325.520895518727,-325.481010624599,-325.406897287707,
-325.332869248636,-325.258912171831,-325.185011772281,-325.11115380508,
-325.037318033266,-324.963492534632,-324.889664458657,-324.815820955436,
-324.741913564608,-324.667972525697,-324.593939371745,-324.535655273961),
 .UNSPECIFIED.);
#520=B_SPLINE_CURVE_WITH_KNOTS('',3,(#57438,#57439,#57440,#57441,#57442,
#57443,#57444,#57445,#57446,#57447,#57448,#57449,#57450,#57451,#57452,#57453,
#57454,#57455,#57456,#57457,#57458,#57459,#57460,#57461,#57462,#57463,#57464,
#57465,#57466,#57467,#57468,#57469,#57470,#57471,#57472,#57473,#57474,#57475,
#57476,#57477,#57478,#57479,#57480,#57481,#57482,#57483,#57484,#57485,#57486,
#57487,#57488,#57489,#57490,#57491,#57492,#57493,#57494,#57495,#57496,#57497,
#57498,#57499,#57500,#57501,#57502,#57503,#57504,#57505,#57506,#57507,#57508,
#57509,#57510,#57511,#57512,#57513,#57514,#57515,#57516,#57517,#57518,#57519,
#57520,#57521,#57522,#57523,#57524,#57525,#57526,#57527,#57528,#57529,#57530,
#57531,#57532,#57533,#57534,#57535,#57536,#57537,#57538,#57539,#57540,#57541,
#57542,#57543,#57544,#57545,#57546,#57547,#57548,#57549,#57550,#57551,#57552,
#57553,#57554,#57555,#57556,#57557,#57558,#57559,#57560,#57561,#57562,#57563,
#57564,#57565,#57566,#57567,#57568,#57569,#57570,#57571,#57572,#57573,#57574,
#57575,#57576,#57577,#57578,#57579,#57580,#57581,#57582,#57583,#57584,#57585,
#57586,#57587,#57588,#57589,#57590,#57591,#57592,#57593,#57594,#57595,#57596,
#57597,#57598,#57599,#57600,#57601,#57602,#57603,#57604,#57605,#57606,#57607,
#57608,#57609,#57610,#57611,#57612,#57613,#57614,#57615,#57616,#57617,#57618,
#57619,#57620,#57621,#57622,#57623,#57624,#57625,#57626,#57627,#57628,#57629,
#57630,#57631,#57632,#57633,#57634,#57635,#57636,#57637,#57638,#57639,#57640,
#57641,#57642,#57643,#57644,#57645,#57646,#57647,#57648,#57649,#57650,#57651,
#57652,#57653,#57654,#57655,#57656,#57657,#57658,#57659,#57660,#57661,#57662,
#57663,#57664,#57665,#57666,#57667,#57668,#57669,#57670,#57671,#57672,#57673,
#57674,#57675,#57676,#57677,#57678,#57679,#57680,#57681,#57682,#57683,#57684,
#57685,#57686,#57687,#57688,#57689,#57690,#57691,#57692,#57693,#57694,#57695,
#57696,#57697,#57698,#57699,#57700,#57701,#57702,#57703,#57704,#57705,#57706,
#57707,#57708,#57709,#57710,#57711,#57712,#57713,#57714,#57715,#57716,#57717,
#57718,#57719,#57720,#57721,#57722,#57723,#57724,#57725,#57726,#57727,#57728,
#57729,#57730,#57731,#57732,#57733,#57734,#57735,#57736,#57737,#57738,#57739,
#57740,#57741,#57742,#57743,#57744,#57745,#57746,#57747,#57748,#57749,#57750,
#57751,#57752,#57753,#57754,#57755,#57756,#57757,#57758,#57759,#57760,#57761,
#57762,#57763,#57764,#57765,#57766,#57767,#57768,#57769,#57770,#57771,#57772,
#57773,#57774,#57775,#57776,#57777,#57778,#57779,#57780,#57781,#57782,#57783,
#57784,#57785,#57786,#57787,#57788,#57789,#57790,#57791,#57792,#57793,#57794,
#57795,#57796,#57797,#57798,#57799,#57800,#57801,#57802,#57803,#57804,#57805,
#57806,#57807,#57808,#57809,#57810,#57811,#57812,#57813,#57814,#57815,#57816,
#57817,#57818,#57819,#57820,#57821,#57822,#57823,#57824,#57825,#57826,#57827,
#57828,#57829,#57830,#57831,#57832,#57833,#57834,#57835,#57836,#57837,#57838,
#57839,#57840,#57841,#57842,#57843,#57844,#57845,#57846,#57847,#57848,#57849,
#57850,#57851,#57852,#57853,#57854,#57855,#57856,#57857,#57858,#57859,#57860,
#57861,#57862,#57863,#57864,#57865,#57866,#57867,#57868,#57869,#57870,#57871,
#57872,#57873,#57874,#57875,#57876,#57877,#57878,#57879,#57880,#57881,#57882,
#57883,#57884,#57885,#57886,#57887,#57888,#57889,#57890,#57891,#57892,#57893,
#57894,#57895,#57896,#57897,#57898,#57899,#57900,#57901,#57902,#57903,#57904,
#57905,#57906,#57907,#57908,#57909,#57910,#57911,#57912,#57913,#57914,#57915,
#57916,#57917,#57918,#57919,#57920,#57921,#57922,#57923,#57924,#57925,#57926,
#57927,#57928,#57929,#57930,#57931,#57932,#57933,#57934,#57935,#57936,#57937,
#57938,#57939,#57940,#57941,#57942,#57943,#57944,#57945,#57946,#57947,#57948,
#57949,#57950,#57951,#57952,#57953,#57954,#57955,#57956,#57957,#57958,#57959,
#57960,#57961,#57962,#57963,#57964,#57965,#57966,#57967,#57968,#57969,#57970,
#57971,#57972,#57973,#57974,#57975,#57976,#57977,#57978,#57979,#57980,#57981,
#57982,#57983,#57984,#57985,#57986,#57987,#57988,#57989,#57990,#57991,#57992,
#57993,#57994,#57995,#57996,#57997,#57998,#57999,#58000,#58001,#58002,#58003,
#58004,#58005,#58006,#58007,#58008,#58009,#58010,#58011,#58012,#58013,#58014,
#58015,#58016,#58017,#58018,#58019,#58020,#58021,#58022,#58023,#58024,#58025,
#58026,#58027,#58028,#58029,#58030,#58031,#58032,#58033,#58034,#58035,#58036,
#58037,#58038,#58039,#58040,#58041),.UNSPECIFIED.,.F.,.F.,(4,2,2,2,2,2,
2,2,2,2,2,2,2,2,2,2,2,2,2,2,2,2,2,2,2,2,2,2,2,2,2,2,2,2,2,2,2,2,2,2,2,2,
2,2,2,2,2,2,2,2,2,2,2,2,2,2,2,2,2,2,2,2,2,2,2,2,2,2,2,2,2,2,2,2,2,2,2,2,
2,2,2,2,2,2,2,2,2,2,2,2,2,2,2,2,2,2,2,2,2,2,2,2,2,2,2,2,2,2,2,2,2,2,2,2,
2,2,2,2,2,2,2,2,2,2,2,2,2,2,2,2,2,2,2,2,2,2,2,2,2,2,2,2,2,2,2,2,2,2,2,2,
2,2,2,2,2,2,2,2,2,2,2,2,2,2,2,2,2,2,2,2,2,2,2,2,2,2,2,2,2,2,2,2,2,2,2,2,
2,2,2,2,2,2,2,2,2,2,2,2,2,2,2,2,2,2,2,2,2,2,2,2,2,2,2,2,2,2,2,2,2,2,2,2,
2,2,2,2,2,2,2,2,2,2,2,2,2,2,2,2,2,2,2,2,2,2,2,2,2,2,2,2,2,2,2,2,2,2,2,2,
2,2,2,2,2,2,2,2,2,2,2,2,2,2,2,2,2,2,2,2,2,2,2,2,2,2,2,2,2,2,2,2,2,2,2,2,
2,2,2,2,2,2,2,4),(0.00136622398944564,0.0549836364701191,0.0575959087568496,
0.0592608135368877,0.0605382522441885,0.0617743502663625,0.0629998489473684,
0.0646756916742249,0.0688645621889766,0.117084529607065,0.122773462059413,
0.131153634355164,0.286044438208657,0.416698022472885,0.430356651377554,
0.434978118346523,0.437992946900742,0.440845169366185,0.444585637914629,
0.450889687103354,0.489749078850845,0.678371606139728,0.715457827701584,
0.760840216312113,0.794122201000565,0.804664488038609,0.809191877773913,
0.812650380643149,0.814320638478753,0.815567921817461,0.816801443060079,
0.818508273664927,0.821943405844319,0.857651705652357,0.864479611526515,
0.949966848352646,0.95910782349341,0.969254789920635,0.980633977839693,
0.993514584864171,1.00825465634677,1.02537115364427,1.08927684796378,1.14284207435874,
1.18362711403943,1.20458526833659,1.20853892283229,1.21067288315403,1.21242906244085,
1.21450016788585,1.21806911105161,1.23153069266861,1.2362757338985,1.49769581269447,
1.57066913504191,1.60142769380722,1.61446364800677,1.62194620323438,1.62383802512198,
1.62476978795356,1.62565040248645,1.6266121987789,1.62831307267665,1.63329999502228,
1.71295078896719,1.71418957342121,1.71541308076413,1.8497374604961,1.86952998751965,
1.89339093147479,1.92900566308549,1.98784532404182,2.01445110218426,2.0186448123843,
2.0208194381931,2.02256497192871,2.02431636472182,2.02746582337276,2.03705831081284,
2.17538338123192,2.2501173478525,2.32373024868085,2.38301787396716,2.40360973903664,
2.41056452709298,2.41367113400105,2.41609819913882,2.41733147041691,2.41824578572452,
2.41921866868889,2.42059477541822,2.42346414283281,2.45399887021593,2.45659144852119,
2.46171223807594,2.46735964086411,2.49994789575026,2.70620281969758,2.79800967133651,
2.81137728312264,2.81487888535627,2.8169535903507,2.81878857839893,2.82108061743515,
2.82462037436985,2.84069759150573,3.08851743177993,3.15465042485733,3.19724728495318,
3.20162231904173,3.20385802729046,3.20573937989056,3.20687343205009,3.2079105908883,
3.20923885952927,3.21135672789564,3.2221000053344,3.39602945880976,3.57417923007587,
3.59008530784042,3.59379763156706,3.5959193330896,3.59756573602103,3.59943285089433,
3.60293355083198,3.61472892441595,3.78405069555577,3.90958447925468,3.9558138625686,
3.98760663077307,3.99309194459957,3.99482503010733,3.99592310314843,3.99694249903544,
3.99826165531829,4.00115883574194,4.02439597057315,4.02960656921686,4.26303270142273,
4.31796713796737,4.37698536162458,4.38713644308349,4.39022951490476,4.39216262995934,
4.39393925279675,4.39621366149945,4.39992804579904,4.40943918638269,4.56584757678512,
4.71857283327626,4.78398178686849,4.78696839442891,4.78830369079372,4.789296614296,
4.79022226772311,4.79150384800621,4.794092828011,4.8173582560741,4.82158581797852,
4.97965523899293,5.04492006435551,5.18681921727791,5.19681175350678,5.20002885019111,
5.2018028506433,5.20357820608608,5.20576248821886,5.20995259080822,5.23586466223165,
5.2920027714497,5.45318364419068,5.58514695881448,5.59431102188089,5.59684829061204,
5.5983435640978,5.59963758623534,5.60121759023072,5.60421174616796,5.62171113723449,
5.65857146842216,5.73879280155077,5.81441968449108,5.95952002348252,5.96884073603031,
5.97251220589428,5.97518045712044,5.97802485511338,5.98178156826293,5.98992144889064,
6.13176725819743,6.32677201448762,6.34678635488243,6.35010334537974,6.35177334704772,
6.35307580732724,6.35451281960426,6.35685617663271,6.36495066419743,6.41383363022294,
6.52942198157384,6.68100534345652,6.7393630837497,6.74497997674114,6.74725575642469,
6.74893041267137,6.75070487577116,6.7530877507837,6.75573102537095,6.76017892325509,
6.86177418736654,7.09448149964857,7.15640282301169,7.16015983454559,7.16151563532281,
7.16246111029065,7.16334629923613,7.16456855205924,7.16697430236636,7.18384376998072,
7.26144323897518,7.38021574846885,7.45359341050738,7.54845133480444,7.55479333226655,
7.55717946658029,7.55887459186821,7.56061637997025,7.56273655802658,7.56513975324901,
7.56902744471967,7.57665887900283,7.64967118996528,7.75679329987061,7.93993301467533,
7.9457540224234,7.95218578688714,7.95407799716185,7.95509618311438,7.9560932114186,
7.95730943038514,7.95957618455766,7.97186221326425,7.99667471615725,8.04469830972115,
8.06734237235833,8.0848381807374,8.12548588831923,8.13470375109014,8.14338038425575,
8.15158103720518,8.1593586919536,8.2692530898096,8.34433037548595,8.35046734830483,
8.35308804001049,8.35495251093868,8.35682064337513,8.35871488630855,8.36369865466696,
8.41508239995064,8.50948338263502,8.71465462538405,8.7391166583074,8.74212183058371,
8.74338626291622,8.74444025812886,8.74552948658939,8.74714718567329,8.75157568685505,
8.85833700198782,8.88400487569615,8.90543087084854,8.98081582127137,9.02742663224101,
9.12254138325966,9.12903743372827,9.13172278728915,9.13360111154788,9.1354565067724,
9.13804303010381,9.14427691528408,9.26741577166684,9.48091372007006,9.52736250495282,
9.53085492284987,9.53219854562552,9.53316282357872,9.53408084640659,9.53536843485012,
9.53801825382757,9.56409286876191,9.64588370684354,9.89942030683067,9.90961703703559,
9.92357694107525,9.9271762621359,9.92924454040451,9.93084517391125,9.93250872590421,
9.93451244944676,9.93745080181594,9.9580269971825),.UNSPECIFIED.);
#521=B_SPLINE_CURVE_WITH_KNOTS('',3,(#58043,#58044,#58045,#58046,#58047,
#58048,#58049,#58050,#58051,#58052,#58053,#58054,#58055,#58056,#58057,#58058,
#58059,#58060,#58061,#58062,#58063,#58064,#58065,#58066,#58067,#58068,#58069,
#58070,#58071,#58072,#58073,#58074,#58075,#58076,#58077,#58078,#58079,#58080,
#58081,#58082,#58083,#58084,#58085,#58086,#58087,#58088,#58089,#58090,#58091,
#58092,#58093,#58094,#58095,#58096,#58097,#58098,#58099,#58100,#58101,#58102,
#58103,#58104,#58105,#58106,#58107,#58108,#58109,#58110,#58111,#58112,#58113,
#58114,#58115,#58116,#58117,#58118,#58119,#58120,#58121,#58122,#58123,#58124,
#58125,#58126,#58127,#58128,#58129,#58130,#58131,#58132,#58133,#58134,#58135,
#58136,#58137,#58138,#58139,#58140,#58141,#58142,#58143,#58144,#58145,#58146,
#58147,#58148,#58149,#58150,#58151,#58152,#58153,#58154,#58155,#58156,#58157,
#58158,#58159,#58160,#58161,#58162,#58163,#58164,#58165,#58166,#58167,#58168,
#58169,#58170,#58171,#58172,#58173,#58174,#58175,#58176,#58177,#58178,#58179,
#58180,#58181,#58182,#58183,#58184,#58185,#58186,#58187,#58188,#58189,#58190,
#58191,#58192,#58193,#58194,#58195,#58196,#58197,#58198,#58199,#58200,#58201,
#58202,#58203,#58204,#58205,#58206,#58207,#58208,#58209,#58210,#58211,#58212,
#58213,#58214,#58215,#58216,#58217,#58218,#58219,#58220,#58221,#58222,#58223,
#58224,#58225,#58226,#58227,#58228,#58229,#58230,#58231,#58232,#58233,#58234,
#58235,#58236,#58237,#58238,#58239,#58240,#58241,#58242,#58243,#58244,#58245,
#58246,#58247,#58248,#58249,#58250,#58251,#58252,#58253,#58254,#58255,#58256,
#58257,#58258,#58259,#58260,#58261,#58262,#58263,#58264,#58265,#58266,#58267,
#58268,#58269,#58270,#58271,#58272,#58273,#58274,#58275,#58276,#58277,#58278,
#58279,#58280,#58281,#58282,#58283,#58284,#58285,#58286,#58287,#58288,#58289,
#58290,#58291,#58292,#58293,#58294,#58295,#58296,#58297,#58298,#58299,#58300,
#58301,#58302,#58303,#58304,#58305,#58306,#58307,#58308,#58309,#58310,#58311,
#58312,#58313,#58314,#58315,#58316,#58317,#58318,#58319,#58320,#58321,#58322,
#58323,#58324,#58325,#58326,#58327,#58328,#58329,#58330,#58331,#58332,#58333,
#58334,#58335,#58336,#58337,#58338,#58339,#58340,#58341,#58342,#58343,#58344,
#58345,#58346,#58347,#58348,#58349,#58350,#58351,#58352,#58353,#58354,#58355,
#58356,#58357,#58358,#58359,#58360,#58361,#58362,#58363,#58364,#58365,#58366,
#58367,#58368,#58369,#58370,#58371,#58372,#58373,#58374,#58375,#58376,#58377,
#58378,#58379,#58380,#58381,#58382,#58383,#58384,#58385,#58386,#58387,#58388,
#58389,#58390,#58391,#58392,#58393,#58394,#58395,#58396,#58397,#58398,#58399,
#58400,#58401,#58402,#58403,#58404,#58405,#58406,#58407,#58408,#58409,#58410,
#58411,#58412,#58413,#58414,#58415,#58416,#58417,#58418,#58419,#58420,#58421,
#58422,#58423,#58424,#58425,#58426,#58427,#58428,#58429,#58430,#58431,#58432,
#58433,#58434,#58435,#58436,#58437,#58438,#58439,#58440,#58441,#58442,#58443,
#58444,#58445,#58446,#58447,#58448,#58449,#58450,#58451,#58452,#58453,#58454,
#58455,#58456,#58457,#58458,#58459,#58460,#58461,#58462,#58463,#58464,#58465,
#58466,#58467,#58468,#58469,#58470,#58471,#58472,#58473,#58474,#58475,#58476,
#58477,#58478,#58479,#58480,#58481,#58482,#58483,#58484,#58485,#58486,#58487,
#58488,#58489,#58490,#58491,#58492,#58493,#58494,#58495,#58496,#58497,#58498,
#58499,#58500,#58501,#58502,#58503,#58504,#58505,#58506,#58507,#58508,#58509,
#58510,#58511,#58512,#58513,#58514,#58515,#58516,#58517,#58518,#58519,#58520,
#58521,#58522,#58523,#58524,#58525,#58526,#58527,#58528,#58529,#58530,#58531,
#58532,#58533,#58534,#58535,#58536,#58537,#58538,#58539,#58540,#58541,#58542,
#58543,#58544,#58545,#58546,#58547,#58548,#58549,#58550,#58551,#58552,#58553,
#58554,#58555,#58556,#58557,#58558,#58559,#58560,#58561,#58562,#58563,#58564,
#58565,#58566,#58567,#58568,#58569,#58570,#58571,#58572,#58573,#58574,#58575,
#58576,#58577,#58578,#58579,#58580,#58581,#58582,#58583,#58584,#58585,#58586,
#58587,#58588,#58589,#58590,#58591,#58592,#58593,#58594,#58595,#58596,#58597,
#58598,#58599,#58600,#58601,#58602,#58603,#58604,#58605,#58606,#58607,#58608,
#58609,#58610,#58611,#58612,#58613,#58614,#58615,#58616,#58617,#58618,#58619,
#58620,#58621,#58622,#58623,#58624,#58625,#58626,#58627,#58628,#58629,#58630,
#58631,#58632,#58633,#58634,#58635,#58636,#58637,#58638,#58639,#58640,#58641,
#58642),.UNSPECIFIED.,.F.,.F.,(4,2,2,2,2,2,2,2,2,2,2,2,2,2,2,2,2,2,2,2,
2,2,2,2,2,2,2,2,2,2,2,2,2,2,2,2,2,2,2,2,2,2,2,2,2,2,2,2,2,2,2,2,2,2,2,2,
2,2,2,2,2,2,2,2,2,2,2,2,2,2,2,2,2,2,2,2,2,2,2,2,2,2,2,2,2,2,2,2,2,2,2,2,
2,2,2,2,2,2,2,2,2,2,2,2,2,2,2,2,2,2,2,2,2,2,2,2,2,2,2,2,2,2,2,2,2,2,2,2,
2,2,2,2,2,2,2,2,2,2,2,2,2,2,2,2,2,2,2,2,2,2,2,2,2,2,2,2,2,2,2,2,2,2,2,2,
2,2,2,2,2,2,2,2,2,2,2,2,2,2,2,2,2,2,2,2,2,2,2,2,2,2,2,2,2,2,2,2,2,2,2,2,
2,2,2,2,2,2,2,2,2,2,2,2,2,2,2,2,2,2,2,2,2,2,2,2,2,2,2,2,2,2,2,2,2,2,2,2,
2,2,2,2,2,2,2,2,2,2,2,2,2,2,2,2,2,2,2,2,2,2,2,2,2,2,2,2,2,2,2,2,2,2,2,2,
2,2,2,2,2,2,2,2,2,2,2,2,2,2,2,2,2,2,2,2,2,2,2,2,2,2,2,4),(0.00206444117643367,
0.25427431608748,0.339067277347239,0.366399914497447,0.369061434760028,
0.370335247392758,0.371228429494803,0.372155344558195,0.373441236097224,
0.376046839704919,0.399823501786385,0.40241207047523,0.4026545356114,0.404864726580252,
0.407130600099304,0.409767078590461,0.411645952746294,0.419848751972015,
0.427270563141598,0.444946466908281,0.673772008220203,0.713191162614711,
0.7555123015024,0.777504155471055,0.78150229940178,0.783259178941547,0.784957261209794,
0.78663663324531,0.788930496568503,0.794651364311366,0.857185395057024,
0.926461665957577,0.972825146685942,1.05650480205845,1.12550004865115,1.15920049507532,
1.17569845060946,1.17864228241125,1.18021179553869,1.18138039652398,1.1826559664504,
1.1849094593692,1.19150880487733,1.30059208763602,1.40326557985149,1.5397807850755,
1.55065497057407,1.55488116716038,1.55781249227586,1.560652047084,1.56457398684755,
1.57348018923723,1.67899289130392,1.83091352603107,1.88509382078349,1.92414976652091,
1.93091139458827,1.93310332441546,1.93450668512066,1.9358198647796,1.93753408548038,
1.94128878902606,1.97433812524604,2.22326212126178,2.31257757723106,2.32109345218367,
2.32531609963515,2.32879963531253,2.33081733474463,2.33241286389285,2.33449352633316,
2.33810369138847,2.35198610581368,2.53765465498566,2.64981294354697,2.69618541992743,
2.73558363437747,2.74177836078784,2.74354731857468,2.74462686089695,2.74561037614764,
2.74688394018323,2.74894112955727,2.7598907940736,2.92997030265151,3.04230941574737,
3.13091685377812,3.13518458002826,3.13774633050417,3.14006615415957,3.14181852299347,
3.14349091243715,3.14579263247026,3.15162383273341,3.22031097737794,3.44198244811632,
3.53238790623307,3.53556798627373,3.53695164468424,3.53797767127976,3.53893043805087,
3.54023103646255,3.54346969333043,3.5783825105287,3.58367792980028,3.59541906151467,
3.78245951239566,3.92769609853722,3.93332771277499,3.93583849792533,3.93770303021958,
3.93943612865611,3.94180474663939,3.94771935640704,4.01307630757973,4.22564608669173,
4.28082937555888,4.31752831320715,4.3235686323625,4.32539047917649,4.32652444061578,
4.32756757043276,4.32891860880413,4.33116026160005,4.3438594230423,4.57367390309785,
4.63301584912154,4.69939728164292,4.71047233928644,4.71374672727321,4.71577036987524,
4.71761500046117,4.71999492430083,4.72493778518826,4.75692456115181,4.76082680167905,
4.76969162719881,4.77577112103574,4.79694903348135,4.98078786716294,5.01442476688674,
5.08069816059329,5.0830339466468,5.08494521092472,5.11037248331752,5.11340204678713,
5.1147558829414,5.11578085566193,5.11686461758359,5.11853806882708,5.12372880799352,
5.15328219438149,5.22180857063446,5.3691834022681,5.49819792987428,5.50657693398901,
5.50955679095335,5.51127388586721,5.51286612230062,5.51503369824752,5.51919526687294,
5.5450350833803,5.60114540550497,5.69772539950262,5.73745491140066,5.78091176263103,
5.89676209437594,5.90454857878548,5.90654815858638,5.90769532102681,5.90857228003648,
5.90970739990934,5.91172770244974,5.92089420512607,5.93789589720552,6.01546775262138,
6.12973379528788,6.30335351632527,6.3153507533736,6.31876683451587,6.32080212768807,
6.32257743616542,6.3247628737941,6.32895894639734,6.35501921408713,6.41172079298135,
6.51948258252078,6.63158643549496,6.70853586175171,6.7140851858047,6.71618358385647,
6.71742755931257,6.71870862528055,6.72036767146531,6.72219237612246,6.72519473094039,
6.73122800761504,6.78456977716475,6.93329597709434,7.07831315188783,7.08767636887057,
7.09135480854045,7.09402454255856,7.09686727712101,7.10061619099023,7.10871717976492,
7.24318436812602,7.43386226117847,7.46483461022097,7.46864804590523,7.47037291523631,
7.4716874519614,7.47305756489847,7.47515999696972,7.47758980986699,7.4820625745571,
7.51836372627306,7.57311000537312,7.80863370073895,7.85860202587526,7.86354818627313,
7.86594588987164,7.86765231124158,7.86926508762447,7.87150850442997,7.87598550855356,
7.9100650954623,8.00298056291935,8.02811508438221,8.04787397645065,8.05574823112596,
8.18274243880661,8.22431862697358,8.23345964133844,8.23630691607363,8.2430612220221,
8.27569808155605,8.27879071212485,8.28003919289574,8.28095624728956,8.2819547313747,
8.28294216818475,8.28533428064562,8.30204550286421,8.31565383282046,8.37478252038758,
8.42915885616388,8.65585175120397,8.67103334244475,8.67441359293433,8.67660937778111,
8.67837188007698,8.68036951869516,8.6837527936194,8.69680390794285,8.78801852432739,
8.81460594920854,8.83513705550795,8.85186178914556,8.86588208597962,8.877843906523,
8.88816962342697,8.89715695700585,8.96897369035021,8.99595240162936,9.01300327628705,
9.0456575410992,9.06850891022486,9.07139106781341,9.07270705278876,9.07372547807939,
9.07482397217211,9.07594845958547,9.07941229017193,9.08421522023498,9.09661652830864,
9.14387530061798,9.19667652314135,9.44942145331006,9.45607473128349,9.46528147473302,
9.46924659903031,9.47164214120946,9.47349396662997,9.47548960372275,9.47864165148474,
9.48864509131477,9.67383961418688,9.76497271985972,9.77251460448592,9.8537716397057,
9.85899437679942,9.86078353544733,9.8617972301364,9.86272925281889,9.86372016723375,
9.86496178249052,9.86684782188861,9.87030959177873,9.95674259834603),
 .UNSPECIFIED.);
#522=B_SPLINE_CURVE_WITH_KNOTS('',3,(#58644,#58645,#58646,#58647,#58648,
#58649,#58650,#58651,#58652,#58653,#58654),.UNSPECIFIED.,.F.,.F.,(4,1,1,
1,1,1,1,1,4),(-299.40224579153,-298.523994407224,-297.525586399173,-296.527178391122,
-296.027974387097,-295.528770383071,-294.530362375021,-293.53195436697,
-293.119454550391),.UNSPECIFIED.);
#523=B_SPLINE_CURVE_WITH_KNOTS('',3,(#58656,#58657,#58658,#58659,#58660,
#58661,#58662,#58663,#58664,#58665,#58666,#58667,#58668,#58669,#58670,#58671,
#58672,#58673,#58674,#58675,#58676,#58677,#58678,#58679,#58680,#58681,#58682,
#58683,#58684,#58685,#58686,#58687,#58688,#58689,#58690,#58691,#58692,#58693,
#58694,#58695,#58696,#58697,#58698,#58699,#58700,#58701,#58702,#58703,#58704,
#58705,#58706,#58707,#58708,#58709,#58710,#58711,#58712,#58713,#58714,#58715,
#58716,#58717,#58718,#58719,#58720,#58721,#58722,#58723,#58724,#58725,#58726,
#58727,#58728,#58729,#58730,#58731,#58732,#58733,#58734,#58735,#58736,#58737,
#58738,#58739,#58740,#58741,#58742,#58743,#58744,#58745,#58746,#58747,#58748,
#58749,#58750,#58751,#58752,#58753,#58754,#58755,#58756,#58757,#58758,#58759,
#58760,#58761,#58762,#58763,#58764,#58765,#58766,#58767,#58768,#58769,#58770,
#58771,#58772,#58773,#58774,#58775,#58776,#58777,#58778,#58779,#58780,#58781,
#58782,#58783,#58784,#58785,#58786,#58787,#58788,#58789,#58790,#58791,#58792,
#58793,#58794,#58795,#58796,#58797,#58798,#58799,#58800,#58801,#58802,#58803,
#58804,#58805,#58806,#58807,#58808,#58809,#58810,#58811,#58812,#58813,#58814,
#58815,#58816,#58817,#58818,#58819,#58820,#58821,#58822,#58823,#58824,#58825,
#58826,#58827,#58828,#58829,#58830,#58831,#58832,#58833,#58834,#58835,#58836,
#58837,#58838,#58839,#58840,#58841,#58842,#58843,#58844,#58845,#58846,#58847,
#58848,#58849,#58850,#58851,#58852,#58853,#58854,#58855,#58856,#58857,#58858,
#58859,#58860,#58861,#58862,#58863,#58864,#58865,#58866,#58867,#58868,#58869,
#58870,#58871,#58872,#58873,#58874,#58875,#58876,#58877,#58878,#58879,#58880,
#58881,#58882,#58883,#58884,#58885,#58886,#58887,#58888,#58889,#58890,#58891,
#58892,#58893,#58894,#58895,#58896,#58897,#58898,#58899,#58900,#58901,#58902,
#58903,#58904,#58905,#58906,#58907,#58908,#58909,#58910,#58911,#58912,#58913,
#58914,#58915,#58916,#58917,#58918,#58919,#58920,#58921,#58922,#58923,#58924,
#58925,#58926,#58927,#58928,#58929,#58930,#58931,#58932,#58933,#58934,#58935,
#58936,#58937,#58938,#58939,#58940,#58941,#58942,#58943,#58944,#58945,#58946,
#58947,#58948,#58949,#58950,#58951,#58952,#58953,#58954,#58955,#58956,#58957,
#58958,#58959,#58960,#58961,#58962,#58963,#58964,#58965,#58966,#58967,#58968,
#58969,#58970,#58971,#58972,#58973,#58974,#58975,#58976,#58977,#58978,#58979,
#58980,#58981,#58982,#58983,#58984,#58985,#58986,#58987,#58988,#58989,#58990,
#58991,#58992,#58993,#58994,#58995,#58996,#58997,#58998,#58999,#59000,#59001,
#59002,#59003,#59004,#59005,#59006,#59007,#59008,#59009,#59010,#59011,#59012,
#59013,#59014,#59015,#59016,#59017,#59018,#59019,#59020,#59021,#59022,#59023,
#59024,#59025,#59026,#59027,#59028,#59029,#59030,#59031,#59032,#59033,#59034,
#59035,#59036,#59037,#59038,#59039,#59040,#59041,#59042,#59043,#59044,#59045,
#59046,#59047,#59048,#59049,#59050,#59051,#59052,#59053,#59054,#59055,#59056,
#59057,#59058,#59059,#59060,#59061,#59062,#59063,#59064,#59065,#59066,#59067,
#59068,#59069,#59070,#59071,#59072,#59073,#59074,#59075,#59076,#59077,#59078,
#59079,#59080,#59081,#59082,#59083,#59084,#59085,#59086,#59087,#59088,#59089,
#59090,#59091,#59092,#59093,#59094,#59095,#59096,#59097,#59098,#59099,#59100,
#59101,#59102,#59103,#59104,#59105,#59106,#59107,#59108,#59109,#59110,#59111,
#59112,#59113,#59114,#59115,#59116,#59117,#59118,#59119,#59120,#59121,#59122,
#59123,#59124,#59125,#59126,#59127,#59128,#59129,#59130,#59131,#59132,#59133,
#59134,#59135,#59136,#59137,#59138,#59139,#59140,#59141,#59142,#59143,#59144,
#59145,#59146,#59147,#59148,#59149,#59150,#59151,#59152,#59153,#59154,#59155,
#59156,#59157,#59158,#59159,#59160,#59161,#59162,#59163,#59164,#59165,#59166,
#59167,#59168,#59169,#59170,#59171,#59172,#59173,#59174,#59175,#59176,#59177,
#59178,#59179,#59180,#59181,#59182,#59183,#59184,#59185,#59186,#59187,#59188,
#59189,#59190,#59191,#59192,#59193,#59194,#59195,#59196,#59197,#59198,#59199,
#59200,#59201,#59202,#59203,#59204,#59205,#59206,#59207,#59208,#59209,#59210,
#59211,#59212,#59213,#59214,#59215),.UNSPECIFIED.,.F.,.F.,(4,2,2,2,2,2,
2,2,2,2,2,2,2,2,2,2,2,2,2,2,2,2,2,2,2,2,2,2,2,2,2,2,2,2,2,2,2,2,2,2,2,2,
2,2,2,2,2,2,2,2,2,2,2,2,2,2,2,2,2,2,2,2,2,2,2,2,2,2,2,2,2,2,2,2,2,2,2,2,
2,2,2,2,2,2,2,2,2,2,2,2,2,2,2,2,2,2,2,2,2,2,2,2,2,2,2,2,2,2,2,2,2,2,2,2,
2,2,2,2,2,2,2,2,2,2,2,2,2,2,2,2,2,2,2,2,2,2,2,2,2,2,2,2,2,2,2,2,2,2,2,2,
2,2,2,2,2,2,2,2,2,2,2,2,2,2,2,2,2,2,2,2,2,2,2,2,2,2,2,2,2,2,2,2,2,2,2,2,
2,2,2,2,2,2,2,2,2,2,2,2,2,2,2,2,2,2,2,2,2,2,2,2,2,2,2,2,2,2,2,2,2,2,2,2,
2,2,2,2,2,2,2,2,2,2,2,2,2,2,2,2,2,2,2,2,2,2,2,2,2,2,2,2,2,2,2,2,2,2,2,2,
2,2,2,2,2,2,2,2,2,2,2,2,2,2,2,2,2,2,2,2,2,4),(0.00182729117505357,0.0654996008145292,
0.0701074088737819,0.0728422120533014,0.0747943813940611,0.0765090142978765,
0.0783641644564241,0.080774520517057,0.0860086466192052,0.124845090641752,
0.144694040278344,0.154702975825758,0.40987014630865,0.45616129617932,0.463125478905227,
0.465043948671223,0.46619968573496,0.467237281011554,0.46856891796434,0.470697699179319,
0.481601163029537,0.747138396296082,0.792862962430324,0.829746281241003,
0.842481204638353,0.851037642781539,0.854000319653516,0.855717376106154,
0.85755893755648,0.859913651506986,0.864729058813973,0.894106271274702,
0.898618119695143,0.904633638535121,0.914247332001024,1.00742449286921,
1.05992933584833,1.07452584042807,1.0910717537891,1.11014411552814,1.16817491732573,
1.2148914464747,1.24687716946578,1.25238282492018,1.25411813001952,1.25521656794703,
1.25623558051963,1.25755322401423,1.2597585799249,1.27308654478159,1.50799210840985,
1.57744093902551,1.6208103577681,1.63640662173346,1.64301766962169,1.6480362705988,
1.65036613427066,1.65204407236765,1.65370002848432,1.65593869058125,1.66029091512886,
1.69286389726613,1.69658950861984,1.69919706376264,1.70186714832853,1.85697384184988,
1.88999843290375,1.91007005830308,1.93830949810155,2.00972820820729,2.03997228620068,
2.04522850700231,2.04689998095725,2.04796169750311,2.04894968195724,2.05024496313522,
2.05243649565854,2.06585448731704,2.28666978807397,2.38758047806079,2.44595834684701,
2.45265771901319,2.45764652238093,2.46003501494346,2.46184226625668,2.46352016713626,
2.46581029355287,2.47151377129052,2.53340074968265,2.68552969186938,2.78920195806079,
2.81177295072392,2.84727143189108,2.85394022484021,2.85611999235643,2.85752015022534,
2.8588335815403,2.86055300183686,2.8641993442349,2.89180785181045,3.0844444269064,
3.2065262221986,3.22534029125046,3.23054063340928,3.23368342094688,3.23643460942883,
3.2398320113717,3.24619211114061,3.2768870628765,3.47482396011193,3.57602025212566,
3.60543698590955,3.60882080164138,3.61048091455183,3.6116605155399,3.61289607808051,
3.61461164743346,3.61903934258769,3.68129429164791,3.84926009682395,3.93761416976383,
3.99262975945702,4.0023472315729,4.00540544075515,4.00734064232026,4.00913564451352,
4.01145658949688,4.01645224879046,4.05208268913113,4.31609399402479,4.41456176489621,
4.4187237504521,4.42024472938987,4.42127034980716,4.42226755846087,4.42346247212247,
4.42640738688737,4.45133822809549,4.66761540676287,4.76016208375238,4.79344126570143,
4.81129208296053,4.81503909602459,4.81711739238437,4.81870103731314,4.82046670605492,
4.82368956615312,4.8338563599165,4.97962355324292,5.18130508682964,5.18543676865487,
5.20911706154826,5.21202919657863,5.21335075455124,5.21437024168725,5.21546667281263,
5.2171935044951,5.22262961720931,5.25397463473391,5.32605112253785,5.58958983290153,
5.60339136798987,5.6094498917172,5.61184253879933,5.61358144901017,5.61544115194774,
5.61792622678755,5.62342132276256,5.73049487927807,5.78318288577994,5.98658317891159,
5.99874789909316,6.00095682330009,6.00229784382983,6.00333912369449,6.00447715089883,
6.00631853299332,6.01254098034217,6.17263244944631,6.37221731355809,6.38582911113373,
6.38948215627375,6.39161168307753,6.39344071902455,6.39565677762603,6.39980535924009,
6.42278950143117,6.46683055893895,6.56887134550894,6.77491237108166,6.78008815612838,
6.78802695125784,6.79006455851089,6.79122749114294,6.79221293317646,6.79316562617901,
6.79502272608746,6.80195385427695,6.8493630658064,6.88121561979771,7.16418361515147,
7.18129963686276,7.18482787705405,7.18706927550078,7.18883595048827,7.19080433197611,
7.19405826928279,7.20574046382023,7.27969874357913,7.38453879689245,7.56898986283093,
7.58046465038643,7.5827391770487,7.58393386760999,7.58488706536052,7.5858004939159,
7.58745229944187,7.59260531876554,7.62195727914172,7.68963173470231,7.93040852785828,
7.98811522345443,7.99371927006413,7.99599174943956,7.99766467407823,7.99947418775777,
8.00192793984711,8.00750374231509,8.08846485719693,8.11953028399923,8.25009379231305,
8.25821453492117,8.26603424871818,8.38140637541629,8.38955344340338,8.39195618198125,
8.39339978113528,8.39468910491681,8.39627956338108,8.39932666436457,8.41806127250395,
8.44177118949497,8.49341867941202,8.63771858293601,8.75464344580777,8.7637076713746,
8.7673341891042,8.76998938803991,8.77283784285586,8.77663137687114,8.78497728089117,
8.97350939317952,9.06406468418882,9.13916442045584,9.14036422609357,9.14223971689198,
9.14489216603862,9.14639406936621,9.14758057811493,9.14906387107188,9.15161754904803,
9.16198573584434,9.31856172853097,9.3922476959119,9.52838779727184,9.53771523847683,
9.54084242042248,9.5425974340325,9.54419637600433,9.54633087455309,9.55029192990362,
9.57142843442649,9.61230281067081,9.66818508581611,9.82376476595195,9.93627842990203,
9.94235955118631,9.95222662661329,9.95437668741503,9.95538583871127),
 .UNSPECIFIED.);
#524=B_SPLINE_CURVE_WITH_KNOTS('',3,(#59217,#59218,#59219,#59220,#59221,
#59222,#59223,#59224,#59225,#59226,#59227,#59228,#59229,#59230,#59231,#59232,
#59233,#59234,#59235,#59236,#59237,#59238,#59239,#59240,#59241,#59242,#59243,
#59244,#59245,#59246,#59247,#59248,#59249,#59250,#59251,#59252,#59253,#59254,
#59255,#59256,#59257,#59258,#59259,#59260,#59261,#59262,#59263,#59264,#59265,
#59266,#59267,#59268,#59269,#59270,#59271,#59272,#59273,#59274,#59275,#59276,
#59277,#59278,#59279,#59280,#59281,#59282,#59283,#59284,#59285,#59286,#59287,
#59288,#59289,#59290,#59291,#59292,#59293,#59294,#59295,#59296,#59297,#59298,
#59299,#59300,#59301,#59302,#59303,#59304,#59305,#59306,#59307,#59308,#59309,
#59310,#59311,#59312,#59313,#59314,#59315,#59316,#59317,#59318,#59319,#59320,
#59321,#59322,#59323,#59324,#59325,#59326,#59327,#59328,#59329,#59330,#59331,
#59332,#59333,#59334,#59335,#59336,#59337,#59338,#59339,#59340,#59341,#59342,
#59343,#59344,#59345,#59346,#59347,#59348,#59349,#59350,#59351,#59352,#59353,
#59354,#59355,#59356,#59357,#59358,#59359,#59360,#59361,#59362,#59363,#59364,
#59365,#59366,#59367,#59368,#59369,#59370,#59371,#59372,#59373,#59374,#59375,
#59376,#59377,#59378,#59379,#59380,#59381,#59382,#59383,#59384,#59385,#59386,
#59387,#59388,#59389,#59390,#59391,#59392,#59393,#59394,#59395,#59396,#59397,
#59398,#59399,#59400,#59401,#59402,#59403,#59404,#59405,#59406,#59407,#59408,
#59409,#59410,#59411,#59412,#59413,#59414,#59415,#59416,#59417,#59418,#59419,
#59420,#59421,#59422,#59423,#59424,#59425,#59426,#59427,#59428,#59429,#59430,
#59431,#59432,#59433,#59434,#59435,#59436,#59437,#59438,#59439,#59440,#59441,
#59442,#59443,#59444,#59445,#59446,#59447,#59448,#59449,#59450,#59451,#59452,
#59453,#59454,#59455,#59456,#59457,#59458,#59459,#59460,#59461,#59462,#59463,
#59464,#59465,#59466,#59467,#59468,#59469,#59470,#59471,#59472,#59473,#59474,
#59475,#59476,#59477,#59478,#59479,#59480,#59481),.UNSPECIFIED.,.F.,.F.,
(4,3,3,3,3,3,3,3,3,3,3,3,3,3,3,3,3,3,3,3,3,3,3,3,3,3,3,3,3,3,3,3,3,3,3,
3,3,3,3,3,3,3,3,3,3,3,3,3,3,3,3,3,3,3,3,3,3,3,3,3,3,3,3,3,3,3,3,3,3,3,3,
3,3,3,3,3,3,3,3,3,3,3,3,3,3,3,3,3,4),(-280.552952748318,-280.479027221112,
-280.405188492471,-280.33142210548,-280.257713656703,-280.184048785067,
-280.110413161578,-280.036780331792,-279.963145359955,-279.889495294389,
-279.815817176824,-279.742059132793,-279.668256289114,-279.594352502714,
-279.554242254257,-279.479681192729,-279.405200965071,-279.330787658037,
-279.256427402599,-279.182106364968,-279.10781073802,-279.03351400232,-278.959212672779,
-278.884894259454,-278.810546265728,-278.736119149574,-278.661646642781,
-278.587077817322,-278.555834246206,-278.481273260072,-278.406793095686,
-278.332379839843,-278.258019623551,-278.183698613046,-278.109403001225,
-278.035106262717,-277.960804919181,-277.886486480672,-277.81213845056,
-277.737711281296,-277.663238711751,-277.588669809291,-277.557426238155,
-277.483532756901,-277.409721890759,-277.335979195336,-277.262290276441,
-277.188640779214,-277.11501637803,-277.041388531105,-276.967754665036,
-276.894101822821,-276.820417038612,-276.746646485715,-276.672827775099,
-276.598903124232,-276.559018230104,-276.48439516469,-276.409857835809,
-276.335392347056,-276.260984849414,-276.186621532172,-276.11228861427,
-276.037962151675,-275.96363581972,-275.889297160923,-275.814933713645,
-275.740498456463,-275.666021983071,-275.59145561093,-275.560610222053,
-275.482244548012,-275.403975378574,-275.325797432178,-275.247736659987,
-275.169747597733,-275.091847744738,-275.061406218028,-274.983495629914,
-274.905515233012,-274.827459903152,-274.749275187397,-274.67101980779,
-274.592645117153,-274.562202214002,-274.473533367918,-274.385256001682,
-274.297705320811,-274.269898628852),.UNSPECIFIED.);
#525=B_SPLINE_CURVE_WITH_KNOTS('',3,(#59483,#59484,#59485,#59486,#59487,
#59488,#59489,#59490,#59491,#59492,#59493,#59494,#59495,#59496,#59497,#59498,
#59499,#59500),.UNSPECIFIED.,.F.,.F.,(4,2,2,2,2,2,2,2,4),(-274.269898628852,
-273.434981716958,-272.600064805063,-271.765147893168,-270.930230981273,
-270.095314069378,-269.260397157483,-268.425480245588,-267.986713321673),
 .UNSPECIFIED.);
#526=B_SPLINE_CURVE_WITH_KNOTS('',3,(#59502,#59503,#59504,#59505,#59506,
#59507,#59508,#59509,#59510,#59511,#59512,#59513,#59514,#59515,#59516,#59517,
#59518,#59519,#59520,#59521,#59522,#59523,#59524,#59525,#59526,#59527,#59528,
#59529,#59530,#59531,#59532,#59533,#59534,#59535,#59536,#59537,#59538,#59539,
#59540,#59541,#59542,#59543,#59544,#59545,#59546,#59547,#59548,#59549,#59550,
#59551,#59552,#59553,#59554,#59555,#59556,#59557,#59558,#59559,#59560,#59561,
#59562,#59563,#59564,#59565,#59566,#59567,#59568,#59569,#59570,#59571,#59572,
#59573,#59574,#59575,#59576,#59577,#59578,#59579,#59580,#59581,#59582,#59583,
#59584,#59585,#59586,#59587,#59588,#59589,#59590,#59591,#59592,#59593,#59594,
#59595,#59596,#59597,#59598,#59599,#59600,#59601,#59602,#59603,#59604,#59605,
#59606,#59607,#59608,#59609,#59610,#59611,#59612,#59613,#59614,#59615,#59616,
#59617,#59618,#59619,#59620,#59621,#59622,#59623,#59624,#59625,#59626,#59627,
#59628,#59629,#59630,#59631,#59632,#59633,#59634,#59635,#59636,#59637,#59638,
#59639,#59640,#59641,#59642,#59643,#59644,#59645,#59646,#59647,#59648,#59649,
#59650,#59651,#59652,#59653,#59654,#59655,#59656,#59657,#59658,#59659,#59660,
#59661,#59662,#59663,#59664,#59665,#59666,#59667,#59668,#59669,#59670,#59671,
#59672,#59673,#59674,#59675,#59676,#59677,#59678,#59679,#59680,#59681,#59682,
#59683,#59684,#59685,#59686,#59687,#59688,#59689,#59690,#59691,#59692,#59693,
#59694,#59695,#59696,#59697,#59698,#59699,#59700,#59701,#59702,#59703,#59704,
#59705,#59706,#59707,#59708,#59709,#59710,#59711,#59712,#59713,#59714,#59715,
#59716,#59717,#59718,#59719,#59720,#59721,#59722,#59723,#59724,#59725,#59726,
#59727,#59728,#59729,#59730,#59731,#59732,#59733,#59734,#59735,#59736,#59737,
#59738,#59739,#59740,#59741,#59742,#59743,#59744,#59745,#59746,#59747,#59748,
#59749,#59750,#59751,#59752,#59753,#59754,#59755,#59756,#59757,#59758,#59759,
#59760,#59761,#59762,#59763),.UNSPECIFIED.,.F.,.F.,(4,3,3,3,3,3,3,3,3,3,
3,3,3,3,3,3,3,3,3,3,3,3,3,3,3,3,3,3,3,3,3,3,3,3,3,3,3,3,3,3,3,3,3,3,3,3,
3,3,3,3,3,3,3,3,3,3,3,3,3,3,3,3,3,3,3,3,3,3,3,3,3,3,3,3,3,3,3,3,3,3,3,3,
3,3,3,3,3,4),(-267.986713321673,-267.906108764019,-267.822918112426,-267.741928442518,
-267.657637300082,-267.573346157646,-267.498787061105,-267.424303411479,
-267.349881348361,-267.275507051909,-267.201166734104,-267.126846630343,
-267.052517761171,-266.978179527966,-266.903819469602,-266.829425115786,
-266.7549447622,-266.680415009185,-266.605783278329,-266.574938149595,-266.501018363321,
-266.427185387969,-266.353424762344,-266.27972207882,-266.206062972188,
-266.132433109361,-266.058806033688,-265.985176804652,-265.911532466892,
-265.837860058435,-265.764107731001,-265.69031058017,-265.616412553523,
-265.576530141544,-265.501969080047,-265.42748885242,-265.353075545418,
-265.278715290011,-265.204394252411,-265.130098625494,-265.055801889826,
-264.981500560316,-264.907182147023,-264.832834153328,-264.758407037205,
-264.683934530443,-264.609365705014,-264.578122133493,-264.503561147286,
-264.429080982827,-264.354667726912,-264.280307510546,-264.20598649997,
-264.131690888076,-264.057394149496,-263.983092805889,-263.908774367309,
-263.834426337128,-263.759999167794,-263.68552659818,-263.610957695652,
-263.579714125442,-263.505820644216,-263.432009778101,-263.358267082705,
-263.284578163837,-263.210928666637,-263.137304265478,-263.063676418577,
-262.990042552533,-262.916389710342,-262.842704926157,-262.768934373282,
-262.695115662688,-262.621191011842,-262.581306117391,-262.507515619813,
-262.433810262704,-262.360175471895,-262.286596727781,-262.213059860217,
-262.13954538831,-262.066040247222,-261.992531379277,-261.918974420258,
-261.84539359123,-261.771731328759,-261.704055150649),.UNSPECIFIED.);
#527=B_SPLINE_CURVE_WITH_KNOTS('',3,(#59765,#59766,#59767,#59768,#59769,
#59770,#59771,#59772,#59773,#59774,#59775,#59776,#59777,#59778,#59779,#59780,
#59781,#59782,#59783,#59784,#59785,#59786,#59787,#59788,#59789,#59790,#59791,
#59792,#59793,#59794,#59795,#59796,#59797,#59798,#59799,#59800,#59801,#59802,
#59803,#59804,#59805,#59806,#59807,#59808,#59809,#59810,#59811,#59812,#59813,
#59814,#59815,#59816,#59817,#59818,#59819,#59820,#59821,#59822,#59823,#59824,
#59825,#59826,#59827,#59828,#59829,#59830,#59831,#59832,#59833,#59834,#59835,
#59836,#59837,#59838,#59839,#59840,#59841,#59842,#59843,#59844,#59845,#59846,
#59847,#59848,#59849,#59850,#59851,#59852,#59853,#59854,#59855,#59856,#59857,
#59858,#59859,#59860,#59861,#59862,#59863,#59864,#59865,#59866,#59867,#59868,
#59869,#59870,#59871,#59872,#59873,#59874,#59875,#59876,#59877,#59878,#59879,
#59880,#59881,#59882,#59883,#59884,#59885,#59886,#59887,#59888,#59889,#59890,
#59891,#59892,#59893,#59894,#59895,#59896,#59897,#59898,#59899,#59900,#59901,
#59902,#59903,#59904,#59905,#59906,#59907,#59908,#59909,#59910,#59911,#59912,
#59913,#59914,#59915,#59916,#59917,#59918,#59919,#59920,#59921,#59922,#59923,
#59924,#59925,#59926,#59927,#59928,#59929,#59930,#59931,#59932,#59933,#59934,
#59935,#59936,#59937,#59938,#59939,#59940,#59941,#59942,#59943,#59944,#59945,
#59946,#59947,#59948,#59949,#59950,#59951,#59952,#59953,#59954,#59955,#59956,
#59957,#59958,#59959,#59960,#59961,#59962,#59963,#59964,#59965,#59966,#59967,
#59968,#59969,#59970,#59971,#59972,#59973,#59974,#59975,#59976,#59977,#59978,
#59979,#59980,#59981,#59982,#59983,#59984,#59985,#59986,#59987,#59988,#59989,
#59990,#59991,#59992,#59993,#59994,#59995,#59996,#59997,#59998,#59999,#60000,
#60001,#60002,#60003,#60004,#60005,#60006,#60007,#60008,#60009,#60010,#60011,
#60012,#60013,#60014,#60015,#60016,#60017,#60018,#60019,#60020,#60021,#60022,
#60023,#60024,#60025,#60026,#60027,#60028,#60029,#60030,#60031,#60032,#60033,
#60034,#60035,#60036,#60037,#60038,#60039,#60040,#60041,#60042,#60043,#60044,
#60045,#60046,#60047,#60048,#60049,#60050,#60051,#60052,#60053,#60054,#60055,
#60056,#60057,#60058,#60059,#60060,#60061,#60062,#60063,#60064,#60065,#60066,
#60067,#60068,#60069,#60070,#60071,#60072,#60073,#60074,#60075,#60076,#60077,
#60078,#60079,#60080,#60081,#60082,#60083,#60084,#60085,#60086,#60087,#60088,
#60089,#60090,#60091,#60092,#60093,#60094,#60095,#60096,#60097,#60098,#60099,
#60100,#60101,#60102,#60103,#60104,#60105,#60106,#60107,#60108,#60109,#60110,
#60111,#60112,#60113,#60114,#60115,#60116,#60117,#60118,#60119,#60120,#60121,
#60122,#60123,#60124,#60125,#60126,#60127,#60128,#60129,#60130,#60131,#60132,
#60133,#60134,#60135,#60136,#60137,#60138,#60139,#60140,#60141,#60142,#60143,
#60144,#60145,#60146,#60147,#60148,#60149,#60150,#60151,#60152,#60153,#60154,
#60155,#60156,#60157,#60158,#60159,#60160,#60161,#60162,#60163,#60164,#60165,
#60166,#60167,#60168,#60169,#60170,#60171,#60172,#60173,#60174,#60175,#60176,
#60177,#60178,#60179,#60180,#60181,#60182,#60183,#60184,#60185,#60186,#60187,
#60188,#60189,#60190,#60191,#60192,#60193,#60194,#60195,#60196,#60197,#60198,
#60199,#60200,#60201,#60202,#60203,#60204,#60205,#60206,#60207,#60208,#60209,
#60210,#60211,#60212,#60213,#60214,#60215,#60216,#60217,#60218,#60219,#60220,
#60221,#60222,#60223,#60224,#60225,#60226,#60227,#60228,#60229,#60230,#60231,
#60232,#60233,#60234,#60235,#60236,#60237,#60238,#60239,#60240,#60241,#60242,
#60243,#60244,#60245,#60246,#60247,#60248,#60249,#60250,#60251,#60252,#60253,
#60254,#60255,#60256,#60257,#60258,#60259,#60260,#60261,#60262,#60263,#60264,
#60265,#60266,#60267,#60268,#60269,#60270,#60271,#60272,#60273,#60274,#60275,
#60276,#60277,#60278,#60279,#60280,#60281,#60282,#60283,#60284,#60285,#60286,
#60287,#60288,#60289,#60290,#60291,#60292,#60293,#60294,#60295,#60296,#60297,
#60298,#60299,#60300,#60301,#60302,#60303,#60304,#60305,#60306,#60307,#60308,
#60309,#60310,#60311,#60312,#60313,#60314,#60315,#60316,#60317,#60318,#60319,
#60320,#60321,#60322,#60323,#60324,#60325,#60326,#60327,#60328,#60329,#60330,
#60331,#60332,#60333,#60334,#60335,#60336,#60337,#60338,#60339,#60340),
 .UNSPECIFIED.,.F.,.F.,(4,2,2,2,2,2,2,2,2,2,2,2,2,2,2,2,2,2,2,2,2,2,2,2,
2,2,2,2,2,2,2,2,2,2,2,2,2,2,2,2,2,2,2,2,2,2,2,2,2,2,2,2,2,2,2,2,2,2,2,2,
2,2,2,2,2,2,2,2,2,2,2,2,2,2,2,2,2,2,2,2,2,2,2,2,2,2,2,2,2,2,2,2,2,2,2,2,
2,2,2,2,2,2,2,2,2,2,2,2,2,2,2,2,2,2,2,2,2,2,2,2,2,2,2,2,2,2,2,2,2,2,2,2,
2,2,2,2,2,2,2,2,2,2,2,2,2,2,2,2,2,2,2,2,2,2,2,2,2,2,2,2,2,2,2,2,2,2,2,2,
2,2,2,2,2,2,2,2,2,2,2,2,2,2,2,2,2,2,2,2,2,2,2,2,2,2,2,2,2,2,2,2,2,2,2,2,
2,2,2,2,2,2,2,2,2,2,2,2,2,2,2,2,2,2,2,2,2,2,2,2,2,2,2,2,2,2,2,2,2,2,2,2,
2,2,2,2,2,2,2,2,2,2,2,2,2,2,2,2,2,2,2,2,2,2,2,2,2,2,2,2,2,2,2,2,2,2,2,2,
2,2,2,2,2,2,2,2,2,2,2,4),(0.00135467936860461,0.105905930347926,0.109781162785451,
0.111971599148687,0.113457851424939,0.114902647586442,0.116203225236225,
0.117858513503175,0.120476298019936,0.133391480944711,0.242813923920672,
0.254956640849107,0.437672197329887,0.477662082861804,0.486041402095746,
0.489842763732373,0.492694103771591,0.49534988272335,0.498973832276405,
0.508014324551167,0.622732808646861,0.696276497028578,0.723696217518591,
0.794401940169627,0.842975615310469,0.856494980750388,0.864683171939286,
0.866427018531058,0.867733985107433,0.869056540279512,0.870274573891002,
0.871921959007485,0.875949218922695,0.926505973886985,0.975494227105744,
1.04932196243803,1.05858070480526,1.069232921339,1.08159728199511,1.096132785653,
1.14426648409367,1.19730391518818,1.25035727062657,1.25985354027119,1.2628859183482,
1.26481576058556,1.26661346119229,1.2689487512867,1.27283496982685,1.28145053066355,
1.43512062978405,1.5200757110767,1.61755590934972,1.65760373379746,1.66858440667646,
1.67293352300218,1.67611277346537,1.67748866140144,1.67848626687923,1.67940466161041,
1.68064735337387,1.68368655596113,1.71373931107317,1.75671962746866,1.81136529901845,
1.9477769258085,1.97150830227803,2.00615049657611,2.04687088502283,2.06784821882593,
2.07177970623093,2.0738983549376,2.07564019400885,2.07769235081026,2.08122368923301,
2.09449282191791,2.29013857515821,2.38491141486254,2.42869334652271,2.45361764704357,
2.4669851894006,2.46925575352262,2.47047702433452,2.47148355053888,2.47265366486427,
2.47465640774287,2.48206850930876,2.59218348615894,2.74717041969454,2.80325040293928,
2.83904097737279,2.86300500251538,2.86720307836638,2.86943026323644,2.87126052566002,
2.87338247474936,2.87700070248533,2.89026193690734,3.08611885385599,3.2502463267109,
3.25445744657098,3.25758780895534,3.2589890650467,3.26004111515289,3.26101924152143,
3.262363868879,3.26504608623641,3.28774287235409,3.32255572966217,3.35329934152961,
3.55296650186679,3.61397157562832,3.64151943120264,3.64587535615561,3.6481359042926,
3.64996818586396,3.65179490400689,3.65509603630614,3.66526739576775,3.81328358323173,
3.943884280613,3.99187330242446,4.02847341842462,4.04428348811881,4.04670845846484,
4.04795802045265,4.0488701693116,4.04984833325476,4.05153662365964,4.05635834462272,
4.13185719284762,4.32090066557039,4.38176762556886,4.430648694589,4.43964937652221,
4.44260545367139,4.44450803499917,4.44629547384494,4.44863921353242,4.45362274715417,
4.49131402928216,4.49298098767543,4.4940723283588,4.49748049918456,4.50036729068039,
4.5067399248079,4.51150395115702,4.58217694522431,4.73464532075125,4.80411363501906,
4.83319291843746,4.83832249637584,4.83997875602932,4.84103719292627,4.84202666524086,
4.84333059408172,4.8462528534955,4.87086724271372,4.87189624476929,4.97793406782097,
5.08840400771867,5.23809519846542,5.24694095567933,5.25079643720284,5.25312254623189,
5.25491872044257,5.25685239417388,5.25990229748367,5.26954564224272,5.32389195446405,
5.4226108409505,5.63286354251302,5.64583364080445,5.64845888757635,5.65011780321481,
5.65141892171266,5.65286194054345,5.655232127965,5.66358743332866,5.71903089472145,
5.78437674262154,5.98512045033842,6.01637918488383,6.02225639943245,6.02587022251524,
6.02870245508081,6.031770781023,6.03663415163201,6.05226394773474,6.14152795757657,
6.25955863475273,6.38585091922345,6.39953468820055,6.40220526203005,6.40385891252999,
6.40516272185708,6.40659381889168,6.40891102236911,6.41676080627408,6.46309497171556,
6.53550357264128,6.77870743965064,6.79470629261983,6.79817002131697,6.80040153322107,
6.80218066925732,6.80414379072952,6.80733911484718,6.81117303003682,6.81863737892238,
6.88832271622816,6.99800239906012,7.19835282047591,7.20067573968731,7.21094644236082,
7.21295024848259,7.21418986680626,7.21517028977066,7.21625910313221,7.21805109503241,
7.22439814698596,7.26535678174477,7.32944300393575,7.40395566010084,7.54091378183065,
7.60153121281455,7.60717384761469,7.609443344494,7.61110739117516,7.61286434970071,
7.61521408922589,7.61781774980441,7.62218648233486,7.63112688574736,7.69057513380319,
7.7486400408186,7.98359329986033,8.0029422908334,8.00541587966643,8.00668319994108,
8.00762739005743,8.00865980031254,8.01007950197134,8.01339186615285,8.10549354228159,
8.22094636824289,8.30951005776843,8.39619016231785,8.40255255250107,8.40521377229103,
8.40708657694722,8.40894553172706,8.41082591555787,8.41568024097913,8.46028577977377,
8.5344087007939,8.77987993903232,8.79234537718995,8.79457326394936,8.7959202825172,
8.79696287278316,8.79809884642329,8.79992956171754,8.80604952056384,8.90638692857541,
9.00918948901993,9.0689030627306,9.17457944142369,9.18130774150486,9.18403339794349,
9.18592030380121,9.18776827571486,9.18962987628439,9.19430613881731,9.23146619108504,
9.32707261236817,9.53714990258149,9.55732759127054,9.58051070062318,9.58346242184171,
9.58480219008999,9.5858250473158,9.586914795481,9.58861503086718,9.59402837030787,
9.62563108756224,9.67216786306517,9.95668469293117),.UNSPECIFIED.);
#528=B_SPLINE_CURVE_WITH_KNOTS('',3,(#60342,#60343,#60344,#60345,#60346,
#60347,#60348,#60349,#60350,#60351,#60352,#60353,#60354,#60355,#60356,#60357,
#60358,#60359,#60360,#60361,#60362,#60363,#60364,#60365,#60366,#60367,#60368,
#60369,#60370,#60371,#60372,#60373,#60374,#60375,#60376,#60377,#60378,#60379,
#60380,#60381,#60382,#60383,#60384,#60385,#60386,#60387,#60388,#60389,#60390,
#60391,#60392,#60393,#60394,#60395,#60396,#60397,#60398,#60399,#60400,#60401,
#60402,#60403,#60404,#60405,#60406,#60407,#60408,#60409,#60410,#60411,#60412,
#60413,#60414,#60415,#60416,#60417,#60418,#60419,#60420,#60421,#60422,#60423,
#60424,#60425,#60426,#60427,#60428,#60429,#60430,#60431,#60432,#60433,#60434,
#60435,#60436,#60437,#60438,#60439,#60440,#60441,#60442,#60443,#60444,#60445,
#60446,#60447,#60448,#60449,#60450,#60451,#60452,#60453,#60454,#60455,#60456,
#60457,#60458,#60459,#60460,#60461,#60462,#60463,#60464,#60465,#60466,#60467,
#60468,#60469,#60470,#60471,#60472,#60473,#60474,#60475,#60476,#60477,#60478,
#60479,#60480,#60481,#60482,#60483,#60484,#60485,#60486,#60487,#60488,#60489,
#60490,#60491,#60492,#60493,#60494,#60495,#60496,#60497,#60498,#60499,#60500,
#60501,#60502,#60503,#60504,#60505,#60506,#60507,#60508,#60509,#60510,#60511,
#60512,#60513,#60514,#60515,#60516,#60517,#60518,#60519,#60520,#60521,#60522,
#60523,#60524,#60525,#60526,#60527,#60528,#60529,#60530,#60531,#60532,#60533,
#60534,#60535,#60536,#60537,#60538,#60539,#60540,#60541,#60542,#60543,#60544,
#60545,#60546,#60547,#60548,#60549,#60550,#60551,#60552,#60553,#60554,#60555,
#60556,#60557,#60558,#60559,#60560,#60561,#60562,#60563,#60564,#60565,#60566,
#60567,#60568,#60569,#60570,#60571,#60572,#60573,#60574,#60575,#60576,#60577,
#60578,#60579,#60580,#60581,#60582,#60583,#60584,#60585,#60586,#60587,#60588,
#60589,#60590,#60591,#60592,#60593,#60594,#60595,#60596,#60597,#60598,#60599,
#60600,#60601,#60602,#60603,#60604,#60605,#60606,#60607,#60608,#60609,#60610,
#60611,#60612,#60613,#60614,#60615,#60616,#60617,#60618,#60619,#60620,#60621,
#60622,#60623,#60624,#60625,#60626,#60627,#60628,#60629,#60630,#60631,#60632,
#60633,#60634,#60635,#60636,#60637,#60638,#60639,#60640,#60641,#60642,#60643,
#60644,#60645,#60646,#60647,#60648,#60649,#60650,#60651,#60652,#60653,#60654,
#60655,#60656,#60657,#60658,#60659,#60660,#60661,#60662,#60663,#60664,#60665,
#60666,#60667,#60668,#60669,#60670,#60671,#60672,#60673,#60674,#60675,#60676,
#60677,#60678,#60679,#60680,#60681,#60682,#60683,#60684,#60685,#60686,#60687,
#60688,#60689,#60690,#60691,#60692,#60693,#60694,#60695,#60696,#60697,#60698,
#60699,#60700,#60701,#60702,#60703,#60704,#60705,#60706,#60707,#60708,#60709,
#60710,#60711,#60712,#60713,#60714,#60715,#60716,#60717,#60718,#60719,#60720,
#60721,#60722,#60723,#60724,#60725,#60726,#60727,#60728,#60729,#60730,#60731,
#60732,#60733,#60734,#60735,#60736,#60737,#60738,#60739,#60740,#60741,#60742,
#60743,#60744,#60745,#60746,#60747,#60748,#60749,#60750,#60751,#60752,#60753,
#60754,#60755,#60756,#60757,#60758,#60759,#60760,#60761,#60762,#60763,#60764,
#60765,#60766,#60767,#60768,#60769,#60770,#60771,#60772,#60773,#60774,#60775,
#60776,#60777,#60778,#60779,#60780,#60781,#60782,#60783,#60784,#60785,#60786,
#60787,#60788,#60789,#60790,#60791,#60792,#60793,#60794,#60795,#60796,#60797,
#60798,#60799,#60800,#60801,#60802,#60803,#60804,#60805,#60806,#60807,#60808,
#60809,#60810,#60811,#60812,#60813,#60814,#60815,#60816,#60817,#60818,#60819,
#60820,#60821,#60822,#60823,#60824,#60825,#60826,#60827,#60828,#60829,#60830,
#60831,#60832,#60833,#60834,#60835,#60836,#60837,#60838,#60839,#60840,#60841,
#60842,#60843,#60844,#60845,#60846,#60847,#60848,#60849,#60850,#60851,#60852,
#60853,#60854,#60855,#60856,#60857,#60858,#60859,#60860,#60861,#60862,#60863,
#60864,#60865,#60866,#60867,#60868,#60869,#60870,#60871,#60872,#60873,#60874,
#60875,#60876,#60877,#60878,#60879,#60880,#60881,#60882,#60883,#60884,#60885,
#60886,#60887,#60888,#60889,#60890,#60891,#60892,#60893,#60894,#60895,#60896,
#60897,#60898,#60899,#60900,#60901,#60902,#60903,#60904,#60905,#60906,#60907,
#60908,#60909,#60910,#60911,#60912,#60913,#60914,#60915,#60916,#60917,#60918,
#60919,#60920,#60921,#60922,#60923,#60924,#60925,#60926,#60927,#60928,#60929,
#60930,#60931,#60932,#60933,#60934,#60935,#60936,#60937,#60938,#60939,#60940,
#60941,#60942,#60943,#60944,#60945,#60946,#60947,#60948,#60949,#60950,#60951,
#60952,#60953,#60954,#60955,#60956,#60957),.UNSPECIFIED.,.F.,.F.,(4,2,2,
2,2,2,2,2,2,2,2,2,2,2,2,2,2,2,2,2,2,2,2,2,2,2,2,2,2,2,2,2,2,2,2,2,2,2,2,
2,2,2,2,2,2,2,2,2,2,2,2,2,2,2,2,2,2,2,2,2,2,2,2,2,2,2,2,2,2,2,2,2,2,2,2,
2,2,2,2,2,2,2,2,2,2,2,2,2,2,2,2,2,2,2,2,2,2,2,2,2,2,2,2,2,2,2,2,2,2,2,2,
2,2,2,2,2,2,2,2,2,2,2,2,2,2,2,2,2,2,2,2,2,2,2,2,2,2,2,2,2,2,2,2,2,2,2,2,
2,2,2,2,2,2,2,2,2,2,2,2,2,2,2,2,2,2,2,2,2,2,2,2,2,2,2,2,2,2,2,2,2,2,2,2,
2,2,2,2,2,2,2,2,2,2,2,2,2,2,2,2,2,2,2,2,2,2,2,2,2,2,2,2,2,2,2,2,2,2,2,2,
2,2,2,2,2,2,2,2,2,2,2,2,2,2,2,2,2,2,2,2,2,2,2,2,2,2,2,2,2,2,2,2,2,2,2,2,
2,2,2,2,2,2,2,2,2,2,2,2,2,2,2,2,2,2,2,2,2,2,2,2,2,2,2,2,2,2,2,2,2,2,2,2,
2,2,2,2,2,2,2,2,2,2,2,2,2,2,2,2,4),(0.00211751522266133,0.0203487448140315,
0.0233396307185236,0.0253653093889092,0.0270336021014908,0.0286196489711016,
0.030659105402196,0.0341342840646406,0.0468442262904942,0.0571183188809527,
0.316321449506284,0.395751492788939,0.420267752109709,0.422876291006466,
0.424139781454416,0.425031367887155,0.425961656823417,0.427260319795774,
0.430647443332828,0.476474940746983,0.507710315873694,0.730301566755093,
0.787060668938419,0.815861512614544,0.826363351505926,0.831297980995632,
0.835260252259935,0.837013278865553,0.838714072668814,0.840397629460644,
0.842707959867446,0.848525574761595,0.915190192337002,1.00193201257549,
1.05720940702609,1.0729715832019,1.09121513166381,1.11291192374864,1.18937277439881,
1.22422821879501,1.23081620325662,1.23298393024763,1.2343801078656,1.23569248272775,
1.237414390011,1.2403197432154,1.25801580912919,1.4819056695185,1.59425643394248,
1.60454838385065,1.60866481023985,1.61155935843278,1.6143966928691,1.61836815298445,
1.62760665685734,1.76458571087279,1.81666939983119,1.92138790386485,1.97625768192028,
1.98455080994873,1.9869083107692,1.98834466710389,1.98964046489571,1.99129353898145,
1.99391139597964,2.00687735020665,2.21718586094031,2.31546325484413,2.35724971268514,
2.3712906343388,2.37741059905734,2.38212766163794,2.3844076171033,2.3861122670254,
2.38780253568542,2.39014582662124,2.39487937829662,2.4375911564596,2.43956161201346,
2.65576998447692,2.66686773035628,2.67909885614578,2.69280758762909,2.79330917507329,
2.79652034191443,2.79788984819507,2.79888806682704,2.79980973866556,2.80105993755311,
2.8041331024341,2.83525153894454,3.08501857729282,3.18479383091183,3.18919981722481,
3.19182092445397,3.19418461154305,3.19594794683303,3.19761428528336,3.19988210259741,
3.20549624124599,3.26457633020326,3.4932706543862,3.51121705408484,3.5339494150222,
3.58139667457577,3.58834186258623,3.59020584733558,3.59133489081425,3.59235211872347,
3.59364788731741,3.59628004112941,3.61192187379014,3.6137383468532,3.61469144542661,
3.61558556795375,3.61730132765294,3.78879717761604,3.89682821902251,3.97084445696559,
3.98271980814225,3.98608095971661,3.98812578930755,3.98996860745907,3.99231696832411,
3.99709176562342,4.02561526800418,4.05123023666428,4.27966376196531,4.33428677642955,
4.36075601936324,4.37482004753219,4.3772057779469,4.37846148719029,4.37948815117661,
4.38051936564364,4.38243297405945,4.38877492573883,4.39639657938534,4.62074094072661,
4.71407607525427,4.74784684285249,4.76599460048085,4.76982928282915,4.77196012567408,
4.7735856172384,4.77566988753082,4.77920066379627,4.7919121724557,4.98045649906709,
5.14409075109595,5.16606871388247,5.16867196448299,5.16997721804109,5.17092677626253,
5.17194666156686,5.17333154224294,5.17648855019712,5.28439301281565,5.54310583802784,
5.54628458262641,5.56038490960152,5.56404227423261,5.56614821749934,5.5677621494078,
5.56984391937517,5.57349180811749,5.58919852054118,5.76533791401445,5.78982001376208,
5.93634422093143,5.95748166191959,5.96033706293842,5.96165163101424,5.9626638106372,
5.96376152842931,5.96551659476634,5.97126070006308,6.00563847826581,6.05883319512685,
6.18077101822055,6.29721809301472,6.2996479486732,6.29999652052559,6.30043104665369,
6.30110290585124,6.30332587178196,6.30358048667121,6.30426593787041,6.30490516887891,
6.3510756476589,6.35652212497748,6.35873314166507,6.36057943820299,6.36247562674068,
6.36524872907727,6.37259017757667,6.47187054765089,6.58050447474925,6.66845716110728,
6.74607744046733,6.75086522706987,6.75257326311576,6.75356465897043,6.75449613534523,
6.75575726779103,6.75819951934292,6.76130053405256,6.89538876504119,6.91549323463673,
6.99076059734671,7.12886539503232,7.13834341256229,7.14155379664398,7.14336361679277,
7.14501742303726,7.14723246973909,7.15136649406493,7.17397342926271,7.21777182334469,
7.29472515593811,7.46594430939503,7.50457923786179,7.53534236269615,7.53854613213906,
7.53981025003095,7.54075677254305,7.54179618322441,7.54320406815022,7.5465293574908,
7.55111973660279,7.59885560848396,7.69077888710198,7.91515756527117,7.93015405108597,
7.9335248281765,7.9357208071321,7.93748768400637,7.93949484121496,7.94290534822238,
7.95619456365978,8.05092493716908,8.07868267668072,8.10007413126194,8.12447838308061,
8.24596209586379,8.32518337536583,8.33013098903248,8.3318280711429,8.33279014516939,
8.33367239690127,8.33460573872196,8.33650472997047,8.34410241683171,8.35740711634689,
8.38918401789272,8.46030480267807,8.72163530912242,8.72559484678511,8.7397273709299,
8.74335643954359,8.74543870407977,8.74703053515841,8.74907915527874,8.75265565819566,
8.76786106833943,8.79478730330389,8.90586407638577,8.92726267398728,8.94514962832429,
8.96047244303898,8.97381213396143,8.98556166739383,8.99600921616865,9.0053870515391,
9.09248539067258,9.10127087357609,9.1038711528879,9.13624403661262,9.13996784021801,
9.14167122072968,9.14297745772833,9.14418620214296,9.14616551954953,9.15143824292911,
9.15911227454543,9.18077152512064,9.23705469809105,9.49673734620167,9.5114402685722,
9.51635838158552,9.51911917847084,9.52188136759699,9.52531268356329,9.53190188606939,
9.57359579554831,9.6684620470765,9.82787860058392,9.83620678294941,9.85876088194946,
9.88984309728776,9.89365342576422,9.89537514938782,9.89668657238815,9.89789282009943,
9.89925572239684,9.90115071667791,9.9043124389687,9.95584215760787),
 .UNSPECIFIED.);
#529=B_SPLINE_CURVE_WITH_KNOTS('',3,(#60959,#60960,#60961,#60962,#60963,
#60964,#60965,#60966,#60967,#60968,#60969,#60970,#60971,#60972,#60973,#60974,
#60975,#60976,#60977,#60978,#60979,#60980,#60981,#60982,#60983,#60984,#60985,
#60986,#60987,#60988,#60989,#60990,#60991,#60992,#60993,#60994,#60995,#60996,
#60997,#60998,#60999,#61000,#61001,#61002,#61003,#61004,#61005,#61006,#61007,
#61008,#61009,#61010,#61011,#61012,#61013,#61014,#61015,#61016,#61017,#61018,
#61019,#61020,#61021,#61022,#61023,#61024,#61025,#61026,#61027,#61028,#61029,
#61030,#61031,#61032,#61033,#61034,#61035,#61036,#61037,#61038,#61039,#61040,
#61041,#61042,#61043,#61044,#61045,#61046,#61047,#61048,#61049,#61050,#61051,
#61052,#61053,#61054,#61055,#61056,#61057,#61058,#61059,#61060,#61061,#61062,
#61063,#61064,#61065,#61066,#61067,#61068,#61069,#61070,#61071,#61072,#61073,
#61074,#61075,#61076,#61077,#61078,#61079,#61080,#61081,#61082,#61083,#61084,
#61085,#61086,#61087,#61088,#61089,#61090,#61091,#61092,#61093,#61094,#61095,
#61096,#61097,#61098,#61099,#61100,#61101,#61102,#61103,#61104,#61105,#61106,
#61107,#61108,#61109,#61110,#61111,#61112,#61113,#61114,#61115,#61116,#61117,
#61118,#61119,#61120,#61121,#61122,#61123,#61124,#61125,#61126,#61127,#61128,
#61129,#61130,#61131,#61132,#61133,#61134,#61135,#61136,#61137,#61138,#61139,
#61140,#61141,#61142,#61143,#61144,#61145,#61146,#61147,#61148,#61149,#61150,
#61151,#61152,#61153,#61154,#61155,#61156,#61157,#61158,#61159,#61160,#61161,
#61162,#61163,#61164,#61165,#61166,#61167,#61168,#61169,#61170,#61171,#61172,
#61173,#61174,#61175,#61176,#61177,#61178,#61179,#61180,#61181,#61182,#61183,
#61184,#61185,#61186,#61187,#61188,#61189,#61190,#61191,#61192,#61193,#61194,
#61195,#61196,#61197,#61198,#61199,#61200,#61201,#61202,#61203,#61204,#61205,
#61206,#61207,#61208,#61209,#61210,#61211,#61212,#61213,#61214,#61215,#61216,
#61217,#61218,#61219,#61220),.UNSPECIFIED.,.F.,.F.,(4,3,3,3,3,3,3,3,3,3,
3,3,3,3,3,3,3,3,3,3,3,3,3,3,3,3,3,3,3,3,3,3,3,3,3,3,3,3,3,3,3,3,3,3,3,3,
3,3,3,3,3,3,3,3,3,3,3,3,3,3,3,3,3,3,3,3,3,3,3,3,3,3,3,3,3,3,3,3,3,3,3,3,
3,3,3,3,3,4),(-236.570517887855,-236.496478268965,-236.422511351756,-236.348602846773,
-236.274738505804,-236.200904112088,-236.127072919686,-236.053240372639,
-235.979393621018,-235.905519809121,-235.831563950077,-235.757564442011,
-235.683456355741,-235.624289900016,-235.550367529142,-235.476531943763,
-235.402768684695,-235.329063346266,-235.255401565183,-235.18176901024,
-235.108139222922,-235.034507269787,-234.960860197126,-234.887185044625,
-234.813429971543,-234.73963006972,-234.665729306294,-234.625881891966,
-234.551321119513,-234.476841179748,-234.402428159158,-234.32806818845,
-234.253747433568,-234.179452087123,-234.105155627678,-234.030854571707,
-233.956536429025,-233.882188702768,-233.807761847989,-233.733289599446,
-233.658721025371,-233.627473883915,-233.552913435452,-233.478433816586,
-233.404021113575,-233.329661456895,-233.255341012262,-233.181045972053,
-233.106749812024,-233.032449051203,-232.958131199188,-232.883783758897,
-232.809357181721,-232.73488520639,-232.660316896702,-232.629065875864,
-232.55517201873,-232.481360773344,-232.407617695596,-232.333928391571,
-232.260278506677,-232.186653715553,-232.113025476293,-232.03939121634,
-231.965737978926,-231.892052798438,-231.818281849421,-231.744462742115,
-231.67053769699,-231.630657867813,-231.556034821066,-231.481497510767,
-231.407032040494,-231.332624561216,-231.258261262204,-231.183928362384,
-231.109601917595,-231.035275603271,-230.960936961917,-230.886573531877,
-230.812138291546,-230.737661834807,-230.663095478887,-230.632249859762,
-230.54608776447,-230.46167604618,-230.374638762388,-230.287601478596),
 .UNSPECIFIED.);
#530=B_SPLINE_CURVE_WITH_KNOTS('',3,(#61222,#61223,#61224,#61225,#61226,
#61227,#61228,#61229,#61230,#61231,#61232,#61233,#61234,#61235,#61236,#61237,
#61238,#61239),.UNSPECIFIED.,.F.,.F.,(4,2,2,2,2,2,2,2,4),(-230.287601478596,
-229.452684566701,-228.617767654806,-227.782850742911,-226.947933831016,
-226.113016919122,-225.278100007227,-224.443183095332,-224.004416171416),
 .UNSPECIFIED.);
#531=B_SPLINE_CURVE_WITH_KNOTS('',3,(#61241,#61242,#61243,#61244,#61245,
#61246,#61247,#61248,#61249,#61250,#61251),.UNSPECIFIED.,.F.,.F.,(4,1,1,
1,1,1,1,1,4),(-224.004416171416,-223.643393803405,-223.14418979938,-222.644985795355,
-221.646577787304,-220.648169779253,-219.649761771202,-218.651353763151,
-217.72156918778),.UNSPECIFIED.);
#532=B_SPLINE_CURVE_WITH_KNOTS('',3,(#61253,#61254,#61255,#61256,#61257,
#61258,#61259,#61260,#61261,#61262,#61263,#61264,#61265,#61266,#61267,#61268,
#61269,#61270,#61271,#61272,#61273,#61274,#61275,#61276,#61277,#61278,#61279,
#61280,#61281,#61282,#61283,#61284,#61285,#61286,#61287,#61288,#61289,#61290,
#61291,#61292,#61293,#61294,#61295,#61296,#61297,#61298,#61299,#61300,#61301,
#61302,#61303,#61304,#61305,#61306,#61307,#61308,#61309,#61310,#61311,#61312,
#61313,#61314,#61315,#61316,#61317,#61318,#61319,#61320,#61321,#61322,#61323,
#61324,#61325,#61326,#61327,#61328,#61329,#61330,#61331,#61332,#61333,#61334,
#61335,#61336,#61337,#61338,#61339,#61340,#61341,#61342,#61343,#61344,#61345,
#61346,#61347,#61348,#61349,#61350,#61351,#61352,#61353,#61354,#61355,#61356,
#61357,#61358,#61359,#61360,#61361,#61362,#61363,#61364,#61365,#61366,#61367,
#61368,#61369,#61370,#61371,#61372,#61373,#61374,#61375,#61376,#61377,#61378,
#61379,#61380,#61381,#61382,#61383,#61384,#61385,#61386,#61387,#61388,#61389,
#61390,#61391,#61392,#61393,#61394,#61395,#61396,#61397,#61398,#61399,#61400,
#61401,#61402,#61403,#61404,#61405,#61406,#61407,#61408,#61409,#61410,#61411,
#61412,#61413,#61414,#61415,#61416,#61417,#61418,#61419,#61420,#61421,#61422,
#61423,#61424,#61425,#61426,#61427,#61428,#61429,#61430,#61431,#61432,#61433,
#61434,#61435,#61436,#61437,#61438,#61439,#61440,#61441,#61442,#61443,#61444,
#61445,#61446,#61447,#61448,#61449,#61450,#61451,#61452,#61453,#61454,#61455,
#61456,#61457,#61458,#61459,#61460,#61461,#61462,#61463,#61464,#61465,#61466,
#61467,#61468,#61469,#61470,#61471,#61472,#61473,#61474,#61475,#61476,#61477,
#61478,#61479,#61480,#61481,#61482,#61483,#61484,#61485,#61486,#61487,#61488,
#61489,#61490,#61491,#61492,#61493,#61494,#61495,#61496,#61497,#61498,#61499,
#61500,#61501,#61502,#61503,#61504,#61505,#61506,#61507,#61508,#61509,#61510,
#61511,#61512,#61513,#61514,#61515,#61516,#61517,#61518,#61519,#61520,#61521,
#61522,#61523,#61524,#61525,#61526,#61527,#61528,#61529,#61530,#61531,#61532,
#61533,#61534,#61535,#61536,#61537,#61538,#61539,#61540,#61541,#61542,#61543,
#61544,#61545,#61546,#61547,#61548,#61549,#61550,#61551,#61552,#61553,#61554,
#61555,#61556,#61557,#61558,#61559,#61560,#61561,#61562,#61563,#61564,#61565,
#61566,#61567,#61568,#61569,#61570,#61571,#61572,#61573,#61574,#61575,#61576,
#61577,#61578,#61579,#61580,#61581,#61582,#61583,#61584,#61585,#61586,#61587,
#61588,#61589,#61590,#61591,#61592,#61593,#61594,#61595,#61596,#61597,#61598,
#61599,#61600,#61601,#61602,#61603,#61604,#61605,#61606,#61607,#61608,#61609,
#61610,#61611,#61612,#61613,#61614,#61615,#61616,#61617,#61618,#61619,#61620,
#61621,#61622,#61623,#61624,#61625,#61626,#61627,#61628,#61629,#61630,#61631,
#61632,#61633,#61634,#61635,#61636,#61637,#61638,#61639,#61640,#61641,#61642,
#61643,#61644,#61645,#61646,#61647,#61648,#61649,#61650,#61651,#61652,#61653,
#61654,#61655,#61656,#61657,#61658,#61659,#61660,#61661,#61662,#61663,#61664,
#61665,#61666,#61667,#61668,#61669,#61670,#61671,#61672,#61673,#61674,#61675,
#61676,#61677,#61678,#61679,#61680,#61681,#61682,#61683,#61684,#61685,#61686,
#61687,#61688,#61689,#61690,#61691,#61692,#61693,#61694,#61695,#61696,#61697,
#61698,#61699,#61700,#61701,#61702,#61703,#61704,#61705,#61706,#61707,#61708,
#61709,#61710,#61711,#61712,#61713,#61714,#61715,#61716,#61717,#61718,#61719,
#61720,#61721,#61722,#61723,#61724,#61725,#61726,#61727,#61728,#61729,#61730,
#61731,#61732,#61733,#61734,#61735,#61736,#61737,#61738,#61739,#61740,#61741,
#61742,#61743,#61744,#61745,#61746,#61747,#61748,#61749,#61750,#61751,#61752,
#61753,#61754,#61755,#61756,#61757,#61758,#61759,#61760,#61761,#61762,#61763,
#61764,#61765,#61766,#61767,#61768,#61769,#61770,#61771,#61772,#61773,#61774,
#61775,#61776,#61777,#61778,#61779,#61780,#61781,#61782,#61783,#61784,#61785,
#61786,#61787,#61788,#61789,#61790,#61791,#61792,#61793,#61794,#61795,#61796,
#61797,#61798,#61799,#61800,#61801,#61802,#61803,#61804,#61805,#61806,#61807,
#61808,#61809,#61810,#61811,#61812,#61813,#61814,#61815,#61816,#61817,#61818,
#61819,#61820,#61821,#61822,#61823,#61824,#61825,#61826,#61827,#61828,#61829,
#61830,#61831,#61832,#61833,#61834,#61835,#61836,#61837,#61838,#61839,#61840),
 .UNSPECIFIED.,.F.,.F.,(4,2,2,2,2,2,2,2,2,2,2,2,2,2,2,2,2,2,2,2,2,2,2,2,
2,2,2,2,2,2,2,2,2,2,2,2,2,2,2,2,2,2,2,2,2,2,2,2,2,2,2,2,2,2,2,2,2,2,2,2,
2,2,2,2,2,2,2,2,2,2,2,2,2,2,2,2,2,2,2,2,2,2,2,2,2,2,2,2,2,2,2,2,2,2,2,2,
2,2,2,2,2,2,2,2,2,2,2,2,2,2,2,2,2,2,2,2,2,2,2,2,2,2,2,2,2,2,2,2,2,2,2,2,
2,2,2,2,2,2,2,2,2,2,2,2,2,2,2,2,2,2,2,2,2,2,2,2,2,2,2,2,2,2,2,2,2,2,2,2,
2,2,2,2,2,2,2,2,2,2,2,2,2,2,2,2,2,2,2,2,2,2,2,2,2,2,2,2,2,2,2,2,2,2,2,2,
2,2,2,2,2,2,2,2,2,2,2,2,2,2,2,2,2,2,2,2,2,2,2,2,2,2,2,2,2,2,2,2,2,2,2,2,
2,2,2,2,2,2,2,2,2,2,2,2,2,2,2,2,2,2,2,2,2,2,2,2,2,2,2,2,2,2,2,2,2,2,2,2,
2,2,2,2,2,2,2,2,2,2,2,2,2,2,2,2,2,4),(0.00206310016479781,0.0503830808988502,
0.0524268792653076,0.0537113840937123,0.0546855606875728,0.0556157387795359,
0.0565331450836818,0.0577822267195454,0.0608769462524458,0.0935667358570958,
0.1050112952103,0.111035653215168,0.314970378675905,0.401194488205747,0.438624331519552,
0.461707117851576,0.465769564042696,0.467926747858301,0.469528949649375,
0.471273994897825,0.47434733835435,0.483275900280479,0.615286404134497,
0.779705853341372,0.809798541705046,0.853665089400275,0.861264784104124,
0.863554516051205,0.864772757973366,0.865954029160069,0.867445851268963,
0.870051938062555,0.880138893397435,0.924874815266039,0.936994950550609,
0.994714499242434,1.2123573467069,1.23277386820493,1.23812548660565,1.24130270669334,
1.24411220545776,1.24759068569905,1.25290262742621,1.27631830806268,1.48964407782103,
1.55146882682353,1.60674164603289,1.61508168623236,1.61745016216806,1.61867848455857,
1.61994433840325,1.62144310093537,1.62407871012408,1.63444026869955,1.77621953920154,
1.78426404396731,1.79278687508964,1.80185911913089,1.81161153821605,1.82273199832761,
1.83565044281444,1.8760704311336,1.97107068491241,2.0076309153499,2.01217817501339,
2.01443619117316,2.01605140115547,2.01775300509979,2.02060734889288,2.02807630094551,
2.03850181331873,2.27302087060922,2.33280349377825,2.38408334667411,2.42022489038964,
2.42410898851928,2.42612583156773,2.42739626748279,2.4285707187389,2.42952722188195,
2.43050431717203,2.43228148880858,2.43784170035034,2.52175079767785,2.66773110152632,
2.68062829070292,2.69527981906675,2.71238587228607,2.73332634436571,2.80813180918227,
2.81989523498609,2.82315863662191,2.82512998084907,2.82689754568116,2.82913766797792,
2.8326592287791,2.84966268797417,3.11256124669895,3.18219832174056,3.21388663176762,
3.21748591363248,3.21940002903702,3.221038478741,3.22209825401321,3.22312074147338,
3.22445873952079,3.22740134016791,3.25034111695839,3.25843999198882,3.27085456177941,
3.51214882728638,3.53475104444254,3.6047200735571,3.61619208221541,3.61950899512696,
3.62154231425786,3.62338483797292,3.62574679157748,3.63043574870699,3.65853730710928,
3.67356311277806,3.69050409043141,3.70590656980858,3.91032771053457,3.96549540892021,
4.00215786217311,4.00819452700101,4.01001600897586,4.0111499157126,4.01219311549608,
4.01354440980433,4.01578683988271,4.02849820005397,4.26180438945362,4.35871582069006,
4.3928242017781,4.39741112977155,4.39971954046507,4.40138299013086,4.40314672016327,
4.4056309907901,4.41224320552322,4.51384354609371,4.63504977813863,4.79018231719396,
4.79696018365848,4.798832716037,4.79996187339252,4.80097293518431,4.80225232568065,
4.80427852685768,4.81464032610943,4.9804847213518,5.17699161328337,5.19028798177488,
5.19382180852563,5.19587441880517,5.19761605201889,5.19973372719817,5.20366129217755,
5.22457098790241,5.26514513426225,5.32120287336182,5.44559659092256,5.58052483305719,
5.58928706209074,5.59118928099527,5.59241515470495,5.59339298482172,5.59450014689056,
5.5963939414982,5.60392141263613,5.66015899823546,5.7215552360471,5.77432099869787,
5.935069984782,5.99637252378493,6.00207093649415,6.00436045967791,6.00603843468076,
6.00784625333532,6.01028511648299,6.01577378256877,6.16866215801806,6.38430459804151,
6.39765430389124,6.40030628043358,6.40197341546939,6.40327551592991,6.40471404085846,
6.4070641912719,6.41522512405134,6.46852745557286,6.60612801272068,6.76284545390843,
6.77271232154962,6.77681114385611,6.77969007276274,6.78258451836723,6.7866260816601,
6.79636235057872,6.93074609026676,7.12197422784265,7.15032312910918,7.1540446765417,
7.15575265618913,7.15706465232665,7.15847040969394,7.1606736765203,7.16752856212847,
7.2046198739944,7.24680847773683,7.34191888203779,7.52801785552134,7.54619237175491,
7.54981657912374,7.55209781692984,7.55388260738899,7.55581775232708,7.55894617490725,
7.56264338306019,7.56974643342612,7.74261913193179,7.94333614781604,7.96217241167257,
7.9646072101625,7.96584979040548,7.96676565124097,7.96776589714003,7.96914230870995,
7.97235786706012,8.06367268210611,8.08306778812237,8.11984415901366,8.14127209378237,
8.14974394819524,8.15773510773838,8.16529839580869,8.27254291014769,8.35295157072723,
8.35902442377338,8.36136680065576,8.36305015096787,8.36479717037477,8.36708132604246,
8.36959434710459,8.37374464171974,8.38208473358466,8.403355825419,8.4988422555759,
8.73452908597825,8.75501855572248,8.75781282705858,8.75911342753162,8.76013015564565,
8.76123710290569,8.76300947734345,8.76883235216942,8.80381803636421,8.88752819026766,
8.94302869918772,9.01134908143064,9.0542897768729,9.14819909920552,9.15468928526942,
9.157154366426,9.15891331450244,9.16072757532108,9.16308176044369,9.16566544862633,
9.16990964051844,9.17838792908977,9.19986146006793,9.29844891000985,9.53174040719135,
9.54452699237474,9.54677433952639,9.54812730814649,9.5491710263944,9.55030470425575,
9.55212414289312,9.55813928698537,9.59458800176715,9.64485976923376,9.91441346941936,
9.92561650147807,9.9335914794583,9.93657942754645,9.93834386281007,9.94011759325285,
9.94190715232923,9.94420607027357,9.95041883173145,9.95922074868957),
 .UNSPECIFIED.);
#533=B_SPLINE_CURVE_WITH_KNOTS('',3,(#61842,#61843,#61844,#61845,#61846,
#61847,#61848,#61849,#61850,#61851,#61852,#61853,#61854,#61855,#61856,#61857,
#61858,#61859,#61860,#61861,#61862,#61863,#61864,#61865,#61866,#61867,#61868,
#61869,#61870,#61871,#61872,#61873,#61874,#61875,#61876,#61877,#61878,#61879,
#61880,#61881,#61882,#61883,#61884,#61885,#61886,#61887,#61888,#61889,#61890,
#61891,#61892,#61893,#61894,#61895,#61896,#61897,#61898,#61899,#61900,#61901,
#61902,#61903,#61904,#61905,#61906,#61907,#61908,#61909,#61910,#61911,#61912,
#61913,#61914,#61915,#61916,#61917,#61918,#61919,#61920,#61921,#61922,#61923,
#61924,#61925,#61926,#61927,#61928,#61929,#61930,#61931,#61932,#61933,#61934,
#61935,#61936,#61937,#61938,#61939,#61940,#61941,#61942,#61943,#61944,#61945,
#61946,#61947,#61948,#61949,#61950,#61951,#61952,#61953,#61954,#61955,#61956,
#61957,#61958,#61959,#61960,#61961,#61962,#61963,#61964,#61965,#61966,#61967,
#61968,#61969,#61970,#61971,#61972,#61973,#61974,#61975,#61976,#61977,#61978,
#61979,#61980,#61981,#61982,#61983,#61984,#61985,#61986,#61987,#61988,#61989,
#61990,#61991,#61992,#61993,#61994,#61995,#61996,#61997,#61998,#61999,#62000,
#62001,#62002,#62003,#62004,#62005,#62006,#62007,#62008,#62009,#62010,#62011,
#62012,#62013,#62014,#62015,#62016,#62017,#62018,#62019,#62020,#62021,#62022,
#62023,#62024,#62025,#62026,#62027,#62028,#62029,#62030,#62031,#62032,#62033,
#62034,#62035,#62036,#62037,#62038,#62039,#62040,#62041,#62042,#62043,#62044,
#62045,#62046,#62047,#62048,#62049,#62050,#62051,#62052,#62053,#62054,#62055,
#62056,#62057,#62058,#62059,#62060,#62061,#62062,#62063,#62064,#62065,#62066,
#62067,#62068,#62069,#62070,#62071,#62072,#62073,#62074,#62075,#62076,#62077,
#62078,#62079,#62080,#62081,#62082,#62083,#62084,#62085,#62086,#62087,#62088,
#62089,#62090,#62091,#62092,#62093,#62094,#62095,#62096,#62097,#62098,#62099,
#62100,#62101,#62102,#62103,#62104,#62105,#62106,#62107,#62108,#62109,#62110,
#62111,#62112,#62113,#62114,#62115,#62116,#62117,#62118,#62119,#62120,#62121,
#62122,#62123,#62124,#62125,#62126,#62127,#62128,#62129,#62130,#62131,#62132,
#62133,#62134,#62135,#62136,#62137,#62138,#62139,#62140,#62141,#62142,#62143,
#62144,#62145,#62146,#62147,#62148,#62149,#62150,#62151,#62152,#62153,#62154,
#62155,#62156,#62157,#62158,#62159,#62160,#62161,#62162,#62163,#62164,#62165,
#62166,#62167,#62168,#62169,#62170,#62171,#62172,#62173,#62174,#62175,#62176,
#62177,#62178,#62179,#62180,#62181,#62182,#62183,#62184,#62185,#62186,#62187,
#62188,#62189,#62190,#62191,#62192,#62193,#62194,#62195,#62196,#62197,#62198,
#62199,#62200,#62201,#62202,#62203,#62204,#62205,#62206,#62207,#62208,#62209,
#62210,#62211,#62212,#62213,#62214,#62215,#62216,#62217,#62218,#62219,#62220,
#62221,#62222,#62223,#62224,#62225,#62226,#62227,#62228,#62229,#62230,#62231,
#62232,#62233,#62234,#62235,#62236,#62237,#62238,#62239,#62240,#62241,#62242,
#62243,#62244,#62245,#62246,#62247,#62248,#62249,#62250,#62251,#62252,#62253,
#62254,#62255,#62256,#62257,#62258,#62259,#62260,#62261,#62262,#62263,#62264,
#62265,#62266,#62267,#62268,#62269,#62270,#62271,#62272,#62273,#62274,#62275,
#62276,#62277,#62278,#62279,#62280,#62281,#62282,#62283,#62284,#62285,#62286,
#62287,#62288,#62289,#62290,#62291,#62292,#62293,#62294,#62295,#62296,#62297,
#62298,#62299,#62300,#62301,#62302,#62303,#62304,#62305,#62306,#62307,#62308,
#62309,#62310,#62311,#62312,#62313,#62314,#62315,#62316,#62317,#62318,#62319,
#62320,#62321,#62322,#62323,#62324,#62325,#62326,#62327,#62328,#62329,#62330,
#62331,#62332,#62333,#62334,#62335,#62336,#62337,#62338,#62339,#62340,#62341,
#62342,#62343,#62344,#62345,#62346,#62347,#62348,#62349,#62350,#62351,#62352,
#62353,#62354,#62355,#62356,#62357,#62358,#62359,#62360,#62361,#62362,#62363,
#62364,#62365,#62366,#62367,#62368,#62369,#62370,#62371,#62372,#62373,#62374,
#62375,#62376,#62377,#62378,#62379,#62380,#62381,#62382,#62383,#62384,#62385,
#62386,#62387,#62388,#62389,#62390,#62391,#62392,#62393,#62394,#62395,#62396,
#62397,#62398,#62399,#62400,#62401,#62402,#62403,#62404,#62405,#62406,#62407),
 .UNSPECIFIED.,.F.,.F.,(4,2,2,2,2,2,2,2,2,2,2,2,2,2,2,2,2,2,2,2,2,2,2,2,
2,2,2,2,2,2,2,2,2,2,2,2,2,2,2,2,2,2,2,2,2,2,2,2,2,2,2,2,2,2,2,2,2,2,2,2,
2,2,2,2,2,2,2,2,2,2,2,2,2,2,2,2,2,2,2,2,2,2,2,2,2,2,2,2,2,2,2,2,2,2,2,2,
2,2,2,2,2,2,2,2,2,2,2,2,2,2,2,2,2,2,2,2,2,2,2,2,2,2,2,2,2,2,2,2,2,2,2,2,
2,2,2,2,2,2,2,2,2,2,2,2,2,2,2,2,2,2,2,2,2,2,2,2,2,2,2,2,2,2,2,2,2,2,2,2,
2,2,2,2,2,2,2,2,2,2,2,2,2,2,2,2,2,2,2,2,2,2,2,2,2,2,2,2,2,2,2,2,2,2,2,2,
2,2,2,2,2,2,2,2,2,2,2,2,2,2,2,2,2,2,2,2,2,2,2,2,2,2,2,2,2,2,2,2,2,2,2,2,
2,2,2,2,2,2,2,2,2,2,2,2,2,2,2,2,2,2,2,2,2,2,2,2,2,2,2,2,2,2,2,2,2,2,2,2,
2,2,2,2,2,2,4),(0.00297604451504543,0.307437594455464,0.371161582836229,
0.379255930588295,0.381247520469777,0.382403600670181,0.383309176057065,
0.384345273648609,0.386278223922282,0.393296840400095,0.395251204720802,
0.398779986928545,0.593253181120357,0.691488307478245,0.743883918454952,
0.762198970999362,0.769655411505022,0.773477566485675,0.775853344079466,
0.778038881741714,0.779772412711776,0.781493345206249,0.78449037278834,
0.792982494912627,0.915805534751877,0.979539837164022,1.10465434478413,
1.17036313763555,1.1735306101825,1.17489870280763,1.17589756473639,1.17681548228123,
1.17806592797039,1.18116733851056,1.21409251601541,1.21593559283684,1.22744211855453,
1.44952133152978,1.52092898355953,1.55842920282579,1.57395891958729,1.58056674656611,
1.58558795220044,1.58793303887868,1.58962626431515,1.59129807907288,1.59356216125344,
1.59911117744845,1.65484153748527,1.79242955617571,1.89923289445484,1.95089881172431,
1.97005669899383,1.98111263644824,1.98372308061504,1.98521991715767,1.98638393472394,
1.98790746088799,1.99056597055898,2.00096940227494,2.22509849381014,2.34676947668228,
2.35626025360985,2.36026027329891,2.36314700288535,2.36603848037698,2.36964317389163,
2.37856060223993,2.48473765140089,2.64649835660391,2.73302726055399,2.73695610015258,
2.7387215099047,2.74003802516155,2.74126542759059,2.74294856164591,2.74628966608516,
2.77775701226603,2.78175289936853,2.78928274531461,3.00484017421296,3.12598854685781,
3.13021172120628,3.13276123370063,3.13507577787528,3.13671210928667,3.13838279165264,
3.1406434214609,3.14504422548245,3.17816986231892,3.46132153087943,3.54456974636974,
3.54800428252614,3.54941266875121,3.55041630498528,3.55132839782235,3.55254522833223,
3.55562205260018,3.58479459260071,3.62643865815275,3.74345924115258,3.8530262304217,
3.92922045931211,3.94111141824744,3.94438767945159,3.94636210433657,3.9481294400624,
3.95036521914059,3.95387211645877,3.97067168829991,4.25778194441792,4.3039555196626,
4.33541480080938,4.34081291708075,4.34251147315146,4.34360100664821,4.3446241634064,
4.34596504757275,4.34892217336037,4.37224606333591,4.37340568177209,4.37854279327014,
4.6074609443119,4.66508628406531,4.7272497041009,4.73789784371986,4.74112600388234,
4.74313979742355,4.74498806245511,4.74735078358507,4.75233381235465,4.78517478513079,
4.80684465962293,4.98433108496847,5.12055812093897,5.1291405271459,5.13109510562046,
5.13237296979,5.13330232349179,5.13445752615367,5.13637327528557,5.1433083719927,
5.18927518278472,5.2668165488979,5.46399155217598,5.47532633709226,5.51340949858671,
5.51809439553617,5.52046418719999,5.52219792213742,5.52406292820472,5.52657398371105,
5.53220466867101,5.67642466639299,5.72053638009082,5.76500723477777,5.90896649712754,
5.91417333741174,5.91896864453272,5.9206743033543,5.92165729671086,5.92256875403068,
5.92380933825557,5.92622024849291,5.94295877815542,6.00738768862343,6.29512649075997,
6.31187547115639,6.31537819654718,6.31761247268939,6.31937936536836,6.32135407368037,
6.32463261972384,6.33655099305369,6.41305219834724,6.49526811434365,6.56925826906714,
6.69111758263847,6.71042500927461,6.71316101123142,6.71443528017928,6.71542196401978,
6.71646875238109,6.71813284813966,6.72009355819043,6.72383004418041,6.75773049938111,
6.8266694698301,7.10388523573989,7.10798986267781,7.12239621138787,7.12572980339555,
7.12792063962473,7.12969612359525,7.131726991057,7.13521221963925,7.14922218997859,
7.25763239225117,7.4131035066815,7.51399770638478,7.5211549643648,7.52348475684752,
7.52477484031725,7.52596616939829,7.52748700439794,7.52911928285559,7.53166135700761,
7.57745200546682,7.63557718244864,7.76599743200456,7.88612986163292,7.89523816174119,
7.89887334340797,7.90153171623142,7.90438066997776,7.90816976331211,7.91648526544872,
7.92741268943911,7.98828338399325,8.03065488990954,8.06294655311029,8.21280309397782,
8.2541827693215,8.27287353881204,8.27609479471951,8.27775780835643,8.2790327298689,
8.28043597663861,8.28189482683876,8.28402014868918,8.28773580088015,8.38895564237337,
8.65202188565386,8.66852788552615,8.67203001351949,8.67427312774102,8.67605300868926,
8.6780485304051,8.68137639368066,8.69363168376002,8.77323978297454,8.84243184117943,
8.86339574401253,8.88090405450091,8.89586133592198,8.90883022829153,8.92019388978084,
8.93023225685929,8.93916413156648,9.01647757493111,9.06093313200018,9.08345251082273,
9.08630076212298,9.08759082221684,9.08857785133288,9.08949221786674,9.09053709880988,
9.0934679614785,9.1280133170749,9.18304705224816,9.39561539070965,9.47449716416361,
9.48053747718202,9.48287356665185,9.48455452351055,9.48615841483564,9.48841403280086,
9.49300685956648,9.53261967100893,9.64047168806455,9.7997260697482,9.8064626528913,
9.82537131618962,9.87484558918037,9.87831908295523,9.87964774310392,9.8806071984042,
9.88157659059722,9.8825689995385,9.88385749356293,9.88587848619483,9.90123656120509,
9.96079208582225),.UNSPECIFIED.);
#534=B_SPLINE_CURVE_WITH_KNOTS('',3,(#62409,#62410,#62411,#62412,#62413,
#62414,#62415,#62416,#62417,#62418,#62419,#62420,#62421,#62422,#62423,#62424,
#62425,#62426,#62427,#62428,#62429,#62430,#62431,#62432,#62433,#62434,#62435,
#62436,#62437,#62438,#62439,#62440,#62441,#62442,#62443,#62444,#62445,#62446,
#62447,#62448,#62449,#62450,#62451,#62452,#62453,#62454,#62455,#62456,#62457,
#62458,#62459,#62460,#62461,#62462,#62463,#62464,#62465,#62466,#62467,#62468,
#62469,#62470,#62471,#62472,#62473,#62474,#62475,#62476,#62477,#62478,#62479,
#62480,#62481,#62482,#62483,#62484,#62485,#62486,#62487,#62488,#62489,#62490,
#62491,#62492,#62493,#62494,#62495,#62496,#62497,#62498,#62499,#62500,#62501,
#62502,#62503,#62504,#62505,#62506,#62507,#62508,#62509,#62510,#62511,#62512,
#62513,#62514,#62515,#62516,#62517,#62518,#62519,#62520,#62521,#62522,#62523,
#62524,#62525,#62526,#62527,#62528,#62529,#62530,#62531,#62532,#62533,#62534,
#62535,#62536,#62537,#62538,#62539,#62540,#62541,#62542,#62543,#62544,#62545,
#62546,#62547,#62548,#62549,#62550,#62551,#62552,#62553,#62554,#62555,#62556,
#62557,#62558,#62559,#62560,#62561,#62562,#62563,#62564,#62565,#62566,#62567,
#62568,#62569,#62570,#62571,#62572,#62573,#62574,#62575,#62576,#62577,#62578,
#62579,#62580,#62581,#62582,#62583,#62584,#62585,#62586,#62587,#62588,#62589,
#62590,#62591,#62592,#62593,#62594,#62595,#62596,#62597,#62598,#62599,#62600,
#62601,#62602,#62603,#62604,#62605,#62606,#62607,#62608,#62609,#62610,#62611,
#62612,#62613,#62614,#62615,#62616,#62617,#62618,#62619,#62620,#62621,#62622,
#62623,#62624,#62625,#62626,#62627,#62628,#62629,#62630,#62631,#62632,#62633,
#62634,#62635,#62636,#62637,#62638,#62639,#62640,#62641,#62642,#62643,#62644,
#62645,#62646,#62647,#62648,#62649,#62650,#62651,#62652,#62653,#62654,#62655,
#62656,#62657,#62658,#62659,#62660,#62661,#62662,#62663,#62664,#62665,#62666,
#62667,#62668,#62669,#62670,#62671,#62672,#62673),.UNSPECIFIED.,.F.,.F.,
(4,3,3,3,3,3,3,3,3,3,3,3,3,3,3,3,3,3,3,3,3,3,3,3,3,3,3,3,3,3,3,3,3,3,3,
3,3,3,3,3,3,3,3,3,3,3,3,3,3,3,3,3,3,3,3,3,3,3,3,3,3,3,3,3,3,3,3,3,3,3,3,
3,3,3,3,3,3,3,3,3,3,3,3,3,3,3,3,3,4),(-192.588489635518,-192.514976588221,
-192.441536697609,-192.368155301087,-192.294817783453,-192.219757753744,
-192.146453138469,-192.073145745637,-191.999822398974,-191.923451185674,
-191.850020602564,-191.776543231949,-191.702976492768,-191.694337545776,
-191.619776559642,-191.545296395256,-191.470883139413,-191.39652292312,
-191.322201912616,-191.247906300795,-191.173609562286,-191.099308218751,
-191.024989780242,-190.95064175013,-190.876214580866,-190.801742011321,
-190.727173108861,-190.695929537725,-190.622036056471,-190.548225190329,
-190.474482494906,-190.400793576011,-190.327144078784,-190.2535196776,-190.179891830674,
-190.106257964606,-190.032605122391,-189.958920338183,-189.885149785285,
-189.81133107467,-189.737406423803,-189.697521529674,-189.62289846426,-189.548361135379,
-189.473895646626,-189.399488148984,-189.325124831742,-189.250791913841,
-189.176465451246,-189.102139119291,-189.027800460494,-188.953437013215,
-188.879001756033,-188.804525282641,-188.7299589105,-188.699113521623,-188.620747847582,
-188.542478678145,-188.464300731748,-188.386239959557,-188.308250897303,
-188.230351044309,-188.199909517598,-188.121998929484,-188.04401853258,
-187.965963202718,-187.887778486963,-187.809523107355,-187.731148416719,
-187.700705513572,-187.626146417045,-187.551662767433,-187.477240704328,
-187.40286640789,-187.328526090098,-187.254205986351,-187.179877117193,
-187.105538884002,-187.031178825652,-186.95678447185,-186.882304118277,
-186.807774365277,-186.733142634435,-186.702297505521,-186.619885579121,
-186.537828525829,-186.455989679252,-186.374521751061,-186.305304328339),
 .UNSPECIFIED.);
#535=B_SPLINE_CURVE_WITH_KNOTS('',3,(#62675,#62676,#62677,#62678,#62679,
#62680,#62681,#62682,#62683,#62684,#62685,#62686,#62687,#62688,#62689,#62690,
#62691,#62692),.UNSPECIFIED.,.F.,.F.,(4,2,2,2,2,2,2,2,4),(-186.305304328339,
-185.470387416444,-184.635470504549,-183.800553592654,-182.965636680759,
-182.130719768864,-181.29580285697,-180.460885945075,-180.022119021159),
 .UNSPECIFIED.);
#536=B_SPLINE_CURVE_WITH_KNOTS('',3,(#62694,#62695,#62696,#62697,#62698,
#62699,#62700,#62701,#62702,#62703,#62704,#62705,#62706,#62707,#62708,#62709,
#62710,#62711,#62712,#62713,#62714,#62715,#62716,#62717,#62718,#62719,#62720,
#62721,#62722,#62723,#62724,#62725,#62726,#62727,#62728,#62729,#62730,#62731,
#62732,#62733,#62734,#62735,#62736,#62737,#62738,#62739,#62740,#62741,#62742,
#62743,#62744,#62745,#62746,#62747,#62748,#62749,#62750,#62751,#62752,#62753,
#62754,#62755,#62756,#62757,#62758,#62759,#62760,#62761,#62762,#62763,#62764,
#62765,#62766,#62767,#62768,#62769,#62770,#62771,#62772,#62773,#62774,#62775,
#62776,#62777,#62778,#62779,#62780,#62781,#62782,#62783,#62784,#62785,#62786,
#62787,#62788,#62789,#62790,#62791,#62792,#62793,#62794,#62795,#62796,#62797,
#62798,#62799,#62800,#62801,#62802,#62803,#62804,#62805,#62806,#62807,#62808,
#62809,#62810,#62811,#62812,#62813,#62814,#62815,#62816,#62817,#62818,#62819,
#62820,#62821,#62822,#62823,#62824,#62825,#62826,#62827,#62828,#62829,#62830,
#62831,#62832,#62833,#62834,#62835,#62836,#62837,#62838,#62839,#62840,#62841,
#62842,#62843,#62844,#62845,#62846,#62847,#62848,#62849,#62850,#62851,#62852,
#62853,#62854,#62855,#62856,#62857,#62858,#62859,#62860,#62861,#62862,#62863,
#62864,#62865,#62866,#62867,#62868,#62869,#62870,#62871,#62872,#62873,#62874,
#62875,#62876,#62877,#62878,#62879,#62880,#62881,#62882,#62883,#62884,#62885,
#62886,#62887,#62888,#62889,#62890,#62891,#62892,#62893,#62894,#62895,#62896,
#62897,#62898,#62899,#62900,#62901,#62902,#62903,#62904,#62905,#62906,#62907,
#62908,#62909,#62910,#62911,#62912,#62913,#62914,#62915,#62916,#62917,#62918,
#62919,#62920,#62921,#62922,#62923,#62924,#62925,#62926,#62927,#62928,#62929,
#62930,#62931,#62932,#62933,#62934,#62935,#62936,#62937,#62938,#62939,#62940,
#62941,#62942,#62943,#62944,#62945,#62946,#62947,#62948,#62949,#62950,#62951,
#62952,#62953,#62954,#62955,#62956,#62957,#62958,#62959,#62960,#62961,#62962,
#62963,#62964,#62965,#62966,#62967,#62968,#62969,#62970,#62971,#62972,#62973,
#62974,#62975,#62976,#62977,#62978,#62979,#62980,#62981,#62982,#62983,#62984,
#62985,#62986,#62987,#62988,#62989,#62990,#62991,#62992,#62993,#62994,#62995,
#62996,#62997,#62998,#62999,#63000,#63001,#63002,#63003,#63004,#63005,#63006,
#63007,#63008,#63009,#63010,#63011,#63012,#63013,#63014,#63015,#63016,#63017,
#63018,#63019,#63020,#63021,#63022,#63023,#63024,#63025,#63026,#63027,#63028,
#63029,#63030,#63031,#63032,#63033,#63034,#63035,#63036,#63037,#63038,#63039,
#63040,#63041,#63042,#63043,#63044,#63045,#63046,#63047,#63048,#63049,#63050,
#63051,#63052,#63053,#63054,#63055,#63056,#63057,#63058,#63059,#63060,#63061,
#63062,#63063,#63064,#63065,#63066,#63067,#63068,#63069,#63070,#63071,#63072,
#63073,#63074,#63075,#63076,#63077,#63078,#63079,#63080,#63081,#63082,#63083,
#63084,#63085,#63086,#63087,#63088,#63089,#63090,#63091,#63092,#63093,#63094,
#63095,#63096,#63097,#63098,#63099,#63100,#63101,#63102,#63103,#63104,#63105,
#63106,#63107,#63108,#63109,#63110,#63111,#63112,#63113,#63114,#63115,#63116,
#63117,#63118,#63119,#63120,#63121,#63122,#63123,#63124,#63125,#63126,#63127,
#63128,#63129,#63130,#63131,#63132,#63133,#63134,#63135,#63136,#63137,#63138,
#63139,#63140,#63141,#63142,#63143,#63144,#63145,#63146,#63147,#63148,#63149,
#63150,#63151,#63152,#63153,#63154,#63155,#63156,#63157,#63158,#63159,#63160,
#63161,#63162,#63163,#63164,#63165,#63166,#63167,#63168,#63169,#63170,#63171,
#63172,#63173,#63174,#63175,#63176,#63177,#63178,#63179,#63180,#63181,#63182,
#63183,#63184,#63185,#63186,#63187,#63188,#63189,#63190,#63191,#63192,#63193,
#63194,#63195,#63196,#63197,#63198,#63199,#63200,#63201,#63202,#63203,#63204,
#63205,#63206,#63207,#63208,#63209,#63210,#63211,#63212,#63213,#63214,#63215,
#63216,#63217,#63218,#63219,#63220,#63221,#63222,#63223,#63224,#63225,#63226,
#63227,#63228,#63229,#63230,#63231,#63232,#63233,#63234,#63235,#63236,#63237,
#63238,#63239,#63240,#63241,#63242,#63243,#63244,#63245,#63246,#63247,#63248,
#63249,#63250,#63251,#63252,#63253,#63254,#63255,#63256,#63257,#63258,#63259,
#63260,#63261,#63262,#63263,#63264,#63265),.UNSPECIFIED.,.F.,.F.,(4,2,2,
2,2,2,2,2,2,2,2,2,2,2,2,2,2,2,2,2,2,2,2,2,2,2,2,2,2,2,2,2,2,2,2,2,2,2,2,
2,2,2,2,2,2,2,2,2,2,2,2,2,2,2,2,2,2,2,2,2,2,2,2,2,2,2,2,2,2,2,2,2,2,2,2,
2,2,2,2,2,2,2,2,2,2,2,2,2,2,2,2,2,2,2,2,2,2,2,2,2,2,2,2,2,2,2,2,2,2,2,2,
2,2,2,2,2,2,2,2,2,2,2,2,2,2,2,2,2,2,2,2,2,2,2,2,2,2,2,2,2,2,2,2,2,2,2,2,
2,2,2,2,2,2,2,2,2,2,2,2,2,2,2,2,2,2,2,2,2,2,2,2,2,2,2,2,2,2,2,2,2,2,2,2,
2,2,2,2,2,2,2,2,2,2,2,2,2,2,2,2,2,2,2,2,2,2,2,2,2,2,2,2,2,2,2,2,2,2,2,2,
2,2,2,2,2,2,2,2,2,2,2,2,2,2,2,2,2,2,2,2,2,2,2,2,2,2,2,2,2,2,2,2,2,2,2,2,
2,2,2,2,2,2,2,2,2,2,2,2,2,2,2,2,2,2,2,2,2,2,2,2,2,2,2,2,2,2,4),(0.000947724590819553,
0.207127724815813,0.237603480675008,0.242880588191167,0.24454806825737,
0.245605280156748,0.246596370893857,0.247897236940394,0.250092317633511,
0.263394818606918,0.496507780731943,0.539185768320658,0.599368239939017,
0.634092615263434,0.637474689143311,0.639664733503269,0.641378320251603,
0.642982115041705,0.644665732403467,0.647009945005304,0.653095635135978,
0.734265729789568,0.773633675436147,0.819428004846183,0.856468935458509,
0.929244616464085,0.999233698146093,1.03022547919743,1.03557229837192,1.03726426378135,
1.03835197678722,1.03937509229096,1.04071833863366,1.04369056265577,1.0674666751502,
1.27624187269221,1.34623592121595,1.40374887419738,1.43034062201941,1.4346437913907,
1.43647496164993,1.4383384309352,1.44007228993145,1.4424446574652,1.44838257809628,
1.51476299402155,1.55646798687329,1.65235350094941,1.81737909797484,1.8238598955143,
1.82572896985573,1.8268733157138,1.827913039325,1.82924217797162,1.8314109894856,
1.84292941111115,2.03102121289364,2.12302884815369,2.1817880146853,2.20868202223375,
2.21299716790313,2.21482971293008,2.21669376305457,2.21842644585236,2.22079454252517,
2.2254751322135,2.26345451814496,2.27094355871683,2.28894276717766,2.31901202130812,
2.44949235498463,2.60306616486844,2.61198456835532,2.61404002566128,2.61520983217603,
2.61611504403584,2.61729391293099,2.61935073984407,2.62766473763541,2.62928427099797,
2.78180023384879,2.87161662808824,2.95461954995335,2.99833013804605,3.0066737908653,
3.00953933817333,3.0114346507468,3.0132248437297,3.01558617153086,3.02085848856206,
3.06473938636343,3.06689176072869,3.06916191466725,3.07195523109899,3.08300676476133,
3.11198134261111,3.30343586960334,3.37146407445748,3.40019193855557,3.4052826712274,
3.40693402441988,3.40799128650385,3.40898106329199,3.41028747428738,3.41311212533903,
3.43598862706669,3.58713352953827,3.72251472077341,3.75227710124463,3.79320537088694,
3.81399809294732,3.81814728721038,3.82034046925134,3.82211611135656,3.82388468192189,
3.82707588579124,3.83687548282645,3.97970191705428,4.04970671255117,4.20587742081602,
4.21364676360052,4.21595483122959,4.21738362840693,4.21868757051583,4.2203720321278,
4.2238779960294,4.24695270637007,4.44631528050854,4.50564934072617,4.5683005823847,
4.58560334600116,4.59065052253146,4.59375915044009,4.59657948134747,4.60016936102526,
4.60584209023865,4.63403131682417,4.83859635114614,4.90122413516529,4.95862180999879,
4.96714953793225,4.96953656223199,4.9709830153505,4.97228283698306,4.97393408972684,
4.97727355566071,5.00650734117506,5.05894188475831,5.23631852131014,5.30267282766002,
5.35800922620107,5.36354529296927,5.36580632297705,5.3674766998798,5.36928914001459,
5.37175703927016,5.37740899425566,5.45757053311368,5.56165006970578,5.69696259849524,
5.72505125436997,5.73199767945725,5.74020723493719,5.74476234725454,5.74609425635309,
5.77544634877715,5.77820838015913,5.77953238662084,5.78046893703126,5.78135663674325,
5.78259923590203,5.78510667275141,5.80537919524097,5.83797031438553,5.89430820420481,
6.0440600310955,6.10294065133863,6.16708229607079,6.1728082112456,6.17509146660627,
6.17675860445949,6.17854883283052,6.18095368266124,6.18632300231797,6.30901879048983,
6.44281263648507,6.56181357330139,6.56939936258579,6.57138800788964,6.5725513919714,
6.57355783712935,6.57478616210781,6.57711182033334,6.59060677539225,6.61745918219728,
6.67180106212564,6.81263421994436,6.9564195293122,6.9664508242804,6.96973273109896,
6.97155506533697,6.97336957680026,6.9756275973213,6.97997429000239,7.00732987835108,
7.06765779865156,7.21628891010548,7.34902065517395,7.35744415785545,7.35957373785265,
7.3607889421538,7.36171617998268,7.36291956779403,7.36505431775467,7.37462947939665,
7.53411564240847,7.61622079936947,7.68534691114172,7.7404325119529,7.7456231821168,
7.74811823503617,7.74988443080237,7.75154603463036,7.75384529441409,7.75839047130692,
7.79121409287726,7.88837602215563,7.98157722973941,8.11129590771979,8.11637557863732,
8.12021939221516,8.14426574416599,8.14720831103851,8.14844488823968,8.14947498136198,
8.15053045560553,8.15207130223126,8.15625492477782,8.25410494204454,8.35429125495423,
8.52727441100835,8.53935536900768,8.54276233626839,8.5447848800462,8.54654452689706,
8.54870490193997,8.55283506466141,8.57796827436248,8.63136356925425,8.65162069698498,
8.66698800859803,8.759453349192,8.926934974668,8.9377322885196,8.93977895374562,
8.94104898698024,8.94203161175717,8.94311207996608,8.94488680188714,8.95114340844106,
8.99120102300993,9.07084470575175,9.1028393295956,9.13798902689615,9.27685845217146,
9.344676829327,9.35052880258044,9.35284428392076,9.3545286206513,9.35633135059043,
9.35874263609865,9.36408382080603,9.46995219416744,9.53371155654059,9.56286865554598,
9.5903721922408,9.73669576998189,9.74629825936004,9.74888018862983,9.75038544466215,
9.7516658036195,9.75322652959894,9.75613253866614,9.75974179342287,9.76749543643411,
9.95163942614331),.UNSPECIFIED.);
#537=B_SPLINE_CURVE_WITH_KNOTS('',3,(#63267,#63268,#63269,#63270,#63271,
#63272,#63273,#63274,#63275,#63276,#63277,#63278,#63279,#63280,#63281,#63282,
#63283,#63284),.UNSPECIFIED.,.F.,.F.,(4,2,2,2,2,2,2,2,4),(-167.4557484068,
-166.620831494905,-165.78591458301,-164.950997671115,-164.11608075922,-163.281163847326,
-162.446246935431,-161.611330023536,-161.17256309962),.UNSPECIFIED.);
#538=B_SPLINE_CURVE_WITH_KNOTS('',3,(#63286,#63287,#63288,#63289,#63290,
#63291,#63292,#63293,#63294,#63295,#63296,#63297,#63298,#63299,#63300,#63301,
#63302,#63303,#63304,#63305,#63306,#63307,#63308,#63309,#63310,#63311,#63312,
#63313,#63314,#63315,#63316,#63317,#63318,#63319,#63320,#63321,#63322,#63323,
#63324,#63325,#63326,#63327,#63328,#63329,#63330,#63331,#63332,#63333,#63334,
#63335,#63336,#63337,#63338,#63339,#63340,#63341,#63342,#63343,#63344,#63345,
#63346,#63347,#63348,#63349,#63350,#63351,#63352,#63353,#63354,#63355,#63356,
#63357,#63358,#63359,#63360,#63361,#63362,#63363,#63364,#63365,#63366,#63367,
#63368,#63369,#63370,#63371,#63372,#63373,#63374,#63375,#63376,#63377,#63378,
#63379,#63380,#63381,#63382,#63383,#63384,#63385,#63386,#63387,#63388,#63389,
#63390,#63391,#63392,#63393,#63394,#63395,#63396,#63397,#63398,#63399,#63400,
#63401,#63402,#63403,#63404,#63405,#63406,#63407,#63408,#63409,#63410,#63411,
#63412,#63413,#63414,#63415,#63416,#63417,#63418,#63419,#63420,#63421,#63422,
#63423,#63424,#63425,#63426,#63427,#63428,#63429,#63430,#63431,#63432,#63433,
#63434,#63435,#63436,#63437,#63438,#63439,#63440,#63441,#63442,#63443,#63444,
#63445,#63446,#63447,#63448,#63449,#63450,#63451,#63452,#63453,#63454,#63455,
#63456,#63457,#63458,#63459,#63460,#63461,#63462,#63463,#63464,#63465,#63466,
#63467,#63468,#63469,#63470,#63471,#63472,#63473,#63474,#63475,#63476,#63477,
#63478,#63479,#63480,#63481,#63482,#63483,#63484,#63485,#63486,#63487,#63488,
#63489,#63490,#63491,#63492,#63493,#63494,#63495,#63496,#63497,#63498,#63499,
#63500,#63501,#63502,#63503,#63504,#63505,#63506,#63507,#63508,#63509,#63510,
#63511,#63512,#63513,#63514,#63515,#63516,#63517,#63518,#63519,#63520,#63521,
#63522,#63523,#63524,#63525,#63526,#63527,#63528,#63529,#63530,#63531,#63532,
#63533,#63534,#63535,#63536,#63537,#63538,#63539,#63540,#63541,#63542,#63543,
#63544,#63545,#63546,#63547,#63548,#63549,#63550),.UNSPECIFIED.,.F.,.F.,
(4,3,3,3,3,3,3,3,3,3,3,3,3,3,3,3,3,3,3,3,3,3,3,3,3,3,3,3,3,3,3,3,3,3,3,
3,3,3,3,3,3,3,3,3,3,3,3,3,3,3,3,3,3,3,3,3,3,3,3,3,3,3,3,3,3,3,3,3,3,3,3,
3,3,3,3,3,3,3,3,3,3,3,3,3,3,3,3,3,4),(-161.17256309962,-161.093277609603,
-161.013852914826,-160.93421691605,-160.85446750119,-160.774546868961,-160.743689296198,
-160.665323622154,-160.587054452714,-160.508876506316,-160.430815734123,
-160.352826671867,-160.27492681887,-160.244485292172,-160.166574704059,
-160.088594307158,-160.010538977298,-159.932354261544,-159.854098881938,
-159.775724191303,-159.745281288147,-159.67072219162,-159.596238542007,
-159.521816478903,-159.447442182465,-159.373101864674,-159.298781760927,
-159.224452891769,-159.150114658578,-159.075754600227,-159.001360246425,
-158.926879892853,-158.852350139852,-158.777718409009,-158.746873280096,
-158.672953493819,-158.599120518462,-158.525359892834,-158.451657209306,
-158.377998102671,-158.304368239841,-158.230741164164,-158.157111935124,
-158.083467597361,-158.009795188901,-157.936042861464,-157.862245710629,
-157.78834768398,-157.748465272045,-157.673904210517,-157.599423982859,
-157.525010675825,-157.450650420387,-157.376329382756,-157.302033755808,
-157.227737020108,-157.153435690567,-157.079117277243,-157.004769283516,
-156.930342167363,-156.85586966057,-156.78130083511,-156.750057263994,-156.67549627786,
-156.601016113474,-156.526602857631,-156.452242641338,-156.377921630834,
-156.303626019013,-156.229329280504,-156.155027936969,-156.080709498459,
-156.006361468348,-155.931934299084,-155.857461729539,-155.782892827079,
-155.751649255943,-155.678823428956,-155.606079482122,-155.533402341825,
-155.460777006045,-155.388185732948,-155.315611970161,-155.243042231707,
-155.170463035149,-155.097826176621,-155.025159832957,-154.952403540713,
-154.890004205893),.UNSPECIFIED.);
#539=B_SPLINE_CURVE_WITH_KNOTS('',3,(#63552,#63553,#63554,#63555,#63556,
#63557,#63558,#63559,#63560,#63561,#63562,#63563,#63564,#63565,#63566,#63567,
#63568,#63569,#63570,#63571,#63572,#63573,#63574,#63575,#63576,#63577,#63578,
#63579,#63580,#63581,#63582,#63583,#63584,#63585,#63586,#63587,#63588,#63589,
#63590,#63591,#63592,#63593,#63594,#63595,#63596,#63597,#63598,#63599,#63600,
#63601,#63602,#63603,#63604,#63605,#63606,#63607,#63608,#63609,#63610,#63611,
#63612,#63613,#63614,#63615,#63616,#63617,#63618,#63619,#63620,#63621,#63622,
#63623,#63624,#63625,#63626,#63627,#63628,#63629,#63630,#63631,#63632,#63633,
#63634,#63635,#63636,#63637,#63638,#63639,#63640,#63641,#63642,#63643,#63644,
#63645,#63646,#63647,#63648,#63649,#63650,#63651,#63652,#63653,#63654,#63655,
#63656,#63657,#63658,#63659,#63660,#63661,#63662,#63663,#63664,#63665,#63666,
#63667,#63668,#63669,#63670,#63671,#63672,#63673,#63674,#63675,#63676,#63677,
#63678,#63679,#63680,#63681,#63682,#63683,#63684,#63685,#63686,#63687,#63688,
#63689,#63690,#63691,#63692,#63693,#63694,#63695,#63696,#63697,#63698,#63699,
#63700,#63701,#63702,#63703,#63704,#63705,#63706,#63707,#63708,#63709,#63710,
#63711,#63712,#63713,#63714,#63715,#63716,#63717,#63718,#63719,#63720,#63721,
#63722,#63723,#63724,#63725,#63726,#63727,#63728,#63729,#63730,#63731,#63732,
#63733,#63734,#63735,#63736,#63737,#63738,#63739,#63740,#63741,#63742,#63743,
#63744,#63745,#63746,#63747,#63748,#63749,#63750,#63751,#63752,#63753,#63754,
#63755,#63756,#63757,#63758,#63759,#63760,#63761,#63762,#63763,#63764,#63765,
#63766,#63767,#63768,#63769,#63770,#63771,#63772,#63773,#63774,#63775,#63776,
#63777,#63778,#63779,#63780,#63781,#63782,#63783,#63784,#63785,#63786,#63787,
#63788,#63789,#63790,#63791,#63792,#63793,#63794,#63795,#63796,#63797,#63798,
#63799,#63800,#63801,#63802,#63803,#63804,#63805,#63806,#63807,#63808,#63809,
#63810,#63811,#63812,#63813,#63814,#63815,#63816,#63817,#63818,#63819,#63820,
#63821,#63822,#63823,#63824,#63825,#63826,#63827,#63828,#63829,#63830,#63831,
#63832,#63833,#63834,#63835,#63836,#63837,#63838,#63839,#63840,#63841,#63842,
#63843,#63844,#63845,#63846,#63847,#63848,#63849,#63850,#63851,#63852,#63853,
#63854,#63855,#63856,#63857,#63858,#63859,#63860,#63861,#63862,#63863,#63864,
#63865,#63866,#63867,#63868,#63869,#63870,#63871,#63872,#63873,#63874,#63875,
#63876,#63877,#63878,#63879,#63880,#63881,#63882,#63883,#63884,#63885,#63886,
#63887,#63888,#63889,#63890,#63891,#63892,#63893,#63894,#63895,#63896,#63897,
#63898,#63899,#63900,#63901,#63902,#63903,#63904,#63905,#63906,#63907,#63908,
#63909,#63910,#63911,#63912,#63913,#63914,#63915,#63916,#63917,#63918,#63919,
#63920,#63921,#63922,#63923,#63924,#63925,#63926,#63927,#63928,#63929,#63930,
#63931,#63932,#63933,#63934,#63935,#63936,#63937,#63938,#63939,#63940,#63941,
#63942,#63943,#63944,#63945,#63946,#63947,#63948,#63949,#63950,#63951,#63952,
#63953,#63954,#63955,#63956,#63957,#63958,#63959,#63960,#63961,#63962,#63963,
#63964,#63965,#63966,#63967,#63968,#63969,#63970,#63971,#63972,#63973,#63974,
#63975,#63976,#63977,#63978,#63979,#63980,#63981,#63982,#63983,#63984,#63985,
#63986,#63987,#63988,#63989,#63990,#63991,#63992,#63993,#63994,#63995,#63996,
#63997,#63998,#63999,#64000,#64001,#64002,#64003,#64004,#64005,#64006,#64007,
#64008,#64009,#64010,#64011,#64012,#64013,#64014,#64015,#64016,#64017,#64018,
#64019,#64020,#64021,#64022,#64023,#64024,#64025,#64026,#64027,#64028,#64029,
#64030,#64031,#64032,#64033,#64034,#64035,#64036,#64037,#64038,#64039,#64040,
#64041,#64042,#64043,#64044,#64045,#64046,#64047,#64048,#64049,#64050,#64051,
#64052,#64053,#64054,#64055,#64056,#64057,#64058,#64059,#64060,#64061,#64062,
#64063,#64064,#64065,#64066,#64067,#64068,#64069,#64070,#64071,#64072,#64073,
#64074,#64075,#64076,#64077,#64078,#64079,#64080,#64081,#64082,#64083,#64084,
#64085,#64086,#64087,#64088,#64089,#64090,#64091,#64092,#64093,#64094,#64095,
#64096,#64097,#64098,#64099,#64100,#64101,#64102,#64103,#64104,#64105,#64106,
#64107,#64108,#64109,#64110,#64111,#64112,#64113,#64114,#64115),
 .UNSPECIFIED.,.F.,.F.,(4,2,2,2,2,2,2,2,2,2,2,2,2,2,2,2,2,2,2,2,2,2,2,2,
2,2,2,2,2,2,2,2,2,2,2,2,2,2,2,2,2,2,2,2,2,2,2,2,2,2,2,2,2,2,2,2,2,2,2,2,
2,2,2,2,2,2,2,2,2,2,2,2,2,2,2,2,2,2,2,2,2,2,2,2,2,2,2,2,2,2,2,2,2,2,2,2,
2,2,2,2,2,2,2,2,2,2,2,2,2,2,2,2,2,2,2,2,2,2,2,2,2,2,2,2,2,2,2,2,2,2,2,2,
2,2,2,2,2,2,2,2,2,2,2,2,2,2,2,2,2,2,2,2,2,2,2,2,2,2,2,2,2,2,2,2,2,2,2,2,
2,2,2,2,2,2,2,2,2,2,2,2,2,2,2,2,2,2,2,2,2,2,2,2,2,2,2,2,2,2,2,2,2,2,2,2,
2,2,2,2,2,2,2,2,2,2,2,2,2,2,2,2,2,2,2,2,2,2,2,2,2,2,2,2,2,2,2,2,2,2,2,2,
2,2,2,2,2,2,2,2,2,2,2,2,2,2,2,2,2,2,2,2,2,2,2,2,2,2,2,2,2,2,2,2,2,2,2,2,
2,2,2,2,2,4),(0.00136600686276613,0.0861468345095725,0.103286173672408,
0.105373964908813,0.106676925466201,0.107657746315892,0.10865265629107,
0.109575320646033,0.110845213942466,0.114060655613495,0.151757518273064,
0.156809171672282,0.163055226769575,0.209266853378583,0.216547421283818,
0.432110891827582,0.512367810499585,0.517965862907182,0.520424619489773,
0.522235952003031,0.523909266231999,0.526180307013929,0.531770917615309,
0.589125755379268,0.697272092775012,0.82379549412045,0.864509470399254,
0.887701450714803,0.903999804991615,0.913749035427492,0.91625083056306,
0.917488942525277,0.918776243759128,0.920266188472274,0.922781350083865,
0.931760480025448,0.950370262315602,0.977948905461798,1.09450731135067,
1.10865866835453,1.12530295012558,1.14542820669018,1.17093726968923,1.2067966486548,
1.268978719982,1.28607505907945,1.29110145481201,1.29420613596962,1.29702861093301,
1.300629237588,1.30772314675413,1.34982398311746,1.53276313042715,1.61743233918193,
1.65068686328156,1.66122248493384,1.66574779953149,1.66818418622269,1.67027716421508,
1.6716453578029,1.67296107897272,1.67469173577668,1.67853615939151,1.71539429179514,
1.87224544842473,1.88058948601965,1.88963349541841,1.9113939115549,1.94260291976575,
2.00028853939063,2.05344262619743,2.06295045486912,2.06598427246075,2.0679144650741,
2.06971209646244,2.07204673543636,2.07593065931185,2.08456506657105,2.23864592516649,
2.32393838946969,2.40584696597568,2.47014098353738,2.47804323091178,2.47996444983278,
2.48089876871747,2.48178029957768,2.4827367827063,2.48441175993337,2.48921637258699,
2.56439651998784,2.74276847862193,2.83798814175757,2.87030720078494,2.87470299444743,
2.87691920665452,2.87851777973851,2.8802141521766,2.88308957390748,2.89077852321149,
3.00413339824161,3.07121444470293,3.16757410578299,3.2664649406515,3.26966174368101,
3.27210303007129,3.27336282293146,3.27428072352468,3.27524370852951,3.27658366359109,
3.2793068765687,3.30459764013293,3.34171191024698,3.56054341550202,3.65391684390414,
3.6673888278488,3.67089919276305,3.67297548701912,3.67480965277939,3.67709773266258,
3.68062587118442,3.69656613203174,3.94930892915765,4.03379691011564,4.05837980696131,
4.0611045654401,4.0624323682412,4.06337269692271,4.0643627973657,4.06575277651548,
4.06941810537744,4.12253580750349,4.35079256456728,4.4160289390183,4.44478297554158,
4.44918576238912,4.45145585467486,4.45327174637383,4.45535456201974,4.45889405834353,
4.46829170226635,4.61060278415822,4.76385048314198,4.81110072473817,4.84329713795082,
4.84882505055077,4.85056282480903,4.85166170424352,4.85268035020252,4.85399642861372,
4.85687798331519,4.87969858920732,4.9782208780694,5.2253300020657,5.24147362636173,
5.24492979600868,5.24714924526974,5.24891404704051,5.25089656967671,5.25421199118372,
5.26652271472088,5.347607468908,5.40227272981092,5.61630040225658,5.6398141836146,
5.64242164436536,5.64371186013077,5.64464245064138,5.64553268844385,5.64680013967281,
5.649456495844,5.67736949713039,5.73311576741655,5.77719678197101,6.03416471666612,
6.03749772886747,6.05181438378162,6.05513986073624,6.05732793140271,6.05910290403764,
6.0611350882833,6.06462731658767,6.07872639889206,6.25263287093517,6.43756495177981,
6.44972603413614,6.45229119825805,6.45393125526195,6.45522988086817,6.45668295962764,
6.459099442793,6.46792626434181,6.52881805723823,6.607811574523,6.77817220742128,
6.81898443050167,6.82595628968731,6.82920689186231,6.83200340772601,6.83500520561845,
6.83956938870991,6.85279883187459,7.04839531567641,7.15554940331971,7.20119473475273,
7.20532738852862,7.20699329486049,7.20821603078815,7.2095351301934,7.21131821437206,
7.21534582194712,7.2831612644692,7.36460895089989,7.55297555133023,7.59571865231594,
7.60045529364844,7.60280104683527,7.60449361501895,7.60620028825252,7.60848436925048,
7.6132110686816,7.61934024256664,7.63338613307489,7.6748716473014,7.77036760075454,
8.00020123064167,8.01392019750202,8.01634178781049,8.01757885037082,8.01855673477646,
8.01965861477876,8.02150931633003,8.02846286996565,8.07631794101876,8.15053235444009,
8.24299298516318,8.29952484148184,8.40341962736315,8.41003791124797,8.41246743126957,
8.41417406971254,8.41591089235737,8.41812808918061,8.42054789967341,8.42447576776836,
8.43221557099516,8.45146875308431,8.48481393795657,8.54030331559143,8.66540516577765,
8.79846844145902,8.80693154051052,8.80881956019495,8.81005731332172,8.81096378510183,
8.8120866951413,8.81393167806943,8.82043554155496,8.86226390722535,8.90536531506369,
9.01765357074381,9.0790168544491,9.19688483061321,9.20480501830483,9.20778382824276,
9.20954605287822,9.21135780171077,9.21369986517822,9.2162665220373,9.22047080346694,
9.22884233802831,9.24995825136854,9.34904089158242,9.58222851194488,9.59500949045565,
9.59725584660048,9.59860821774252,9.59965147456159,9.60078465069335,9.60260328298588,
9.60861575143648,9.64504819585966,9.9560577309929),.UNSPECIFIED.);
#540=B_SPLINE_CURVE_WITH_KNOTS('',3,(#64117,#64118,#64119,#64120,#64121,
#64122,#64123,#64124,#64125,#64126,#64127),.UNSPECIFIED.,.F.,.F.,(4,1,1,
1,1,1,1,1,4),(-142.322804428922,-141.77393714323,-140.775529135179,-139.777121127128,
-139.277917123103,-138.778713119077,-137.780305111027,-136.781897102976,
-136.039821870902),.UNSPECIFIED.);
#541=B_SPLINE_CURVE_WITH_KNOTS('',3,(#64129,#64130,#64131,#64132,#64133,
#64134,#64135,#64136,#64137,#64138,#64139,#64140,#64141,#64142,#64143,#64144,
#64145,#64146,#64147,#64148,#64149,#64150,#64151,#64152,#64153,#64154,#64155,
#64156,#64157,#64158,#64159,#64160,#64161,#64162,#64163,#64164,#64165,#64166,
#64167,#64168,#64169,#64170,#64171,#64172,#64173,#64174,#64175,#64176,#64177,
#64178,#64179,#64180,#64181,#64182,#64183,#64184,#64185,#64186,#64187,#64188,
#64189,#64190,#64191,#64192,#64193,#64194,#64195,#64196,#64197,#64198,#64199,
#64200,#64201,#64202,#64203,#64204,#64205,#64206,#64207,#64208,#64209,#64210,
#64211,#64212,#64213,#64214,#64215,#64216,#64217,#64218,#64219,#64220,#64221,
#64222,#64223,#64224,#64225,#64226,#64227,#64228,#64229,#64230,#64231,#64232,
#64233,#64234,#64235,#64236,#64237,#64238,#64239,#64240,#64241,#64242,#64243,
#64244,#64245,#64246,#64247,#64248,#64249,#64250,#64251,#64252,#64253,#64254,
#64255,#64256,#64257,#64258,#64259,#64260,#64261,#64262,#64263,#64264,#64265,
#64266,#64267,#64268,#64269,#64270,#64271,#64272,#64273,#64274,#64275,#64276,
#64277,#64278,#64279,#64280,#64281,#64282,#64283,#64284,#64285,#64286,#64287,
#64288,#64289,#64290,#64291,#64292,#64293,#64294,#64295,#64296,#64297,#64298,
#64299,#64300,#64301,#64302,#64303,#64304,#64305,#64306,#64307,#64308,#64309,
#64310,#64311,#64312,#64313,#64314,#64315,#64316,#64317,#64318,#64319,#64320,
#64321,#64322,#64323,#64324,#64325,#64326,#64327,#64328,#64329,#64330,#64331,
#64332,#64333,#64334,#64335,#64336,#64337,#64338,#64339,#64340,#64341,#64342,
#64343,#64344,#64345,#64346,#64347,#64348,#64349,#64350,#64351,#64352,#64353,
#64354,#64355,#64356,#64357,#64358,#64359,#64360,#64361,#64362,#64363,#64364,
#64365,#64366,#64367,#64368,#64369,#64370,#64371,#64372,#64373,#64374,#64375,
#64376,#64377,#64378,#64379,#64380,#64381,#64382,#64383,#64384,#64385,#64386,
#64387,#64388,#64389,#64390,#64391,#64392,#64393),.UNSPECIFIED.,.F.,.F.,
(4,3,3,3,3,3,3,3,3,3,3,3,3,3,3,3,3,3,3,3,3,3,3,3,3,3,3,3,3,3,3,3,3,3,3,
3,3,3,3,3,3,3,3,3,3,3,3,3,3,3,3,3,3,3,3,3,3,3,3,3,3,3,3,3,3,3,3,3,3,3,3,
3,3,3,3,3,3,3,3,3,3,3,3,3,3,3,3,3,4),(-136.039821779079,-135.94619225248,
-135.850900439115,-135.783489094925,-135.70892810879,-135.634447944404,
-135.560034688561,-135.485674472268,-135.411353461763,-135.337057849942,
-135.262761111433,-135.188459767897,-135.114141329388,-135.039793299276,
-134.965366130011,-134.890893560466,-134.816324658006,-134.785081086874,
-134.71118760562,-134.637376739478,-134.563634044055,-134.48994512516,-134.416295627933,
-134.342671226749,-134.269043379823,-134.195409513755,-134.12175667154,
-134.048071887332,-133.974301334434,-133.900482623819,-133.826557972951,
-133.786673078823,-133.712050013409,-133.637512684528,-133.563047195775,
-133.488639698134,-133.414276380892,-133.339943462991,-133.265617000396,
-133.191290668441,-133.116952009644,-133.042588562366,-132.968153305183,
-132.893676831792,-132.819110459651,-132.788265070772,-132.709899396731,
-132.631630227293,-132.553452280897,-132.475391508706,-132.397402446453,
-132.319502593457,-132.289061066747,-132.211150478633,-132.133170081729,
-132.055114751869,-131.976930036113,-131.898674656506,-131.820299965869,
-131.789857062721,-131.715297966194,-131.640814316582,-131.566392253477,
-131.49201795704,-131.417677639249,-131.343357535502,-131.269028666344,
-131.194690433153,-131.120330374802,-131.045936021,-130.971455667428,-130.896925914427,
-130.822294183585,-130.79144905467,-130.717529268393,-130.643696293037,
-130.569935667409,-130.496232983881,-130.422573877246,-130.348944014416,
-130.275316938739,-130.2016877097,-130.128043371937,-130.054370963477,-129.98061863604,
-129.906821485206,-129.832923458557,-129.793041046619,-129.756636563722),
 .UNSPECIFIED.);
#542=B_SPLINE_CURVE_WITH_KNOTS('',3,(#64395,#64396,#64397,#64398,#64399,
#64400,#64401,#64402,#64403,#64404,#64405),.UNSPECIFIED.,.F.,.F.,(4,1,1,
1,1,1,1,1,4),(-129.75663160721,-128.794633038568,-127.796225030517,-126.797817022466,
-125.799409014416,-125.30020501039,-124.801001006365,-123.802592998314,
-123.473451256543),.UNSPECIFIED.);
#543=B_SPLINE_CURVE_WITH_KNOTS('',3,(#64407,#64408,#64409,#64410,#64411,
#64412,#64413,#64414,#64415,#64416,#64417,#64418,#64419,#64420,#64421,#64422,
#64423,#64424),.UNSPECIFIED.,.F.,.F.,(4,2,2,2,2,2,2,2,4),(-123.473451256543,
-122.638534344648,-121.803617432753,-120.968700520858,-120.133783608963,
-119.298866697069,-118.463949785174,-117.629032873279,-117.190265949363),
 .UNSPECIFIED.);
#544=B_SPLINE_CURVE_WITH_KNOTS('',3,(#64426,#64427,#64428,#64429,#64430,
#64431,#64432,#64433,#64434,#64435,#64436,#64437,#64438,#64439,#64440,#64441,
#64442,#64443,#64444,#64445,#64446,#64447,#64448,#64449,#64450,#64451,#64452,
#64453,#64454,#64455,#64456,#64457,#64458,#64459,#64460,#64461,#64462,#64463,
#64464,#64465,#64466,#64467,#64468,#64469,#64470,#64471,#64472,#64473,#64474,
#64475,#64476,#64477,#64478,#64479,#64480,#64481,#64482,#64483,#64484,#64485,
#64486,#64487,#64488,#64489,#64490,#64491,#64492,#64493,#64494,#64495,#64496,
#64497,#64498,#64499,#64500,#64501,#64502,#64503,#64504,#64505,#64506,#64507,
#64508,#64509,#64510,#64511,#64512,#64513,#64514,#64515,#64516,#64517,#64518,
#64519,#64520,#64521,#64522,#64523,#64524,#64525,#64526,#64527,#64528,#64529,
#64530,#64531,#64532,#64533,#64534,#64535,#64536,#64537,#64538,#64539,#64540,
#64541,#64542,#64543,#64544,#64545,#64546,#64547,#64548,#64549,#64550,#64551,
#64552,#64553,#64554,#64555,#64556,#64557,#64558,#64559,#64560,#64561,#64562,
#64563,#64564,#64565,#64566,#64567,#64568,#64569,#64570,#64571,#64572,#64573,
#64574,#64575,#64576,#64577,#64578,#64579,#64580,#64581,#64582,#64583,#64584,
#64585,#64586,#64587,#64588,#64589,#64590,#64591,#64592,#64593,#64594,#64595,
#64596,#64597,#64598,#64599,#64600,#64601,#64602,#64603,#64604,#64605,#64606,
#64607,#64608,#64609,#64610,#64611,#64612,#64613,#64614,#64615,#64616,#64617,
#64618,#64619,#64620,#64621,#64622,#64623,#64624,#64625,#64626,#64627,#64628,
#64629,#64630,#64631,#64632,#64633,#64634,#64635,#64636,#64637,#64638,#64639,
#64640,#64641,#64642,#64643,#64644,#64645,#64646,#64647,#64648,#64649,#64650,
#64651,#64652,#64653,#64654,#64655,#64656,#64657,#64658,#64659,#64660,#64661,
#64662,#64663,#64664,#64665,#64666,#64667,#64668,#64669,#64670,#64671,#64672,
#64673,#64674,#64675,#64676,#64677,#64678,#64679,#64680,#64681,#64682,#64683,
#64684,#64685,#64686,#64687,#64688,#64689,#64690),.UNSPECIFIED.,.F.,.F.,
(4,3,3,3,3,3,3,3,3,3,3,3,3,3,3,3,3,3,3,3,3,3,3,3,3,3,3,3,3,3,3,3,3,3,3,
3,3,3,3,3,3,3,3,3,3,3,3,3,3,3,3,3,3,3,3,3,3,3,3,3,3,3,3,3,3,3,3,3,3,3,3,
3,3,3,3,3,3,3,3,3,3,3,3,3,3,3,3,3,4),(-117.190265949363,-117.105316619372,
-117.019674410368,-116.933688950344,-116.84729407057,-116.813736941957,
-116.73981715568,-116.665984180324,-116.592223554695,-116.518520871167,
-116.444861764532,-116.371231901702,-116.297604826025,-116.223975596986,
-116.150331259222,-116.076658850763,-116.002906523325,-115.929109372491,
-115.855211345842,-115.815328933906,-115.740767872377,-115.66628764472,
-115.591874337686,-115.517514082247,-115.443193044616,-115.368897417668,
-115.294600681968,-115.220299352427,-115.145980939102,-115.071632945376,
-114.997205829222,-114.922733322429,-114.84816449697,-114.816920925855,
-114.742359939721,-114.667879775335,-114.593466519493,-114.5191063032,-114.444785292696,
-114.370489680875,-114.296192942367,-114.221891598831,-114.147573160322,
-114.073225130211,-113.998797960947,-113.924325391403,-113.849756488943,
-113.818512917805,-113.744619436551,-113.670808570409,-113.597065874986,
-113.523376956091,-113.449727458864,-113.37610305768,-113.302475210754,
-113.228841344686,-113.155188502471,-113.081503718263,-113.007733165365,
-112.93391445475,-112.859989803883,-112.820104909754,-112.74548184434,-112.670944515459,
-112.596479026706,-112.522071529065,-112.447708211822,-112.373375293921,
-112.299048831326,-112.224722499371,-112.150383840575,-112.076020393296,
-112.001585136114,-111.927108662723,-111.852542290581,-111.821696901703,
-111.743331227661,-111.665062058222,-111.586884111824,-111.508823339632,
-111.430834277378,-111.352934424382,-111.322492897677,-111.247393740118,
-111.172260130373,-111.097041135258,-111.021774372652,-110.946406268164,
-110.907282228194),.UNSPECIFIED.);
#545=B_SPLINE_CURVE_WITH_KNOTS('',3,(#64692,#64693,#64694,#64695,#64696,
#64697,#64698,#64699,#64700,#64701,#64702,#64703,#64704,#64705,#64706,#64707,
#64708,#64709),.UNSPECIFIED.,.F.,.F.,(4,2,2,2,2,2,2,2,4),(-110.907004517659,
-110.072163730289,-109.237246818394,-108.402329906499,-107.567412994604,
-106.732496082709,-105.897579170815,-105.06266225892,-104.623985027996),
 .UNSPECIFIED.);
#546=B_SPLINE_CURVE_WITH_KNOTS('',3,(#64711,#64712,#64713,#64714,#64715,
#64716,#64717,#64718,#64719,#64720,#64721,#64722,#64723,#64724,#64725,#64726,
#64727,#64728,#64729,#64730,#64731,#64732,#64733,#64734,#64735,#64736,#64737,
#64738,#64739,#64740,#64741,#64742,#64743,#64744,#64745,#64746,#64747,#64748,
#64749,#64750,#64751,#64752,#64753,#64754,#64755,#64756,#64757,#64758,#64759,
#64760,#64761,#64762,#64763,#64764,#64765,#64766,#64767,#64768,#64769,#64770,
#64771,#64772,#64773,#64774,#64775,#64776,#64777,#64778,#64779,#64780,#64781,
#64782,#64783,#64784,#64785,#64786,#64787,#64788,#64789,#64790,#64791,#64792,
#64793,#64794,#64795,#64796,#64797,#64798,#64799,#64800,#64801,#64802,#64803,
#64804,#64805,#64806,#64807,#64808,#64809,#64810,#64811,#64812,#64813,#64814,
#64815,#64816,#64817,#64818,#64819,#64820,#64821,#64822,#64823,#64824,#64825,
#64826,#64827,#64828,#64829,#64830,#64831,#64832,#64833,#64834,#64835,#64836,
#64837,#64838,#64839,#64840,#64841,#64842,#64843,#64844,#64845,#64846,#64847,
#64848,#64849,#64850,#64851,#64852,#64853,#64854,#64855,#64856,#64857,#64858,
#64859,#64860,#64861,#64862,#64863,#64864,#64865,#64866,#64867,#64868,#64869,
#64870,#64871,#64872,#64873,#64874,#64875,#64876,#64877,#64878,#64879,#64880,
#64881,#64882,#64883,#64884,#64885,#64886,#64887,#64888,#64889,#64890,#64891,
#64892,#64893,#64894,#64895,#64896,#64897,#64898,#64899,#64900,#64901,#64902,
#64903,#64904,#64905,#64906,#64907,#64908,#64909,#64910,#64911,#64912,#64913,
#64914,#64915,#64916,#64917,#64918,#64919,#64920,#64921,#64922,#64923,#64924,
#64925,#64926,#64927,#64928,#64929,#64930,#64931,#64932,#64933,#64934,#64935,
#64936,#64937,#64938,#64939,#64940,#64941,#64942,#64943,#64944,#64945,#64946,
#64947,#64948,#64949,#64950,#64951,#64952,#64953,#64954,#64955,#64956,#64957,
#64958,#64959,#64960,#64961,#64962,#64963,#64964,#64965,#64966,#64967,#64968,
#64969,#64970,#64971,#64972,#64973,#64974,#64975),.UNSPECIFIED.,.F.,.F.,
(4,3,3,3,3,3,3,3,3,3,3,3,3,3,3,3,3,3,3,3,3,3,3,3,3,3,3,3,3,3,3,3,3,3,3,
3,3,3,3,3,3,3,3,3,3,3,3,3,3,3,3,3,3,3,3,3,3,3,3,3,3,3,3,3,3,3,3,3,3,3,3,
3,3,3,3,3,3,3,3,3,3,3,3,3,3,3,3,3,4),(-104.623358907686,-104.550797753273,
-104.47828304321,-104.405799590655,-104.333636841321,-104.255726253206,
-104.177745856302,-104.09969052644,-104.021505810683,-103.943250431075,
-103.864875740437,-103.834432837295,-103.759873740768,-103.685390091156,
-103.610968028051,-103.536593731613,-103.462253413823,-103.387933310076,
-103.313604440918,-103.239266207727,-103.164906149377,-103.090511795574,
-103.016031442002,-102.941501689001,-102.866869958159,-102.836024829244,
-102.762105042967,-102.688272067611,-102.614511441983,-102.540808758455,
-102.467149651821,-102.393519788992,-102.319892713315,-102.246263484276,
-102.172619146513,-102.098946738052,-102.025194410616,-101.951397259782,
-101.877499233133,-101.837616821194,-101.763055759665,-101.688575532008,
-101.614162224974,-101.539801969536,-101.465480931905,-101.391185304956,
-101.316888569256,-101.242587239716,-101.168268826391,-101.093920832665,
-101.019493716511,-100.945021209718,-100.870452384259,-100.839208813143,
-100.764647827009,-100.690167662623,-100.61575440678,-100.541394190487,
-100.467073179983,-100.392777568161,-100.318480829653,-100.244179486117,
-100.169861047607,-100.095513017496,-100.021085848232,-99.9466132786866,
-99.8720443762267,-99.8408008050917,-99.7669073238381,-99.6930964576958,
-99.619353762273,-99.5456648433779,-99.4720153461518,-99.3983909449678,
-99.3247630980424,-99.2511292319739,-99.177476389759,-99.1037916055511,
-99.0300210526534,-98.9562023420383,-98.8822776911711,-98.8423927970408,
-98.7629300258068,-98.683602234694,-98.604407958319,-98.5254009471871,-98.4465090550021,
-98.3677746029374,-98.3407100278245),.UNSPECIFIED.);
#547=B_SPLINE_CURVE_WITH_KNOTS('',3,(#64977,#64978,#64979,#64980,#64981,
#64982,#64983,#64984,#64985,#64986,#64987,#64988,#64989,#64990,#64991,#64992,
#64993,#64994,#64995,#64996,#64997,#64998,#64999,#65000,#65001,#65002,#65003,
#65004,#65005,#65006,#65007,#65008,#65009,#65010,#65011,#65012,#65013,#65014,
#65015,#65016,#65017,#65018,#65019,#65020,#65021,#65022,#65023,#65024,#65025,
#65026,#65027,#65028,#65029,#65030,#65031,#65032,#65033,#65034,#65035,#65036,
#65037,#65038,#65039,#65040,#65041,#65042,#65043,#65044,#65045,#65046,#65047,
#65048,#65049,#65050,#65051,#65052,#65053,#65054,#65055,#65056,#65057,#65058,
#65059,#65060,#65061,#65062,#65063,#65064,#65065,#65066,#65067,#65068,#65069,
#65070,#65071,#65072,#65073,#65074,#65075,#65076,#65077,#65078,#65079,#65080,
#65081,#65082,#65083,#65084,#65085,#65086,#65087,#65088,#65089,#65090,#65091,
#65092,#65093,#65094,#65095,#65096,#65097,#65098,#65099,#65100,#65101,#65102,
#65103,#65104,#65105,#65106,#65107,#65108,#65109,#65110,#65111,#65112,#65113,
#65114,#65115,#65116,#65117,#65118,#65119,#65120,#65121,#65122,#65123,#65124,
#65125,#65126,#65127,#65128,#65129,#65130,#65131,#65132,#65133,#65134,#65135,
#65136,#65137,#65138,#65139,#65140,#65141,#65142,#65143,#65144,#65145,#65146,
#65147,#65148,#65149,#65150,#65151,#65152,#65153,#65154,#65155,#65156,#65157,
#65158,#65159,#65160,#65161,#65162,#65163,#65164,#65165,#65166,#65167,#65168,
#65169,#65170,#65171,#65172,#65173,#65174,#65175,#65176,#65177,#65178,#65179,
#65180,#65181,#65182,#65183,#65184,#65185,#65186,#65187,#65188,#65189,#65190,
#65191,#65192,#65193,#65194,#65195,#65196,#65197,#65198,#65199,#65200,#65201,
#65202,#65203,#65204,#65205,#65206,#65207,#65208,#65209,#65210,#65211,#65212,
#65213,#65214,#65215,#65216,#65217),.UNSPECIFIED.,.F.,.F.,(4,3,3,3,3,3,
3,3,3,3,3,3,3,3,3,3,3,3,3,3,3,3,3,3,3,3,3,3,3,3,3,3,3,3,3,3,3,3,3,3,3,3,
3,3,3,3,3,3,3,3,3,3,3,3,3,3,3,3,3,3,3,3,3,3,3,3,3,3,3,3,3,3,3,3,3,3,3,3,
3,3,4),(-98.3407100278245,-98.3398751109126,-98.2497923383696,-98.1594093744117,
-98.0690731139765,-97.9789567735724,-97.8891402262143,-97.8442804143033,
-97.7552175859449,-97.6724974832672,-97.6057318876503,-97.5390372049508,
-97.5057931159296,-97.3913563601377,-97.3450651360715,-97.2298028424745,
-97.1144050455794,-96.9994261646693,-96.8854619929382,-96.8461239064708,
-96.7342773273762,-96.6708762040348,-96.5912548848605,-96.5107793206893,
-96.4292551225898,-96.3799354774799,-96.2761438716762,-96.1689624435349,
-96.0652171864929,-95.9629223065681,-95.8638736849662,-95.847418159111,
-95.8359592921399,-95.7438149252361,-95.6479844699747,-95.5510733494601,
-95.4537908365631,-95.4185008361925,-95.3295095279158,-95.2413177536157,
-95.1543001375577,-95.0695592780133,-95.001042380245,-94.8989066470248,
-94.8483475199855,-94.7446888282949,-94.6404310244062,-94.5356081345725,
-94.43092383478,-94.3272430696066,-94.2541340789527,-94.1932522994489,-94.1661254683501,
-94.0819039095132,-93.9980018643696,-93.9148482355806,-93.8504898373246,
-93.7668082244376,-93.682989170877,-93.59965070049,-93.5842440152402,-93.5121655571065,
-93.4395403317008,-93.3663365921562,-93.3312085564552,-93.2476744079394,
-93.1640127763708,-93.0804884793871,-92.9971666819597,-92.9140745743315,
-92.8524988242307,-92.7672692310056,-92.6820396377804,-92.6021855545101,
-92.5207460562211,-92.4962916445604,-92.4066331146904,-92.3166043445123,
-92.2274393260093,-92.1407699558148,-92.0575247206449),.UNSPECIFIED.);
#548=B_SPLINE_CURVE_WITH_KNOTS('',3,(#65219,#65220,#65221,#65222,#65223,
#65224,#65225,#65226,#65227,#65228,#65229,#65230,#65231,#65232,#65233,#65234,
#65235,#65236),.UNSPECIFIED.,.F.,.F.,(4,2,2,2,2,2,2,2,4),(-92.0575247206449,
-91.2226078087501,-90.3876908968552,-89.5527739849604,-88.7178570730655,
-87.8829401611707,-87.0480232492758,-86.213106337381,-85.774546795447),
 .UNSPECIFIED.);
#549=B_SPLINE_CURVE_WITH_KNOTS('',3,(#65238,#65239,#65240,#65241,#65242,
#65243,#65244,#65245,#65246,#65247,#65248),.UNSPECIFIED.,.F.,.F.,(4,1,1,
1,1,1,1,1,4),(-85.7739081130952,-84.864680684328,-83.866272676277,-83.3670686722516,
-82.8678646682261,-81.8694566601752,-80.8710486521243,-79.8726406440734,
-79.4911610665801),.UNSPECIFIED.);
#550=B_SPLINE_CURVE_WITH_KNOTS('',3,(#65250,#65251,#65252,#65253,#65254,
#65255,#65256,#65257,#65258,#65259,#65260,#65261,#65262,#65263,#65264,#65265,
#65266,#65267,#65268,#65269,#65270,#65271,#65272,#65273,#65274,#65275,#65276,
#65277,#65278,#65279,#65280,#65281,#65282,#65283,#65284,#65285,#65286,#65287,
#65288,#65289,#65290,#65291,#65292,#65293,#65294,#65295,#65296,#65297,#65298,
#65299,#65300,#65301,#65302,#65303,#65304,#65305,#65306,#65307,#65308,#65309,
#65310,#65311,#65312,#65313,#65314,#65315,#65316,#65317,#65318,#65319,#65320,
#65321,#65322,#65323,#65324,#65325,#65326,#65327,#65328,#65329,#65330,#65331,
#65332,#65333,#65334,#65335,#65336,#65337,#65338,#65339,#65340,#65341,#65342,
#65343,#65344,#65345,#65346,#65347,#65348,#65349,#65350,#65351,#65352,#65353,
#65354,#65355,#65356,#65357,#65358,#65359,#65360,#65361,#65362,#65363,#65364,
#65365,#65366,#65367,#65368,#65369,#65370,#65371,#65372,#65373,#65374,#65375,
#65376,#65377,#65378,#65379,#65380,#65381,#65382,#65383,#65384,#65385,#65386,
#65387,#65388,#65389,#65390,#65391,#65392,#65393,#65394,#65395,#65396,#65397,
#65398,#65399,#65400,#65401,#65402,#65403,#65404,#65405,#65406,#65407,#65408,
#65409,#65410,#65411,#65412,#65413,#65414,#65415,#65416,#65417,#65418,#65419,
#65420,#65421,#65422,#65423,#65424,#65425,#65426,#65427,#65428,#65429,#65430,
#65431,#65432,#65433,#65434,#65435,#65436,#65437,#65438,#65439,#65440,#65441,
#65442,#65443,#65444,#65445,#65446,#65447,#65448,#65449,#65450,#65451,#65452,
#65453,#65454,#65455,#65456,#65457,#65458,#65459,#65460,#65461,#65462,#65463,
#65464,#65465,#65466,#65467,#65468,#65469,#65470,#65471,#65472,#65473,#65474,
#65475,#65476,#65477,#65478,#65479,#65480,#65481,#65482,#65483,#65484,#65485,
#65486,#65487,#65488,#65489,#65490,#65491,#65492,#65493,#65494,#65495,#65496,
#65497,#65498,#65499,#65500,#65501,#65502,#65503,#65504,#65505,#65506,#65507,
#65508,#65509,#65510,#65511,#65512,#65513,#65514),.UNSPECIFIED.,.F.,.F.,
(4,3,3,3,3,3,3,3,3,3,3,3,3,3,3,3,3,3,3,3,3,3,3,3,3,3,3,3,3,3,3,3,3,3,3,
3,3,3,3,3,3,3,3,3,3,3,3,3,3,3,3,3,3,3,3,3,3,3,3,3,3,3,3,3,3,3,3,3,3,3,3,
3,3,3,3,3,3,3,3,3,3,3,3,3,3,3,3,3,4),(-79.4911541062857,-79.4140389225028,
-79.3388515225128,-79.2636409863518,-79.1883959109838,-79.1098550922435,
-79.0344649991889,-78.9590167596919,-78.8834664025531,-78.8742326360225,
-78.8003391547687,-78.7265282886263,-78.652785593203,-78.5790966743082,
-78.5054471770817,-78.4318227758969,-78.3581949289715,-78.2845610629028,
-78.210908220688,-78.13722343648,-78.0634528835819,-77.9896341729666,-77.9157095220992,
-77.8758246279715,-77.8012015625577,-77.7266642336767,-77.6521987449237,
-77.5777912472822,-77.5034279300403,-77.4290950121387,-77.354768549544,
-77.2804422175887,-77.2061035587924,-77.1317401115139,-77.0573048543314,
-76.9828283809401,-76.9082620087988,-76.8774166199206,-76.7990509458789,
-76.7207817764409,-76.6426038300442,-76.564543057853,-76.4865539955989,
-76.4086541426038,-76.3782126158952,-76.3003020277817,-76.2223216308785,
-76.1442663010181,-76.0660815852632,-75.9878262056562,-75.9094515150197,
-75.8790086118697,-75.8044495153425,-75.7299658657305,-75.6555438026262,
-75.5811695061888,-75.5068291883977,-75.4325090846501,-75.3581802154919,
-75.2838419823009,-75.2094819239501,-75.1350875701474,-75.0606072165753,
-74.9860774635745,-74.9114457327325,-74.8806006038188,-74.8066808175414,
-74.7328478421853,-74.6590872165573,-74.5853845330293,-74.5117254263945,
-74.4380955635651,-74.3644684878882,-74.2908392588486,-74.2171949210857,
-74.1435225126251,-74.0697701851881,-73.9959730343537,-73.9220750077044,
-73.8821925957679,-73.8075920945069,-73.7326391825818,-73.6582186814261,
-73.5838517352182,-73.5095258513851,-73.4341365883154,-73.3598492930203,
-73.2839090460632,-73.2079687991061),.UNSPECIFIED.);
#551=B_SPLINE_CURVE_WITH_KNOTS('',3,(#65516,#65517,#65518,#65519,#65520,
#65521,#65522,#65523,#65524,#65525,#65526),.UNSPECIFIED.,.F.,.F.,(4,1,1,
1,1,1,1,1,4),(-73.2079618312794,-72.8837845877169,-71.885376579666,-70.8869685716151,
-69.8885605635642,-69.3893565595387,-68.8901525555133,-67.8917445474624,
-66.9249979083913),.UNSPECIFIED.);
#552=B_SPLINE_CURVE_WITH_KNOTS('',3,(#65528,#65529,#65530,#65531,#65532,
#65533,#65534,#65535,#65536,#65537,#65538,#65539,#65540,#65541,#65542,#65543,
#65544,#65545),.UNSPECIFIED.,.F.,.F.,(4,2,2,2,2,2,2,2,4),(-66.9246686944173,
-66.0898665800317,-65.2549496681368,-64.420032756242,-63.5851158443471,
-62.7501989324523,-61.9152820205574,-61.0803651086626,-60.641598184747),
 .UNSPECIFIED.);
#553=B_SPLINE_CURVE_WITH_KNOTS('',3,(#65547,#65548,#65549,#65550,#65551,
#65552,#65553,#65554,#65555,#65556,#65557,#65558,#65559,#65560,#65561,#65562,
#65563,#65564),.UNSPECIFIED.,.F.,.F.,(4,2,2,2,2,2,2,2,4),(-60.641598184747,
-59.8066812728521,-58.9717643609573,-58.1368474490624,-57.3019305371676,
-56.4670136252727,-55.6320967133778,-54.797179801483,-54.3584128775674),
 .UNSPECIFIED.);
#554=B_SPLINE_CURVE_WITH_KNOTS('',3,(#65566,#65567,#65568,#65569,#65570,
#65571,#65572,#65573,#65574,#65575,#65576),.UNSPECIFIED.,.F.,.F.,(4,1,1,
1,1,1,1,1,4),(-54.3584128775674,-53.9140324347495,-52.9156244266986,-51.9172164186477,
-50.9188084105968,-49.9204004025459,-48.9219923944949,-48.4227883904695,
-48.0756242030887),.UNSPECIFIED.);
#555=B_SPLINE_CURVE_WITH_KNOTS('',3,(#65578,#65579,#65580,#65581,#65582,
#65583,#65584,#65585,#65586,#65587,#65588,#65589,#65590,#65591,#65592,#65593,
#65594,#65595),.UNSPECIFIED.,.F.,.F.,(4,2,2,2,2,2,2,2,4),(-48.0751022683111,
-47.2403106584929,-46.405393746598,-45.5704768347031,-44.7355599228082,
-43.9006430109134,-43.0657260990185,-42.2308091871236,-41.792165349807),
 .UNSPECIFIED.);
#556=B_SPLINE_CURVE_WITH_KNOTS('',3,(#65597,#65598,#65599,#65600,#65601,
#65602,#65603,#65604,#65605,#65606,#65607),.UNSPECIFIED.,.F.,.F.,(4,1,1,
1,1,1,1,1,4),(-41.7916731482383,-41.4339323341131,-40.9347283300876,-39.9363203220367,
-38.9379123139858,-37.9395043059348,-36.9410962978839,-35.942688289833,
-35.5088569560286),.UNSPECIFIED.);
#557=B_SPLINE_CURVE_WITH_KNOTS('',3,(#65609,#65610,#65611,#65612,#65613,
#65614,#65615,#65616,#65617,#65618,#65619,#65620,#65621,#65622,#65623,#65624,
#65625,#65626,#65627,#65628,#65629,#65630,#65631,#65632,#65633,#65634,#65635,
#65636,#65637,#65638,#65639,#65640,#65641,#65642,#65643,#65644,#65645,#65646,
#65647,#65648,#65649,#65650,#65651,#65652,#65653,#65654,#65655,#65656,#65657,
#65658,#65659,#65660,#65661,#65662,#65663,#65664,#65665,#65666,#65667,#65668,
#65669,#65670,#65671,#65672,#65673,#65674,#65675,#65676,#65677,#65678,#65679,
#65680,#65681,#65682,#65683,#65684,#65685,#65686,#65687,#65688,#65689,#65690,
#65691,#65692,#65693,#65694,#65695,#65696,#65697,#65698,#65699,#65700,#65701,
#65702,#65703,#65704,#65705,#65706,#65707,#65708,#65709,#65710,#65711,#65712,
#65713,#65714,#65715,#65716,#65717,#65718,#65719,#65720,#65721,#65722,#65723,
#65724,#65725,#65726,#65727,#65728,#65729,#65730,#65731,#65732,#65733,#65734,
#65735,#65736,#65737,#65738,#65739,#65740,#65741,#65742,#65743,#65744,#65745,
#65746,#65747,#65748,#65749,#65750,#65751,#65752,#65753,#65754,#65755,#65756,
#65757,#65758,#65759,#65760,#65761,#65762,#65763,#65764,#65765,#65766,#65767,
#65768,#65769,#65770,#65771,#65772,#65773,#65774,#65775,#65776,#65777,#65778,
#65779,#65780,#65781,#65782,#65783,#65784,#65785,#65786,#65787,#65788,#65789,
#65790,#65791,#65792,#65793,#65794,#65795,#65796,#65797,#65798,#65799,#65800,
#65801,#65802,#65803,#65804,#65805,#65806,#65807,#65808,#65809,#65810,#65811,
#65812,#65813,#65814,#65815,#65816,#65817,#65818,#65819,#65820,#65821,#65822,
#65823,#65824,#65825,#65826,#65827,#65828,#65829,#65830,#65831,#65832,#65833,
#65834,#65835,#65836,#65837,#65838,#65839,#65840,#65841,#65842,#65843,#65844,
#65845,#65846),.UNSPECIFIED.,.F.,.F.,(4,3,3,3,3,3,3,3,3,3,3,3,3,3,3,3,3,
3,3,3,3,3,3,3,3,3,3,3,3,3,3,3,3,3,3,3,3,3,3,3,3,3,3,3,3,3,3,3,3,3,3,3,3,
3,3,3,3,3,3,3,3,3,3,3,3,3,3,3,3,3,3,3,3,3,3,3,3,3,3,4),(-35.5088569560286,
-35.5080220391167,-35.4078226390595,-35.3069421369146,-35.2059486885099,
-35.105244626726,-35.0050126956435,-34.9446638723629,-34.8458356537844,
-34.7591101236746,-34.7092184675934,-34.6739400441337,-34.5831464955377,
-34.4908340657363,-34.4450138153475,-34.3507477017669,-34.2564815881863,
-34.1463815848413,-34.0363558288672,-33.9460902199452,-33.8390231322389,
-33.7510601187875,-33.6605691285795,-33.5688148214294,-33.4758388293184,
-33.4215646762915,-33.3042274288324,-33.1904896172914,-33.0844504646164,
-33.004106220344,-32.9476783657108,-32.8536744421173,-32.7592046327776,
-32.6643487376451,-32.5866477643965,-32.4997781842343,-32.4120965402195,
-32.3250698966745,-32.2402926429357,-32.1691893084491,-32.0750415190886,
-31.9820995782183,-31.9488402515311,-31.8561241312604,-31.7622897538461,
-31.6684546500954,-31.5873078553393,-31.5117019803102,-31.4355870580904,
-31.3593882068004,-31.3342723965543,-31.2551135477029,-31.1760459938561,
-31.0971771530997,-31.0185521244204,-30.9509227757793,-30.8721831335571,
-30.7937911100304,-30.7523909434444,-30.6822918968919,-30.6117873185264,
-30.5407351827176,-30.4993554846594,-30.4114258939849,-30.3232470914475,
-30.230635044061,-30.1426420911496,-30.0548682539713,-29.9674611296698,
-29.9527989019017,-29.8663222153201,-29.8142264196547,-29.757682515458,
-29.7011770307223,-29.6644385727646,-29.578284095983,-29.4901309841995,
-29.4022684992888,-29.3139700740689,-29.225671648849),.UNSPECIFIED.);
#558=B_SPLINE_CURVE_WITH_KNOTS('',3,(#65848,#65849,#65850,#65851,#65852,
#65853,#65854,#65855,#65856,#65857,#65858,#65859,#65860,#65861,#65862,#65863,
#65864,#65865,#65866,#65867,#65868,#65869,#65870,#65871,#65872,#65873,#65874,
#65875,#65876,#65877,#65878,#65879,#65880,#65881,#65882,#65883,#65884,#65885,
#65886,#65887,#65888,#65889,#65890,#65891,#65892,#65893,#65894,#65895,#65896,
#65897,#65898,#65899,#65900,#65901,#65902,#65903,#65904,#65905,#65906,#65907,
#65908,#65909,#65910,#65911,#65912,#65913,#65914,#65915,#65916,#65917,#65918,
#65919,#65920,#65921,#65922,#65923,#65924,#65925,#65926,#65927,#65928,#65929,
#65930,#65931,#65932,#65933,#65934,#65935,#65936,#65937,#65938,#65939,#65940,
#65941,#65942,#65943,#65944,#65945,#65946,#65947,#65948,#65949,#65950,#65951,
#65952,#65953,#65954,#65955,#65956,#65957,#65958,#65959,#65960,#65961,#65962,
#65963,#65964,#65965,#65966,#65967,#65968,#65969,#65970,#65971,#65972,#65973,
#65974,#65975,#65976,#65977,#65978,#65979,#65980,#65981,#65982,#65983,#65984,
#65985,#65986,#65987,#65988,#65989,#65990,#65991,#65992,#65993,#65994,#65995,
#65996,#65997,#65998,#65999,#66000,#66001,#66002,#66003,#66004,#66005,#66006,
#66007,#66008,#66009,#66010,#66011,#66012,#66013,#66014,#66015,#66016,#66017,
#66018,#66019,#66020,#66021,#66022,#66023,#66024,#66025,#66026,#66027,#66028,
#66029,#66030,#66031,#66032,#66033,#66034,#66035,#66036,#66037,#66038,#66039,
#66040,#66041,#66042,#66043,#66044,#66045,#66046,#66047,#66048,#66049,#66050,
#66051,#66052,#66053,#66054,#66055,#66056,#66057,#66058,#66059,#66060,#66061,
#66062,#66063,#66064,#66065,#66066,#66067,#66068,#66069,#66070,#66071,#66072,
#66073,#66074,#66075,#66076,#66077,#66078,#66079,#66080,#66081,#66082,#66083,
#66084,#66085,#66086,#66087,#66088,#66089,#66090,#66091,#66092,#66093,#66094,
#66095,#66096,#66097,#66098,#66099,#66100,#66101,#66102,#66103,#66104,#66105,
#66106,#66107,#66108,#66109,#66110,#66111,#66112,#66113,#66114,#66115,#66116,
#66117,#66118,#66119,#66120,#66121,#66122,#66123,#66124,#66125,#66126,#66127,
#66128,#66129,#66130,#66131,#66132,#66133,#66134,#66135,#66136,#66137,#66138,
#66139,#66140,#66141,#66142,#66143,#66144,#66145,#66146,#66147,#66148,#66149,
#66150,#66151,#66152,#66153,#66154,#66155,#66156,#66157,#66158,#66159,#66160,
#66161,#66162,#66163,#66164,#66165,#66166,#66167,#66168,#66169,#66170,#66171,
#66172,#66173,#66174,#66175,#66176,#66177,#66178,#66179,#66180,#66181,#66182,
#66183,#66184,#66185,#66186,#66187,#66188,#66189,#66190,#66191,#66192,#66193,
#66194,#66195,#66196,#66197,#66198,#66199,#66200,#66201,#66202,#66203,#66204,
#66205,#66206,#66207,#66208,#66209,#66210,#66211,#66212,#66213,#66214,#66215,
#66216,#66217,#66218,#66219,#66220,#66221,#66222,#66223,#66224,#66225,#66226,
#66227,#66228,#66229,#66230,#66231,#66232,#66233,#66234,#66235,#66236,#66237,
#66238,#66239,#66240,#66241,#66242,#66243,#66244,#66245,#66246,#66247,#66248,
#66249,#66250,#66251,#66252,#66253,#66254,#66255,#66256,#66257,#66258,#66259,
#66260,#66261,#66262,#66263,#66264,#66265,#66266,#66267,#66268,#66269,#66270,
#66271,#66272,#66273,#66274,#66275,#66276,#66277,#66278,#66279,#66280,#66281,
#66282,#66283,#66284,#66285,#66286,#66287,#66288,#66289,#66290,#66291,#66292,
#66293,#66294,#66295,#66296,#66297,#66298,#66299,#66300,#66301,#66302,#66303,
#66304,#66305,#66306,#66307,#66308,#66309,#66310,#66311,#66312,#66313,#66314,
#66315,#66316,#66317,#66318,#66319,#66320,#66321,#66322,#66323,#66324,#66325,
#66326,#66327,#66328,#66329,#66330,#66331,#66332,#66333,#66334,#66335,#66336,
#66337,#66338,#66339,#66340,#66341,#66342,#66343,#66344,#66345,#66346,#66347,
#66348,#66349,#66350,#66351,#66352,#66353,#66354,#66355,#66356,#66357,#66358,
#66359,#66360,#66361,#66362,#66363,#66364,#66365,#66366,#66367,#66368,#66369,
#66370,#66371,#66372,#66373,#66374,#66375,#66376,#66377,#66378,#66379,#66380,
#66381,#66382,#66383,#66384,#66385,#66386,#66387,#66388,#66389,#66390,#66391,
#66392,#66393,#66394,#66395,#66396,#66397,#66398,#66399,#66400,#66401,#66402,
#66403,#66404,#66405,#66406,#66407),.UNSPECIFIED.,.F.,.F.,(4,2,2,2,2,2,
2,2,2,2,2,2,2,2,2,2,2,2,2,2,2,2,2,2,2,2,2,2,2,2,2,2,2,2,2,2,2,2,2,2,2,2,
2,2,2,2,2,2,2,2,2,2,2,2,2,2,2,2,2,2,2,2,2,2,2,2,2,2,2,2,2,2,2,2,2,2,2,2,
2,2,2,2,2,2,2,2,2,2,2,2,2,2,2,2,2,2,2,2,2,2,2,2,2,2,2,2,2,2,2,2,2,2,2,2,
2,2,2,2,2,2,2,2,2,2,2,2,2,2,2,2,2,2,2,2,2,2,2,2,2,2,2,2,2,2,2,2,2,2,2,2,
2,2,2,2,2,2,2,2,2,2,2,2,2,2,2,2,2,2,2,2,2,2,2,2,2,2,2,2,2,2,2,2,2,2,2,2,
2,2,2,2,2,2,2,2,2,2,2,2,2,2,2,2,2,2,2,2,2,2,2,2,2,2,2,2,2,2,2,2,2,2,2,2,
2,2,2,2,2,2,2,2,2,2,2,2,2,2,2,2,2,2,2,2,2,2,2,2,2,2,2,2,2,2,2,2,2,2,2,2,
2,2,2,2,2,2,2,2,2,2,2,2,2,2,2,2,2,2,2,2,2,4),(0.00156532237835257,0.17091198575568,
0.207222044334215,0.213114571822337,0.214859008958513,0.21593723683326,
0.216920339048251,0.218180441939555,0.220252266223459,0.231571329861011,
0.232374313989906,0.421839154393626,0.441471010575572,0.45895600194081,
0.496527568298866,0.620284332679301,0.625704004424397,0.628130491401357,
0.629936452366404,0.631617985894264,0.633920560157569,0.639692817873232,
0.704397104304271,0.831718616604965,0.897726105172791,0.979889125669097,
1.01542845563187,1.02210293679107,1.02428389357666,1.02568464164343,1.02699850312874,
1.02871830861566,1.03161118657523,1.0490064374067,1.23167620699884,1.32241227949923,
1.36745586561959,1.39252393554242,1.39823731160618,1.4009526180676,1.40350295568623,
1.40619311151654,1.40994760655908,1.4176164505781,1.49633768409118,1.61407369888607,
1.70869963385546,1.76494143491077,1.77504926126684,1.77758213928747,1.77906146779443,
1.78035682133211,1.78195784055565,1.78439717193456,1.79498606567316,1.94322770270387,
2.03919426651885,2.13822307967879,2.15423385763598,2.16956404976285,2.17315533580032,
2.1752099541776,2.1768052663174,2.1786154504831,2.18201236143277,2.19348056050792,
2.35556996007128,2.47745658925013,2.52751920776311,2.57868561417901,2.5858835663221,
2.58774864820281,2.58884947920185,2.58982835895663,2.59106415765009,2.59299829580082,
2.60217579955307,2.74132338282202,2.83059035182472,2.91432313816549,2.95587350324658,
2.97831503175031,2.98245753596772,2.98462106226711,2.98621278202622,2.98793169076646,
2.99092079530467,2.99936298900047,3.12377123290145,3.27438478098718,3.344449639781,
3.37694349084083,3.3796949179669,3.38100138450275,3.38192206805785,3.38287946950333,
3.38419822687073,3.38683677495832,3.40947362848246,3.53937227605842,3.69126386474088,
3.76354160547186,3.7712511287355,3.77697651393606,3.77952774811514,3.78139913749344,
3.7831222778922,3.78545238950731,3.79114632494279,3.84772510466974,3.89428917158918,
4.0797698411106,4.11179213214894,4.14970406585538,4.16597163644554,4.16845506224293,
4.169733632886,4.17076587052824,4.17195526839645,4.17397262786818,4.18125801802497,
4.29057331604547,4.46630886885966,4.55034907080562,4.55570588938883,4.55816553348199,
4.56002159322068,4.56176837821911,4.56418972654398,4.56908033885465,4.6133189880826,
4.6335836262616,4.83742579194341,4.90010496954302,4.94859638373132,4.95569551757532,
4.95759889516182,4.95873495671618,4.95974483635744,4.96101287277483,4.96348016474068,
4.97764364645044,5.00914422764245,5.06583248171667,5.33250055608807,5.34879440441641,
5.35226230016677,5.3544855010552,5.35625083866129,5.35823138303028,5.36153740835061,
5.3737467498349,5.45360670002394,5.60629983614269,5.73985202249173,5.74834712965012,
5.75022802371263,5.75144721071487,5.7524243432637,5.75353588678314,5.75544973085389,
5.76321694698121,5.82397826486286,5.88385225661824,6.06049972388032,6.09418470132512,
6.15538855396458,6.16108400927817,6.16337286417672,6.16505053529474,6.16685820374977,
6.16929717513358,6.17466579819149,6.18184257204658,6.2475354714967,6.39663328727209,
6.49356792896584,6.55407445078301,6.55837994976079,6.56007512299525,6.56130534236182,
6.5624876963338,6.5641646236099,6.56763252385029,6.60099662200162,6.6654308425079,
6.91498632094265,6.92983507866367,6.93479076784127,6.93756979963217,6.940320018155,
6.94368831065719,6.94731092978816,6.9530111204984,6.96385462201226,7.0243742017623,
7.08283889007759,7.29986043561504,7.31061465140634,7.31306549767383,7.31466883456716,
7.31583470102624,7.31726951457356,7.3196046408652,7.32762656154413,7.37575038783523,
7.40613398370776,7.5658047327608,7.69753177017189,7.70642659746195,7.70949467328503,
7.71123834266517,7.71284027042881,7.71499856283841,7.71898658129515,7.73639492694558,
7.76950801501643,7.8501973758505,7.92069692995797,8.10892538928674,8.10945343827896,
8.12089009653594,8.12296859413053,8.12423041706083,8.1252134091904,8.12629006813002,
8.12802879177178,8.13387312449858,8.1697202082136,8.23781482028477,8.31223464550103,
8.40171163419133,8.45150171697918,8.45997506133572,8.46625489428652,8.46826786736495,
8.51216207554354,8.51743462767127,8.51979593742876,8.52158606653488,8.52348126375185,
8.52540708939205,8.53107899814716,8.5915877747844,8.67948461743734,8.9001746809301,
8.91319202847375,8.91538019121428,8.91669279506628,8.91771089239394,8.9188113106224,
8.92055604854181,8.92614334966688,8.95889910609161,9.02907506070383,9.10307630689263,
9.14101548565173,9.18836401865907,9.30373870124536,9.31159270675471,9.31456095996236,
9.31632104103345,9.31798555639991,9.31976121288474,9.32201769810091,9.32548479189891,
9.36082397496341,9.41954965255361,9.46215601694711,9.66516308305237,9.68232515367044,
9.70106288747595,9.70359777460581,9.70490459607476,9.70587290571473,9.70693226598835,
9.70840375989528,9.71190547133014,9.81939241609079,9.95375608942013),
 .UNSPECIFIED.);
#559=B_SPLINE_CURVE_WITH_KNOTS('',3,(#66408,#66409,#66410,#66411,#66412,
#66413,#66414,#66415,#66416,#66417,#66418,#66419,#66420,#66421,#66422,#66423,
#66424,#66425,#66426,#66427,#66428,#66429,#66430,#66431,#66432,#66433,#66434,
#66435,#66436,#66437,#66438,#66439,#66440,#66441,#66442,#66443,#66444,#66445,
#66446,#66447,#66448,#66449,#66450,#66451,#66452,#66453,#66454,#66455,#66456,
#66457,#66458,#66459,#66460,#66461,#66462,#66463,#66464,#66465,#66466,#66467,
#66468,#66469,#66470,#66471,#66472,#66473,#66474,#66475,#66476,#66477,#66478,
#66479,#66480,#66481,#66482,#66483,#66484,#66485,#66486,#66487,#66488,#66489,
#66490,#66491,#66492,#66493,#66494,#66495,#66496,#66497,#66498,#66499,#66500,
#66501,#66502,#66503,#66504,#66505,#66506,#66507,#66508,#66509,#66510,#66511,
#66512,#66513,#66514,#66515,#66516,#66517,#66518,#66519,#66520,#66521,#66522,
#66523,#66524,#66525,#66526,#66527,#66528,#66529,#66530,#66531,#66532,#66533,
#66534,#66535,#66536,#66537,#66538,#66539,#66540,#66541,#66542,#66543,#66544,
#66545,#66546,#66547,#66548,#66549,#66550,#66551,#66552,#66553,#66554,#66555,
#66556,#66557,#66558,#66559,#66560,#66561,#66562,#66563,#66564,#66565,#66566,
#66567,#66568,#66569,#66570,#66571,#66572,#66573,#66574,#66575,#66576,#66577,
#66578,#66579,#66580,#66581,#66582,#66583,#66584,#66585,#66586,#66587,#66588,
#66589,#66590,#66591,#66592,#66593,#66594,#66595,#66596,#66597,#66598,#66599,
#66600,#66601,#66602,#66603,#66604,#66605,#66606,#66607,#66608,#66609,#66610,
#66611,#66612,#66613,#66614,#66615,#66616,#66617,#66618,#66619,#66620,#66621,
#66622,#66623,#66624,#66625,#66626,#66627,#66628,#66629,#66630,#66631,#66632,
#66633,#66634,#66635,#66636,#66637,#66638,#66639,#66640,#66641,#66642,#66643,
#66644,#66645,#66646,#66647,#66648,#66649,#66650,#66651,#66652,#66653,#66654,
#66655,#66656,#66657,#66658,#66659,#66660,#66661,#66662,#66663,#66664,#66665,
#66666,#66667,#66668,#66669,#66670,#66671,#66672,#66673,#66674,#66675,#66676,
#66677,#66678,#66679,#66680,#66681,#66682,#66683,#66684,#66685,#66686,#66687,
#66688,#66689,#66690,#66691,#66692,#66693,#66694,#66695,#66696,#66697,#66698,
#66699,#66700,#66701,#66702,#66703,#66704,#66705,#66706,#66707,#66708,#66709,
#66710,#66711,#66712,#66713,#66714,#66715,#66716,#66717,#66718,#66719,#66720,
#66721,#66722,#66723,#66724,#66725,#66726,#66727,#66728,#66729,#66730,#66731,
#66732,#66733,#66734,#66735,#66736,#66737,#66738,#66739,#66740,#66741,#66742,
#66743,#66744,#66745,#66746,#66747,#66748,#66749,#66750,#66751,#66752,#66753,
#66754,#66755,#66756,#66757,#66758,#66759,#66760,#66761,#66762,#66763,#66764,
#66765,#66766,#66767,#66768,#66769,#66770,#66771,#66772,#66773,#66774,#66775,
#66776,#66777,#66778,#66779,#66780,#66781,#66782,#66783,#66784,#66785,#66786,
#66787,#66788,#66789,#66790,#66791,#66792,#66793,#66794,#66795,#66796,#66797,
#66798,#66799,#66800,#66801,#66802,#66803,#66804,#66805,#66806,#66807,#66808,
#66809,#66810,#66811,#66812,#66813,#66814,#66815,#66816,#66817,#66818,#66819,
#66820,#66821,#66822,#66823,#66824,#66825,#66826,#66827,#66828,#66829,#66830,
#66831,#66832,#66833,#66834,#66835,#66836,#66837,#66838,#66839,#66840,#66841,
#66842,#66843,#66844,#66845,#66846,#66847,#66848,#66849,#66850,#66851,#66852,
#66853,#66854,#66855,#66856,#66857,#66858,#66859,#66860,#66861,#66862,#66863,
#66864,#66865,#66866,#66867,#66868,#66869,#66870,#66871,#66872,#66873,#66874,
#66875,#66876,#66877,#66878,#66879,#66880,#66881,#66882,#66883,#66884,#66885,
#66886,#66887,#66888,#66889,#66890,#66891,#66892,#66893,#66894,#66895,#66896,
#66897,#66898,#66899,#66900,#66901,#66902,#66903,#66904,#66905,#66906,#66907,
#66908,#66909,#66910,#66911,#66912,#66913,#66914,#66915,#66916,#66917,#66918,
#66919,#66920,#66921,#66922,#66923,#66924,#66925,#66926,#66927,#66928,#66929,
#66930,#66931,#66932,#66933,#66934,#66935,#66936,#66937,#66938,#66939,#66940,
#66941,#66942,#66943,#66944,#66945,#66946,#66947,#66948,#66949,#66950,#66951,
#66952,#66953,#66954,#66955,#66956,#66957,#66958,#66959,#66960,#66961,#66962,
#66963,#66964,#66965,#66966,#66967,#66968,#66969,#66970,#66971,#66972,#66973,
#66974,#66975,#66976,#66977,#66978,#66979),.UNSPECIFIED.,.F.,.F.,(4,2,2,
2,2,2,2,2,2,2,2,2,2,2,2,2,2,2,2,2,2,2,2,2,2,2,2,2,2,2,2,2,2,2,2,2,2,2,2,
2,2,2,2,2,2,2,2,2,2,2,2,2,2,2,2,2,2,2,2,2,2,2,2,2,2,2,2,2,2,2,2,2,2,2,2,
2,2,2,2,2,2,2,2,2,2,2,2,2,2,2,2,2,2,2,2,2,2,2,2,2,2,2,2,2,2,2,2,2,2,2,2,
2,2,2,2,2,2,2,2,2,2,2,2,2,2,2,2,2,2,2,2,2,2,2,2,2,2,2,2,2,2,2,2,2,2,2,2,
2,2,2,2,2,2,2,2,2,2,2,2,2,2,2,2,2,2,2,2,2,2,2,2,2,2,2,2,2,2,2,2,2,2,2,2,
2,2,2,2,2,2,2,2,2,2,2,2,2,2,2,2,2,2,2,2,2,2,2,2,2,2,2,2,2,2,2,2,2,2,2,2,
2,2,2,2,2,2,2,2,2,2,2,2,2,2,2,2,2,2,2,2,2,2,2,2,2,2,2,2,2,2,2,2,2,2,2,2,
2,2,2,2,2,2,2,2,2,2,2,2,2,2,2,2,2,2,2,2,2,2,2,2,2,2,2,2,2,2,4),(0.00230660127850738,
0.128345221299926,0.134920681005092,0.138444386242725,0.140724949474323,
0.142508472062085,0.144177389799666,0.145928375692367,0.148364814814351,
0.154681539308349,0.238875327581102,0.276509332655191,0.287233309423933,
0.473069833707347,0.537672296612725,0.540906916335336,0.542312915935396,
0.543342879364206,0.544290082307809,0.545569450243708,0.5487438631145,0.583747592806631,
0.78634720366351,0.847112789003208,0.905598660780656,0.923021431936684,
0.933872207622032,0.936219605831329,0.937987456768179,0.939783021604548,
0.941444244688455,0.943702663790448,0.949281257397128,1.00734723993167,
1.07414691052537,1.157715840318,1.16787183435951,1.17948683764632,1.19290049275817,
1.20863044925713,1.22756443935456,1.29639674228562,1.32754297526308,1.33289680491233,
1.33458009829973,1.33564457361223,1.3366317942913,1.33792121116186,1.34076453027969,
1.36312884601792,1.56197401493471,1.66178182418684,1.71630562546323,1.73307022502847,
1.74362884824775,1.74596989535025,1.74816415585285,1.74994003945794,1.75170832830087,
1.75489757584768,1.76468077755972,1.90701099886728,2.05730317281499,2.08461541888431,
2.1333582496924,2.14143935599111,2.14378098857757,2.14521741964217,2.14638333802988,
2.14798473875959,2.15042892032036,2.16110029256818,2.37628271934823,2.43521607290879,
2.49681578006484,2.50792333901872,2.51372459313611,2.51738987593,2.52078648865102,
2.52354038564477,2.52630310747086,2.53117715381897,2.54542750470412,2.7918392715674,
2.84929342443344,2.88896022903573,2.8957843922249,2.89798335465623,2.89938784519667,
2.90069970591071,2.90240880974919,2.9061387035619,2.93826085567872,2.94174329558787,
2.95514697192867,2.97924175159734,3.05224976599085,3.15913856134385,3.25331654834907,
3.28677108277123,3.29199599100632,3.2944331146302,3.29624057798281,3.29791888993328,
3.30020990163617,3.30591727664759,3.36758624221959,3.42175484108784,3.58915467387187,
3.65151698971242,3.69894673490316,3.70585918591164,3.70769819521392,3.70879321949632,
3.70977317851828,3.71101843987944,3.71298314717672,3.72257483818995,3.87303308975443,
4.01914424311439,4.09605319841951,4.10164296966842,4.10408832386243,4.1058860006037,
4.10754402157203,4.1097902289916,4.11529947943244,4.1707324262075,4.39503258938269,
4.45173176096255,4.4833223073281,4.49778884667176,4.50011295118531,4.50133568971659,
4.50234226643736,4.50351112526991,4.50550853085898,4.51286867514984,4.62210180040717,
4.77700987720342,4.83307348977952,4.88616788589078,4.89579457589138,4.89890218937483,
4.90088856190432,4.90274504239576,4.90516547629103,4.90921284607816,4.93293175548031,
4.94410876979255,4.95209591288574,4.98036213696699,5.03851983158081,5.26493346155454,
5.28560182345081,5.28850058350351,5.2898478001113,5.29089006673285,5.29202497430403,
5.29385308129089,5.2999563389031,5.36670758665547,5.48510936851614,5.66216643158317,
5.6739141294271,5.67740818314465,5.67927338924316,5.68091900195438,5.68304090309669,
5.6867570949866,5.70273044109283,5.73111623245015,5.78306163032006,6.00348430390019,
6.04266633459154,6.04552718570898,6.04809754522921,6.05131497396005,6.07448089261174,
6.07743121040447,6.07877042537367,6.07979289479764,6.08088226325311,6.08258262450377,
6.08799872927215,6.11962239041733,6.16620548944169,6.28477887436226,6.45786471015039,
6.4696825710734,6.47310373408216,6.47511130885555,6.47685817416462,6.47903750820815,
6.48324994677044,6.51027789042411,6.57055824293226,6.6805624832239,6.85933012443352,
6.86849540404132,6.87042968254335,6.87166606881031,6.87264573403327,6.8737251276232,
6.87553041241013,6.87769673323445,6.88197942829283,7.01139060248478,7.21690260981582,
7.27565974944715,7.28129550649728,7.28357496460972,7.28525090397973,7.28706164310502,
7.28951346022059,7.29506951458921,7.3761168334038,7.47051139731932,7.66410799346736,
7.6764962685436,7.6790635898108,7.68069669816208,7.68195812208696,7.68335631094932,
7.6856149414343,7.68829790976247,7.69348615884106,7.70620794947686,7.74904395165377,
7.81074717894133,8.03568726524247,8.04944531275463,8.05417144639542,8.05685485940246,
8.05931959978896,8.06262292863043,8.06875449169653,8.10189391594875,8.1656505340179,
8.28216252427989,8.40883989268998,8.43040719690892,8.43381011908805,8.43546047111226,
8.43669707232212,8.43806938165352,8.44023563622075,8.44276388066525,8.44751142388798,
8.45853056711512,8.49505075917323,8.52664168920347,8.81104765590495,8.82767841720906,
8.83117233643037,8.83340383151837,8.83517038255303,8.83714664447517,8.84043226537289,
8.85242323119308,8.92947229407872,9.05134171018654,9.10292432586987,9.16474973800832,
9.21340043738603,9.24164175279483,9.24436266525319,9.24567287580225,9.24660748479505,
9.24749783839472,9.24845060594464,9.24966918715297,9.25447493580103,9.31035283527648,
9.34706401935888,9.58339405392858,9.63639247904457,9.64141583360316,9.64383091101246,
9.64554061864745,9.64714914952137,9.64937505856541,9.65377537708792,9.6855358940007,
9.78208413797257,9.95839499409821),.UNSPECIFIED.);
#560=B_SPLINE_CURVE_WITH_KNOTS('',3,(#67039,#67040,#67041,#67042,#67043,
#67044,#67045,#67046,#67047,#67048,#67049,#67050,#67051,#67052,#67053,#67054,
#67055,#67056,#67057,#67058,#67059,#67060,#67061,#67062,#67063,#67064,#67065,
#67066,#67067,#67068),.UNSPECIFIED.,.F.,.F.,(4,2,2,2,2,2,2,2,2,2,2,2,2,
2,4),(-5.1172649587789,-4.77125985892989,-4.39072557177308,-3.78322541506865,
-3.21302721090485,-2.63736934344719,-2.17538637120503,-1.75347930631198,
-1.43774045964503,-1.15825087501937,-0.854608089732673,-0.620651733076443,
-0.367068559363653,-0.196690632762468,-0.000776879412541869),
 .UNSPECIFIED.);
#561=B_SPLINE_CURVE_WITH_KNOTS('',3,(#67069,#67070,#67071,#67072,#67073,
#67074,#67075,#67076,#67077,#67078,#67079,#67080,#67081,#67082,#67083,#67084,
#67085,#67086,#67087,#67088,#67089,#67090,#67091,#67092,#67093,#67094,#67095,
#67096,#67097,#67098,#67099,#67100,#67101,#67102,#67103,#67104,#67105,#67106,
#67107,#67108,#67109,#67110,#67111,#67112,#67113,#67114,#67115,#67116,#67117,
#67118,#67119,#67120,#67121,#67122,#67123,#67124,#67125,#67126,#67127,#67128,
#67129,#67130,#67131,#67132,#67133,#67134,#67135,#67136,#67137,#67138),
 .UNSPECIFIED.,.F.,.F.,(4,3,3,3,3,3,3,3,3,3,3,3,3,3,3,3,3,3,3,3,3,3,3,4),
(-1.12803176442304,-1.06660631931699,-1.00636787721923,-0.961112508690392,
-0.899376762802759,-0.85939191897837,-0.849462260101921,-0.842475058397111,
-0.782885726971055,-0.72274595667072,-0.662901991936166,-0.604134381573305,
-0.579498012207646,-0.565265641437903,-0.554476152855422,-0.547373062825023,
-0.489041380710527,-0.430655486338116,-0.372940968315836,-0.315893092681781,
-0.290970068308981,-0.275474495988932,-0.266102779271428,-0.216200995190583),
 .UNSPECIFIED.);
#562=B_SPLINE_CURVE_WITH_KNOTS('',3,(#69371,#69372,#69373,#69374,#69375,
#69376,#69377,#69378,#69379,#69380,#69381,#69382,#69383,#69384,#69385,#69386,
#69387,#69388,#69389,#69390,#69391,#69392,#69393,#69394,#69395,#69396,#69397,
#69398,#69399,#69400,#69401,#69402,#69403,#69404,#69405,#69406,#69407,#69408,
#69409,#69410,#69411,#69412,#69413,#69414,#69415,#69416,#69417,#69418,#69419,
#69420,#69421,#69422,#69423,#69424,#69425,#69426,#69427,#69428,#69429,#69430,
#69431,#69432,#69433,#69434,#69435,#69436,#69437,#69438,#69439,#69440,#69441,
#69442,#69443,#69444,#69445,#69446,#69447,#69448,#69449,#69450,#69451,#69452,
#69453,#69454,#69455,#69456,#69457,#69458,#69459,#69460,#69461,#69462,#69463,
#69464,#69465,#69466,#69467,#69468,#69469,#69470,#69471,#69472,#69473,#69474,
#69475,#69476,#69477,#69478,#69479),.UNSPECIFIED.,.F.,.F.,(4,3,3,3,3,3,
3,3,3,3,3,3,3,3,3,3,3,3,3,3,3,3,3,3,3,3,3,3,3,3,3,3,3,3,3,3,4),(-1.52870610664526,
-1.4669968085376,-1.40516063220429,-1.34270018454279,-1.32404855442001,
-1.31376060856527,-1.25232916205104,-1.19058262877584,-1.12913545396555,
-1.1198174668383,-1.11189637748511,-1.05127683134977,-0.9908173650714,-0.93102541318309,
-0.875002691406706,-0.832985650074418,-0.821141831585003,-0.762941140003209,
-0.706934526077554,-0.648166878086584,-0.589327029396728,-0.558993140800858,
-0.547233056843969,-0.537331142832007,-0.47987739433253,-0.42225444188307,
-0.365147363201414,-0.346655920629775,-0.30332393055107,-0.283703366897939,
-0.271772304256833,-0.26150992201455,-0.205232539959138,-0.149113591098172,
-0.0934593024883868,-0.0388976662899543,-1.34448406245148E-13),
 .UNSPECIFIED.);
#563=B_SPLINE_CURVE_WITH_KNOTS('',3,(#71716,#71717,#71718,#71719,#71720,
#71721,#71722,#71723,#71724,#71725,#71726,#71727,#71728,#71729,#71730,#71731,
#71732,#71733,#71734,#71735,#71736,#71737,#71738,#71739,#71740,#71741,#71742,
#71743,#71744,#71745,#71746,#71747,#71748,#71749,#71750,#71751,#71752,#71753,
#71754,#71755,#71756,#71757,#71758,#71759,#71760,#71761,#71762,#71763,#71764,
#71765,#71766,#71767,#71768,#71769,#71770,#71771,#71772,#71773,#71774,#71775,
#71776,#71777,#71778,#71779,#71780,#71781,#71782,#71783,#71784,#71785,#71786,
#71787,#71788,#71789,#71790,#71791,#71792,#71793,#71794,#71795,#71796,#71797,
#71798,#71799,#71800,#71801,#71802,#71803,#71804,#71805,#71806,#71807,#71808,
#71809,#71810,#71811,#71812,#71813,#71814,#71815,#71816,#71817,#71818,#71819,
#71820,#71821,#71822,#71823,#71824),.UNSPECIFIED.,.F.,.F.,(4,3,3,3,3,3,
3,3,3,3,3,3,3,3,3,3,3,3,3,3,3,3,3,3,3,3,3,3,3,3,3,3,3,3,3,3,4),(-1.53373699248731,
-1.4821365546276,-1.42770923574272,-1.37225914868662,-1.35730091972004,
-1.3456492103406,-1.2887137341168,-1.23163095606003,-1.1889477616213,-1.17417243892694,
-1.16116852269338,-1.14054366009933,-1.08259591133439,-1.02385609453003,
-0.965203361155031,-0.907403642265373,-0.890165400550202,-0.883312518347464,
-0.823389257062025,-0.768413556573938,-0.710270076125937,-0.651296044762335,
-0.618741054482267,-0.600604850453944,-0.581663798302628,-0.522138221798477,
-0.461815506006418,-0.400951391085016,-0.39085612252179,-0.330016377059625,
-0.310377881025886,-0.303327250694008,-0.241908819659544,-0.179747915445459,
-0.117618730811708,-0.0562544900865141,0.),.UNSPECIFIED.);
#564=B_SPLINE_CURVE_WITH_KNOTS('',3,(#71903,#71904,#71905,#71906,#71907,
#71908,#71909,#71910),.UNSPECIFIED.,.F.,.F.,(4,1,1,1,1,4),(74.4819856391522,
74.7118741291818,75.2107389412091,75.7096037532364,76.2084685652637,76.7073333772911),
 .UNSPECIFIED.);
#565=B_SPLINE_CURVE_WITH_KNOTS('',3,(#71913,#71914,#71915,#71916,#71917,
#71918,#71919,#71920,#71921),.UNSPECIFIED.,.F.,.F.,(4,1,1,1,1,1,4),(74.4820002615382,
74.7614958321197,75.260360644147,75.7592254561744,76.2580902682017,76.756955080229,
77.2307066486088),.UNSPECIFIED.);
#566=B_SPLINE_CURVE_WITH_KNOTS('',3,(#71927,#71928,#71929,#71930,#71931,
#71932,#71933,#71934,#71935,#71936,#71937,#71938,#71939,#71940,#71941,#71942,
#71943,#71944,#71945,#71946,#71947,#71948,#71949,#71950,#71951,#71952,#71953,
#71954,#71955,#71956,#71957,#71958,#71959,#71960,#71961,#71962,#71963,#71964,
#71965,#71966,#71967,#71968,#71969,#71970,#71971,#71972,#71973,#71974,#71975,
#71976,#71977,#71978,#71979,#71980,#71981,#71982,#71983,#71984,#71985,#71986,
#71987,#71988,#71989,#71990,#71991,#71992,#71993,#71994,#71995,#71996,#71997,
#71998,#71999,#72000,#72001,#72002,#72003,#72004,#72005,#72006,#72007,#72008,
#72009,#72010,#72011,#72012,#72013,#72014,#72015,#72016,#72017,#72018,#72019,
#72020,#72021,#72022,#72023,#72024,#72025,#72026,#72027,#72028,#72029,#72030,
#72031,#72032,#72033,#72034,#72035,#72036,#72037,#72038,#72039,#72040,#72041,
#72042,#72043,#72044,#72045,#72046,#72047,#72048,#72049,#72050,#72051,#72052,
#72053,#72054,#72055,#72056,#72057,#72058,#72059,#72060,#72061,#72062,#72063,
#72064,#72065,#72066,#72067,#72068,#72069,#72070,#72071,#72072,#72073,#72074,
#72075,#72076,#72077,#72078,#72079,#72080,#72081,#72082,#72083,#72084,#72085,
#72086,#72087,#72088,#72089,#72090,#72091,#72092,#72093,#72094,#72095,#72096,
#72097,#72098,#72099,#72100,#72101),.UNSPECIFIED.,.F.,.F.,(4,3,3,3,3,3,
3,3,3,3,3,3,3,3,3,3,3,3,3,3,3,3,3,3,3,3,3,3,3,3,3,3,3,3,3,3,3,3,3,3,3,3,
3,3,3,3,3,3,3,3,3,3,3,3,3,3,3,3,4),(68.1987975186712,68.2266315728265,68.3041236122402,
68.3816013676368,68.4590704189412,68.5365456775087,68.6140206493277,68.6915121862316,
68.7254963848538,68.8029883992075,68.8804661294451,68.9579351555709,69.0354103891201,
69.1128853360578,69.1903768484489,69.2243611968811,69.3018532647296,69.3793310486332,
69.456800128424,69.5342754152362,69.6117504151087,69.6892419796001,69.7232260089085,
69.800717988916,69.8781956847726,69.9556646765945,70.0331398762059,70.1106147894785,
70.1881062688295,70.2220908209358,70.2995828974163,70.3770606897927,70.4545297778736,
70.5320050726442,70.6094800802699,70.6869716521594,70.7209556329631,70.7984477160451,
70.8759255156548,70.9533946115695,71.0308699150024,71.1083449317504,71.1858365133831,
71.2198204449904,71.2973121319933,71.3747895331616,71.4522582295674,71.5297331348839,
71.6072077550478,71.684698944971,71.7186852570178,71.7961782868195,71.8736570365031,
71.9511270827911,72.0286033299696,72.1060792849236,72.1835717903897,72.2175500690451,
72.2566310325652),.UNSPECIFIED.);
#567=B_SPLINE_CURVE_WITH_KNOTS('',3,(#72102,#72103,#72104,#72105,#72106,
#72107,#72108,#72109),.UNSPECIFIED.,.F.,.F.,(4,1,1,1,1,4),(72.2566310687215,
72.7164148810724,73.2152796930998,73.7141445051271,74.2130093171544,74.4819856391522),
 .UNSPECIFIED.);
#568=B_SPLINE_CURVE_WITH_KNOTS('',3,(#72111,#72112,#72113,#72114,#72115,
#72116,#72117,#72118,#72119),.UNSPECIFIED.,.F.,.F.,(4,1,1,1,1,1,4),(72.2566310325652,
72.2671717719831,72.7660365840104,73.2649013960377,73.7637662080651,74.2626310200924,
74.4820002615382),.UNSPECIFIED.);
#569=B_SPLINE_CURVE_WITH_KNOTS('',3,(#72120,#72121,#72122,#72123,#72124,
#72125,#72126,#72127,#72128,#72129,#72130,#72131,#72132,#72133,#72134,#72135,
#72136,#72137,#72138,#72139,#72140,#72141,#72142,#72143,#72144,#72145,#72146,
#72147,#72148,#72149,#72150,#72151,#72152,#72153,#72154,#72155,#72156,#72157,
#72158,#72159,#72160,#72161,#72162,#72163,#72164,#72165,#72166,#72167,#72168,
#72169,#72170,#72171,#72172,#72173,#72174,#72175,#72176,#72177,#72178,#72179,
#72180,#72181,#72182,#72183,#72184,#72185,#72186,#72187,#72188,#72189,#72190,
#72191,#72192,#72193,#72194,#72195,#72196,#72197,#72198,#72199,#72200,#72201,
#72202,#72203,#72204,#72205,#72206,#72207,#72208,#72209,#72210,#72211,#72212,
#72213,#72214,#72215,#72216,#72217,#72218,#72219,#72220,#72221,#72222,#72223,
#72224,#72225,#72226,#72227,#72228,#72229,#72230,#72231,#72232,#72233,#72234,
#72235,#72236,#72237,#72238,#72239,#72240,#72241,#72242,#72243,#72244,#72245,
#72246,#72247,#72248,#72249,#72250,#72251,#72252,#72253,#72254,#72255,#72256,
#72257,#72258,#72259,#72260,#72261,#72262,#72263,#72264,#72265,#72266,#72267,
#72268,#72269,#72270,#72271,#72272,#72273,#72274,#72275,#72276,#72277,#72278,
#72279,#72280,#72281,#72282,#72283,#72284,#72285,#72286,#72287,#72288,#72289,
#72290,#72291),.UNSPECIFIED.,.F.,.F.,(4,3,3,3,3,3,3,3,3,3,3,3,3,3,3,3,3,
3,3,3,3,3,3,3,3,3,3,3,3,3,3,3,3,3,3,3,3,3,3,3,3,3,3,3,3,3,3,3,3,3,3,3,3,
3,3,3,3,4),(68.1987898047183,68.2762532757644,68.3537453085195,68.4312230572261,
68.5086921018308,68.586167353733,68.6636423189185,68.7411338492811,68.7751180877918,
68.8526101196304,68.9300878674179,69.0075569111027,69.0850321620932,69.1625071263726,
69.2399986558434,69.2739828998191,69.3514749330283,69.4289526821889,69.5064217272455,
69.5838969795948,69.6613719452233,69.7388634760199,69.7728477118464,69.8503397438658,
69.9278174918377,70.0052865357114,70.0827617868932,70.1602367513658,70.2377282810308,
70.2717125238738,70.3492045547049,70.4266823014742,70.5041513441335,70.5816265940954,
70.6591015573465,70.736593085796,70.7705773359011,70.8480693754309,70.9255471309442,
71.0030161823662,71.0804914410497,71.1579664129848,71.2354579500022,71.2694421479284,
71.3469341620217,71.4244118919975,71.5018809178624,71.5793561511515,71.6568310978316,
71.7343226099682,71.7683069599557,71.8457247371354,71.9231279927475,72.0005225461464,
72.077923117042,72.15532396466,72.2327409413495,72.2566310325652),
 .UNSPECIFIED.);
#570=B_SPLINE_CURVE_WITH_KNOTS('',3,(#72297,#72298,#72299,#72300,#72301,
#72302,#72303,#72304,#72305,#72306,#72307,#72308),.UNSPECIFIED.,.F.,.F.,
(4,1,1,1,1,1,1,1,1,4),(61.9156408615241,62.2402538284985,62.7391186405258,
63.2379834525532,63.7368482645805,64.2357130766078,64.7345778886352,65.2334427006625,
65.7323075126898,65.9734457190118),.UNSPECIFIED.);
#571=B_SPLINE_CURVE_WITH_KNOTS('',3,(#72309,#72310,#72311,#72312,#72313,
#72314,#72315,#72316,#72317,#72318,#72319,#72320,#72321,#72322,#72323,#72324,
#72325,#72326,#72327,#72328,#72329,#72330,#72331,#72332,#72333,#72334,#72335,
#72336,#72337,#72338,#72339,#72340,#72341,#72342,#72343,#72344,#72345,#72346,
#72347,#72348,#72349,#72350,#72351,#72352,#72353,#72354,#72355,#72356,#72357,
#72358,#72359,#72360,#72361,#72362,#72363,#72364,#72365,#72366,#72367,#72368,
#72369,#72370,#72371,#72372,#72373,#72374,#72375,#72376,#72377,#72378,#72379,
#72380,#72381,#72382,#72383,#72384,#72385,#72386,#72387,#72388,#72389,#72390,
#72391,#72392,#72393,#72394,#72395,#72396,#72397,#72398,#72399,#72400,#72401,
#72402),.UNSPECIFIED.,.F.,.F.,(4,3,3,3,3,3,3,3,3,3,3,3,3,3,3,3,3,3,3,3,
3,3,3,3,3,3,3,3,3,3,3,4),(65.9734457253856,66.051752866185,66.1300656952307,
66.2083969560539,66.2311723247172,66.3086643565655,66.3861421043627,66.4636111480579,
66.5410863990578,66.6185613633469,66.6960528928273,66.7300371367445,66.8075291699426,
66.8850069190923,66.9624759641383,67.0399512164768,67.1174261820946,67.1949177128806,
67.2289019487718,67.3063939807927,67.3838717287663,67.4613407726409,67.5388160238239,
67.6162909882975,67.6937825179636,67.7277667607991,67.8052584948873,67.8827358464432,
67.9617512645002,68.0392239583848,68.119010738528,68.1987975186712),
 .UNSPECIFIED.);
#572=B_SPLINE_CURVE_WITH_KNOTS('',3,(#72404,#72405,#72406,#72407,#72408,
#72409,#72410,#72411,#72412,#72413,#72414,#72415,#72416,#72417,#72418,#72419,
#72420,#72421,#72422,#72423,#72424,#72425,#72426,#72427,#72428,#72429,#72430,
#72431,#72432,#72433,#72434,#72435,#72436,#72437,#72438,#72439,#72440,#72441,
#72442,#72443,#72444,#72445,#72446,#72447,#72448,#72449,#72450,#72451,#72452,
#72453,#72454,#72455,#72456,#72457,#72458,#72459,#72460,#72461,#72462,#72463,
#72464,#72465,#72466,#72467,#72468,#72469,#72470,#72471,#72472,#72473,#72474,
#72475,#72476,#72477,#72478,#72479,#72480,#72481,#72482,#72483,#72484,#72485,
#72486,#72487,#72488,#72489,#72490,#72491,#72492,#72493,#72494,#72495,#72496,
#72497),.UNSPECIFIED.,.F.,.F.,(4,3,3,3,3,3,3,3,3,3,3,3,3,3,3,3,3,3,3,3,
3,3,3,3,3,3,3,3,3,3,3,4),(65.9734457253856,66.05113864352,66.1288303647685,
66.2065431816206,66.2807940276551,66.3582860600736,66.4357638084426,66.5132328527091,
66.5907081042758,66.6681830691279,66.7456745991621,66.7796588396825,66.8571508721125,
66.934628620493,67.0120976647703,67.0895729163482,67.1670478812115,67.2445394112565,
67.2785236517098,67.3560156841782,67.433493432597,67.5109624769137,67.5884377285306,
67.6659126934328,67.7434042235161,67.7773884637371,67.8548798500932,67.9323566782865,
68.0098309919021,68.0873000058441,68.1647781672896,68.1987898047183),
 .UNSPECIFIED.);
#573=B_SPLINE_CURVE_WITH_KNOTS('',3,(#72498,#72499,#72500,#72501,#72502,
#72503,#72504,#72505,#72506,#72507,#72508,#72509),.UNSPECIFIED.,.F.,.F.,
(4,1,1,1,1,1,1,1,1,4),(61.9156464171414,62.2898755314365,62.7887403434638,
63.2876051554911,63.7864699675185,64.2853347795458,64.7841995915731,65.2830644036005,
65.7819292156278,65.9734456898724),.UNSPECIFIED.);
#574=B_SPLINE_CURVE_WITH_KNOTS('',3,(#72515,#72516,#72517,#72518,#72519,
#72520,#72521,#72522,#72523,#72524,#72525,#72526,#72527,#72528,#72529,#72530,
#72531,#72532,#72533,#72534,#72535,#72536,#72537,#72538,#72539,#72540,#72541,
#72542,#72543,#72544,#72545,#72546,#72547,#72548,#72549,#72550,#72551,#72552,
#72553,#72554,#72555,#72556,#72557,#72558,#72559,#72560,#72561,#72562,#72563,
#72564,#72565,#72566,#72567,#72568,#72569,#72570,#72571,#72572,#72573,#72574,
#72575,#72576,#72577,#72578,#72579,#72580,#72581,#72582,#72583,#72584,#72585,
#72586,#72587,#72588,#72589,#72590,#72591,#72592,#72593,#72594,#72595,#72596,
#72597,#72598,#72599,#72600,#72601,#72602,#72603,#72604,#72605,#72606,#72607,
#72608,#72609,#72610,#72611,#72612,#72613,#72614,#72615,#72616,#72617,#72618,
#72619,#72620,#72621,#72622,#72623,#72624,#72625,#72626,#72627,#72628,#72629,
#72630,#72631,#72632,#72633,#72634,#72635,#72636,#72637,#72638,#72639,#72640,
#72641,#72642,#72643,#72644,#72645,#72646,#72647,#72648,#72649,#72650,#72651,
#72652,#72653,#72654,#72655,#72656,#72657,#72658,#72659,#72660,#72661,#72662,
#72663,#72664,#72665,#72666,#72667,#72668,#72669,#72670,#72671,#72672,#72673,
#72674,#72675,#72676,#72677,#72678,#72679,#72680,#72681,#72682,#72683,#72684,
#72685,#72686),.UNSPECIFIED.,.F.,.F.,(4,3,3,3,3,3,3,3,3,3,3,3,3,3,3,3,3,
3,3,3,3,3,3,3,3,3,3,3,3,3,3,3,3,3,3,3,3,3,3,3,3,3,3,3,3,3,3,3,3,3,3,3,3,
3,3,3,3,4),(55.6324185145553,55.7099104487287,55.7550112721432,55.8325033045725,
55.9099810529522,55.9874500972293,56.0649253488068,56.1424003136698,56.2198918437144,
56.2538760841706,56.3313681165998,56.4088458649798,56.4863149092575,56.5637901608348,
56.6412651256974,56.718756655742,56.7527408961979,56.830232928627,56.9077106770066,
56.985179721284,57.0626549728614,57.1401299377238,57.2176214677687,57.2516057082252,
57.3290977406545,57.4065754890343,57.484044533311,57.5615197848885,57.6389947497512,
57.7164862797957,57.7504705202526,57.8279625526819,57.9054403010617,57.9829093453387,
58.0603845969162,58.1378595617786,58.2153510918235,58.2493353322799,58.3268273647091,
58.404305113089,58.4817741573666,58.5592494089439,58.6367243738066,58.7142159038511,
58.7482001443072,58.8256921767366,58.9031699251163,58.9806389693927,59.05811422097,
59.1355891858328,59.2130807158776,59.2470649563345,59.3242792098715,59.4014782880975,
59.4786774007806,59.5558721176712,59.6330828530534,59.6902604182061),
 .UNSPECIFIED.);
#575=B_SPLINE_CURVE_WITH_KNOTS('',3,(#72687,#72688,#72689,#72690,#72691,
#72692,#72693,#72694,#72695),.UNSPECIFIED.,.F.,.F.,(4,1,1,1,1,1,4),(59.6902604182061,
59.7459297683619,60.2447945803892,60.7436593924165,61.2425242044439,61.7413890164712,
61.9156408615241),.UNSPECIFIED.);
#576=B_SPLINE_CURVE_WITH_KNOTS('',3,(#72697,#72698,#72699,#72700,#72701,
#72702,#72703,#72704,#72705),.UNSPECIFIED.,.F.,.F.,(4,1,1,1,1,1,4),(59.6902604182061,
59.7955514712998,60.2944162833272,60.7932810953545,61.2921459073818,61.7910107194092,
61.9156464171414),.UNSPECIFIED.);
#577=B_SPLINE_CURVE_WITH_KNOTS('',3,(#72706,#72707,#72708,#72709,#72710,
#72711,#72712,#72713,#72714,#72715,#72716,#72717,#72718,#72719,#72720,#72721,
#72722,#72723,#72724,#72725,#72726,#72727,#72728,#72729,#72730,#72731,#72732,
#72733,#72734,#72735,#72736,#72737,#72738,#72739,#72740,#72741,#72742,#72743,
#72744,#72745,#72746,#72747,#72748,#72749,#72750,#72751,#72752,#72753,#72754,
#72755,#72756,#72757,#72758,#72759,#72760,#72761,#72762,#72763,#72764,#72765,
#72766,#72767,#72768,#72769,#72770,#72771,#72772,#72773,#72774,#72775,#72776,
#72777,#72778,#72779,#72780,#72781,#72782,#72783,#72784,#72785,#72786,#72787,
#72788,#72789,#72790,#72791,#72792,#72793,#72794,#72795,#72796,#72797,#72798,
#72799,#72800,#72801,#72802,#72803,#72804,#72805,#72806,#72807,#72808,#72809,
#72810,#72811,#72812,#72813,#72814,#72815,#72816,#72817,#72818,#72819,#72820,
#72821,#72822,#72823,#72824,#72825,#72826,#72827,#72828,#72829,#72830,#72831,
#72832,#72833,#72834,#72835,#72836,#72837,#72838,#72839,#72840,#72841,#72842,
#72843,#72844,#72845,#72846,#72847,#72848,#72849,#72850,#72851,#72852,#72853,
#72854,#72855,#72856,#72857,#72858,#72859,#72860,#72861,#72862,#72863,#72864,
#72865,#72866,#72867,#72868,#72869,#72870,#72871,#72872,#72873,#72874,#72875,
#72876,#72877),.UNSPECIFIED.,.F.,.F.,(4,3,3,3,3,3,3,3,3,3,3,3,3,3,3,3,3,
3,3,3,3,3,3,3,3,3,3,3,3,3,3,3,3,3,3,3,3,3,3,3,3,3,3,3,3,3,3,3,3,3,3,3,3,
3,3,3,3,4),(55.6324228066038,55.7098984440576,55.787389714901,55.8046329750812,
55.8821250075104,55.9596027558903,56.0370718001674,56.1145470517449,56.1920220166075,
56.2695135466522,56.3034977871085,56.3809898195378,56.4584675679174,56.5359366121958,
56.6134118637733,56.6908868286361,56.7683783586809,56.8023625991359,56.879854631565,
56.9573323799445,57.0348014242223,57.1122766757997,57.1897516406624,57.2672431707073,
57.3012274111632,57.3787194435924,57.4561971919722,57.5336662362496,57.611141487827,
57.6886164526896,57.7661079827342,57.8000922231905,57.8775842556198,57.9550620039998,
58.0325310482768,58.1100062998543,58.1874812647173,58.2649727947617,58.2989570352179,
58.3764490676469,58.4539268160264,58.5313958603032,58.6088711118807,58.6863460767432,
58.7638376067878,58.7978218472452,58.8753138796745,58.952791628054,59.0302606723321,
59.1077359239092,59.1852108887716,59.262702418816,59.2966866592725,59.3738879299902,
59.4529810520442,59.5301632256214,59.6102118219137,59.6902604182061),
 .UNSPECIFIED.);
#578=B_SPLINE_CURVE_WITH_KNOTS('',3,(#72883,#72884,#72885,#72886,#72887,
#72888,#72889,#72890,#72891,#72892,#72893,#72894,#72895,#72896,#72897,#72898,
#72899,#72900,#72901,#72902,#72903,#72904,#72905,#72906,#72907,#72908,#72909,
#72910,#72911,#72912,#72913,#72914,#72915,#72916,#72917,#72918,#72919,#72920,
#72921,#72922,#72923,#72924,#72925,#72926,#72927,#72928,#72929,#72930,#72931,
#72932,#72933,#72934,#72935,#72936,#72937,#72938,#72939,#72940,#72941,#72942,
#72943,#72944,#72945,#72946,#72947,#72948,#72949,#72950,#72951,#72952,#72953,
#72954,#72955,#72956,#72957,#72958,#72959,#72960,#72961,#72962,#72963,#72964,
#72965,#72966,#72967,#72968,#72969,#72970,#72971,#72972,#72973,#72974,#72975,
#72976,#72977,#72978,#72979,#72980,#72981,#72982,#72983,#72984,#72985,#72986,
#72987,#72988,#72989,#72990,#72991,#72992,#72993,#72994,#72995,#72996,#72997,
#72998,#72999,#73000,#73001,#73002,#73003,#73004,#73005,#73006,#73007,#73008,
#73009,#73010,#73011,#73012,#73013,#73014,#73015,#73016,#73017,#73018,#73019,
#73020,#73021,#73022,#73023,#73024,#73025,#73026,#73027,#73028,#73029,#73030,
#73031,#73032,#73033,#73034,#73035,#73036,#73037,#73038,#73039,#73040,#73041,
#73042,#73043,#73044,#73045,#73046,#73047,#73048,#73049,#73050,#73051,#73052,
#73053,#73054),.UNSPECIFIED.,.F.,.F.,(4,3,3,3,3,3,3,3,3,3,3,3,3,3,3,3,3,
3,3,3,3,3,3,3,3,3,3,3,3,3,3,3,3,3,3,3,3,3,3,3,3,3,3,3,3,3,3,3,3,3,3,3,3,
3,3,3,3,4),(49.3492660090855,49.4267434618947,49.5042123549391,49.5816875286347,
49.6591625602837,49.7366540371569,49.7686335278153,49.8461255602445,49.9236033086243,
50.0010723529015,50.078547604479,50.1560225693416,50.2335140993863,50.2674983398426,
50.3449903722719,50.4224681206516,50.4999371649288,50.5774124165063,50.654887381369,
50.7323789114136,50.76636315187,50.8438551842993,50.921332932679,50.9988019769563,
51.0762772285338,51.1537521933964,51.2312437234411,51.2652279638973,51.3427199963265,
51.4201977447062,51.4976667889834,51.5751420405608,51.6526170054234,51.730108535468,
51.7640927759246,51.8415848083539,51.9190625567337,51.9965316010112,52.0740068525886,
52.1514818174514,52.228973347496,52.2629575879519,52.3404496203811,52.4179273687608,
52.4953964130381,52.5728716646155,52.6503466294781,52.7278381595228,52.7618223999793,
52.8393144324086,52.9167921807885,52.9942612250656,53.0717364766431,53.1492114415058,
53.2267029715505,53.2606872120066,53.3414563463415,53.4070751109153),
 .UNSPECIFIED.);
#579=B_SPLINE_CURVE_WITH_KNOTS('',3,(#73055,#73056,#73057,#73058,#73059,
#73060,#73061,#73062,#73063,#73064,#73065,#73066,#73067,#73068,#73069,#73070,
#73071,#73072,#73073,#73074,#73075,#73076,#73077,#73078,#73079,#73080,#73081,
#73082,#73083,#73084,#73085,#73086,#73087,#73088,#73089,#73090,#73091,#73092,
#73093,#73094,#73095,#73096,#73097,#73098,#73099,#73100,#73101,#73102,#73103,
#73104,#73105,#73106,#73107,#73108,#73109,#73110,#73111,#73112,#73113,#73114,
#73115,#73116,#73117,#73118,#73119,#73120,#73121,#73122,#73123,#73124,#73125,
#73126,#73127,#73128,#73129,#73130,#73131,#73132,#73133,#73134,#73135,#73136,
#73137,#73138,#73139,#73140,#73141,#73142,#73143,#73144,#73145,#73146,#73147,
#73148),.UNSPECIFIED.,.F.,.F.,(4,3,3,3,3,3,3,3,3,3,3,3,3,3,3,3,3,3,3,3,
3,3,3,3,3,3,3,3,3,3,3,4),(53.4070751110265,53.4844112691831,53.5617528045003,
53.6390933869444,53.716451872362,53.7595520240339,53.8370440564632,53.9145218048428,
53.9919908491204,54.0694661006978,54.1469410655606,54.2244325956052,54.2584168360613,
54.3359088684906,54.4133866168704,54.4908556611472,54.5683309127246,54.6458058775878,
54.7232974076326,54.7572816480886,54.8347736805178,54.9122514288974,54.9897204731745,
55.0671957247518,55.1446706896146,55.2221622196592,55.2561464601159,55.3336377293316,
55.4111196629735,55.4885910423118,55.5660683959404,55.6324185145553),
 .UNSPECIFIED.);
#580=B_SPLINE_CURVE_WITH_KNOTS('',3,(#73150,#73151,#73152,#73153,#73154,
#73155,#73156,#73157,#73158,#73159,#73160,#73161,#73162,#73163,#73164,#73165,
#73166,#73167,#73168,#73169,#73170,#73171,#73172,#73173,#73174,#73175,#73176,
#73177,#73178,#73179,#73180,#73181,#73182,#73183,#73184,#73185,#73186,#73187,
#73188,#73189,#73190,#73191,#73192,#73193,#73194,#73195,#73196,#73197,#73198,
#73199,#73200,#73201,#73202,#73203,#73204,#73205,#73206,#73207,#73208,#73209,
#73210,#73211,#73212,#73213,#73214,#73215,#73216,#73217,#73218,#73219,#73220,
#73221,#73222,#73223,#73224,#73225,#73226,#73227,#73228,#73229,#73230,#73231,
#73232,#73233,#73234,#73235,#73236,#73237,#73238,#73239,#73240,#73241,#73242,
#73243,#73244,#73245,#73246),.UNSPECIFIED.,.F.,.F.,(4,3,3,3,3,3,3,3,3,3,
3,3,3,3,3,3,3,3,3,3,3,3,3,3,3,3,3,3,3,3,3,3,4),(53.4070751110912,53.4842508434172,
53.5614165780464,53.638587389558,53.7157587866332,53.7929466274777,53.8091737269719,
53.8866657594011,53.9641435077811,54.0416125520584,54.119087803636,54.1965627684987,
54.2740542985434,54.3080385389992,54.3855305714285,54.4630083198084,54.5404773640861,
54.6179526156636,54.6954275805259,54.7729191105704,54.8069033510266,54.884395383456,
54.9618731318356,55.0393421761127,55.1168174276899,55.1942923925525,55.2717839225971,
55.3057681630539,55.3832595234145,55.4607387422742,55.5382077764871,55.6156767556165,
55.6324228066038),.UNSPECIFIED.);
#581=B_SPLINE_CURVE_WITH_KNOTS('',3,(#73247,#73248,#73249,#73250,#73251,
#73252,#73253,#73254,#73255,#73256,#73257,#73258,#73259,#73260,#73261,#73262,
#73263,#73264,#73265,#73266,#73267,#73268,#73269,#73270,#73271,#73272,#73273,
#73274,#73275,#73276,#73277,#73278,#73279,#73280,#73281,#73282,#73283,#73284,
#73285,#73286,#73287,#73288,#73289,#73290,#73291,#73292,#73293,#73294,#73295,
#73296,#73297,#73298,#73299,#73300,#73301,#73302,#73303,#73304,#73305,#73306,
#73307,#73308,#73309,#73310,#73311,#73312,#73313,#73314,#73315,#73316,#73317,
#73318,#73319,#73320,#73321,#73322,#73323,#73324,#73325,#73326,#73327,#73328,
#73329,#73330,#73331,#73332,#73333,#73334,#73335,#73336,#73337,#73338,#73339,
#73340,#73341,#73342,#73343,#73344,#73345,#73346,#73347,#73348,#73349,#73350,
#73351,#73352,#73353,#73354,#73355,#73356,#73357,#73358,#73359,#73360,#73361,
#73362,#73363,#73364,#73365,#73366,#73367,#73368,#73369,#73370,#73371,#73372,
#73373,#73374,#73375,#73376,#73377,#73378,#73379,#73380,#73381,#73382,#73383,
#73384,#73385,#73386,#73387,#73388,#73389,#73390,#73391,#73392,#73393,#73394,
#73395,#73396,#73397,#73398,#73399,#73400,#73401,#73402,#73403,#73404,#73405,
#73406,#73407,#73408,#73409,#73410,#73411,#73412,#73413,#73414,#73415,#73416,
#73417,#73418),.UNSPECIFIED.,.F.,.F.,(4,3,3,3,3,3,3,3,3,3,3,3,3,3,3,3,3,
3,3,3,3,3,3,3,3,3,3,3,3,3,3,3,3,3,3,3,3,3,3,3,3,3,3,3,3,3,3,3,3,3,3,3,3,
3,3,3,3,4),(49.3492586328116,49.4267444987807,49.5042182319584,49.5827274816571,
49.6602019486695,49.7392285897114,49.8182552307533,49.8957472631825,49.9732250115623,
50.0506940558395,50.128169307417,50.2056442722796,50.2831358023243,50.3171200427806,
50.3946120752099,50.4720898235896,50.5495588678669,50.6270341194443,50.704509084307,
50.7820006143517,50.8159848548079,50.8934768872372,50.970954635617,51.0484236798943,
51.1258989314718,51.2033738963344,51.2808654263791,51.3148496668353,51.3923416992646,
51.4698194476443,51.5472884919217,51.6247637434991,51.7022387083619,51.7797302384065,
51.8137144788626,51.8912065112918,51.9686842596716,52.0461533039487,52.1236285555262,
52.2011035203887,52.2785950504333,52.3125792908899,52.3900713233191,52.467549071699,
52.5450181159764,52.6224933675538,52.6999683324166,52.7774598624612,52.8114441029172,
52.8889361353464,52.966413883726,53.043882928003,53.1213581795804,53.198833144443,
53.2763246744876,53.3103089149446,53.3927667121797,53.4070751110265),
 .UNSPECIFIED.);
#582=B_SPLINE_CURVE_WITH_KNOTS('',3,(#73424,#73425,#73426,#73427,#73428,
#73429,#73430,#73431,#73432,#73433,#73434,#73435,#73436,#73437,#73438,#73439,
#73440,#73441,#73442,#73443,#73444,#73445,#73446,#73447,#73448,#73449,#73450,
#73451,#73452,#73453,#73454,#73455,#73456,#73457,#73458,#73459,#73460,#73461,
#73462,#73463,#73464,#73465,#73466,#73467,#73468,#73469,#73470,#73471,#73472,
#73473,#73474,#73475,#73476,#73477,#73478,#73479,#73480,#73481,#73482,#73483,
#73484,#73485,#73486,#73487,#73488,#73489,#73490,#73491,#73492,#73493,#73494,
#73495,#73496,#73497,#73498,#73499,#73500,#73501,#73502,#73503,#73504,#73505,
#73506,#73507,#73508,#73509,#73510,#73511,#73512,#73513,#73514,#73515,#73516,
#73517,#73518,#73519,#73520,#73521,#73522,#73523,#73524,#73525,#73526,#73527,
#73528,#73529,#73530,#73531,#73532,#73533,#73534,#73535,#73536,#73537,#73538,
#73539,#73540,#73541,#73542,#73543,#73544,#73545,#73546,#73547,#73548,#73549,
#73550,#73551,#73552,#73553,#73554,#73555,#73556,#73557,#73558,#73559,#73560,
#73561,#73562,#73563,#73564,#73565,#73566,#73567,#73568,#73569,#73570,#73571,
#73572,#73573,#73574,#73575,#73576,#73577,#73578,#73579,#73580,#73581,#73582,
#73583,#73584,#73585,#73586,#73587,#73588,#73589,#73590,#73591,#73592,#73593,
#73594,#73595),.UNSPECIFIED.,.F.,.F.,(4,3,3,3,3,3,3,3,3,3,3,3,3,3,3,3,3,
3,3,3,3,3,3,3,3,3,3,3,3,3,3,3,3,3,3,3,3,3,3,3,3,3,3,3,3,3,3,3,3,3,3,3,3,
3,3,3,3,4),(43.066058970899,43.1435333918981,43.2210263208101,43.28339097146,
43.3608830038894,43.4383607522689,43.5158297965461,43.5933050481236,43.6707800129862,
43.7482715430309,43.7822557834873,43.8597478159166,43.9372255642961,44.0146946085731,
44.0921698601506,44.1696448250135,44.247136355058,44.2811205955147,44.3586126279439,
44.4360903763234,44.5135594206003,44.5910346721779,44.6685096370401,44.7460011670846,
44.779985407542,44.8574774399711,44.934955188351,45.0124242326282,45.0898994842056,
45.1673744490675,45.2448659791124,45.2788502195693,45.3563422519987,45.4338200003786,
45.5112890446562,45.5887642962336,45.6662392610963,45.7437307911408,45.7777150315967,
45.8552070640259,45.9326848124057,46.010153856683,46.08762910826,46.1651040731226,
46.2425956031668,46.276579843624,46.354071876053,46.4315496244331,46.5090186687113,
46.5864939202887,46.6639688851504,46.7414604151948,46.7754446556513,46.8528264263137,
46.9301963796882,47.0075557276487,47.0849176157589,47.1238898038469),
 .UNSPECIFIED.);
#583=B_SPLINE_CURVE_WITH_KNOTS('',3,(#73596,#73597,#73598,#73599,#73600,
#73601,#73602,#73603,#73604,#73605,#73606,#73607,#73608,#73609,#73610,#73611,
#73612,#73613,#73614,#73615,#73616,#73617,#73618,#73619,#73620,#73621,#73622,
#73623,#73624,#73625,#73626,#73627,#73628,#73629,#73630,#73631,#73632,#73633,
#73634,#73635,#73636,#73637,#73638,#73639,#73640,#73641,#73642,#73643,#73644,
#73645,#73646,#73647,#73648,#73649,#73650,#73651,#73652,#73653,#73654,#73655,
#73656,#73657,#73658,#73659,#73660,#73661,#73662,#73663,#73664,#73665,#73666,
#73667,#73668,#73669,#73670,#73671,#73672,#73673,#73674,#73675,#73676,#73677,
#73678,#73679,#73680,#73681,#73682,#73683,#73684,#73685,#73686,#73687,#73688,
#73689),.UNSPECIFIED.,.F.,.F.,(4,3,3,3,3,3,3,3,3,3,3,3,3,3,3,3,3,3,3,3,
3,3,3,3,3,3,3,3,3,3,3,4),(47.1238898039682,47.2045406527714,47.2743094676786,
47.3518015001079,47.4292792484876,47.5067482927648,47.5842235443423,47.661698509205,
47.7391900392496,47.773174279706,47.8506663121353,47.928144060515,48.005613104792,
48.0830883563694,48.1605633212322,48.2380548512768,48.2720390917333,48.3495311241625,
48.4270088725422,48.5044779168194,48.5819531683968,48.6594281332595,48.7369196633042,
48.7709039037606,48.8483959361898,48.9258736845696,49.0033427288469,49.0808179804244,
49.158292945287,49.2357844753317,49.269768715788,49.3492660090855),
 .UNSPECIFIED.);
#584=B_SPLINE_CURVE_WITH_KNOTS('',3,(#73691,#73692,#73693,#73694,#73695,
#73696,#73697,#73698,#73699,#73700,#73701,#73702,#73703,#73704,#73705,#73706,
#73707,#73708,#73709,#73710,#73711,#73712,#73713,#73714,#73715,#73716,#73717,
#73718,#73719,#73720,#73721,#73722,#73723,#73724,#73725,#73726,#73727,#73728,
#73729,#73730,#73731,#73732,#73733,#73734,#73735,#73736,#73737,#73738,#73739,
#73740,#73741,#73742,#73743,#73744,#73745,#73746,#73747,#73748,#73749,#73750,
#73751,#73752,#73753,#73754,#73755,#73756,#73757,#73758,#73759,#73760,#73761,
#73762,#73763,#73764,#73765,#73766,#73767,#73768,#73769,#73770,#73771,#73772,
#73773,#73774,#73775,#73776,#73777,#73778,#73779,#73780,#73781,#73782,#73783,
#73784,#73785,#73786,#73787),.UNSPECIFIED.,.F.,.F.,(4,3,3,3,3,3,3,3,3,3,
3,3,3,3,3,3,3,3,3,3,3,3,3,3,3,3,3,3,3,3,3,3,4),(47.1238898039176,47.2032584038848,
47.2826529753093,47.3239311706166,47.4014232030459,47.4789009514257,47.5563699957031,
47.6338452472805,47.7113202121431,47.7888117421879,47.8227959826439,47.9002880150732,
47.9777657634529,48.05523480773,48.1327100593075,48.2101850241701,48.2876765542147,
48.3216607946713,48.3991528271006,48.4766305754802,48.5540996197574,48.6315748713349,
48.7090498361976,48.7865413662423,48.8205256066986,48.8980176391279,48.9754953875076,
49.0529644317848,49.1304396833623,49.207914648225,49.2854061782696,49.3193904187259,
49.3492586328116),.UNSPECIFIED.);
#585=B_SPLINE_CURVE_WITH_KNOTS('',3,(#73788,#73789,#73790,#73791,#73792,
#73793,#73794,#73795,#73796,#73797,#73798,#73799,#73800,#73801,#73802,#73803,
#73804,#73805,#73806,#73807,#73808,#73809,#73810,#73811,#73812,#73813,#73814,
#73815,#73816,#73817,#73818,#73819,#73820,#73821,#73822,#73823,#73824,#73825,
#73826,#73827,#73828,#73829,#73830,#73831,#73832,#73833,#73834,#73835,#73836,
#73837,#73838,#73839,#73840,#73841,#73842,#73843,#73844,#73845,#73846,#73847,
#73848,#73849,#73850,#73851,#73852,#73853,#73854,#73855,#73856,#73857,#73858,
#73859,#73860,#73861,#73862,#73863,#73864,#73865,#73866,#73867,#73868,#73869,
#73870,#73871,#73872,#73873,#73874,#73875,#73876,#73877,#73878,#73879,#73880,
#73881,#73882,#73883,#73884,#73885,#73886,#73887,#73888,#73889,#73890,#73891,
#73892,#73893,#73894,#73895,#73896,#73897,#73898,#73899,#73900,#73901,#73902,
#73903,#73904,#73905,#73906,#73907,#73908,#73909,#73910,#73911,#73912,#73913,
#73914,#73915,#73916,#73917,#73918,#73919,#73920,#73921,#73922,#73923,#73924,
#73925,#73926,#73927,#73928,#73929,#73930,#73931,#73932,#73933,#73934,#73935,
#73936,#73937,#73938,#73939,#73940,#73941,#73942,#73943,#73944,#73945,#73946,
#73947,#73948,#73949,#73950,#73951,#73952,#73953,#73954,#73955,#73956,#73957,
#73958,#73959),.UNSPECIFIED.,.F.,.F.,(4,3,3,3,3,3,3,3,3,3,3,3,3,3,3,3,3,
3,3,3,3,3,3,3,3,3,3,3,3,3,3,3,3,3,3,3,3,3,3,3,3,3,3,3,3,3,3,3,3,3,3,3,3,
3,3,3,3,4),(43.0660676533433,43.143542925694,43.2210178738762,43.2985094186679,
43.333012674398,43.4105047068272,43.4879824552068,43.5654514994841,43.6429267510615,
43.720401715924,43.7978932459686,43.8318774864253,43.9093695188546,43.9868472672343,
44.0643163115116,44.1417915630891,44.2192665279518,44.2967580579965,44.3307422984526,
44.4082343308818,44.4857120792616,44.5631811235388,44.6406563751163,44.718131339979,
44.7956228700236,44.82960711048,44.9070991429092,44.984576891289,45.0620459355663,
45.1395211871438,45.2169961520065,45.2944876820511,45.3284719225073,45.4059639549365,
45.4834417033163,45.5609107475936,45.6383859991711,45.7158609640337,45.7933524940783,
45.8273367345346,45.9048287669638,45.9823065153436,46.0597755596211,46.1372508111986,
46.2147257760612,46.2922173061059,46.326201546562,46.4036935789912,46.481171327371,
46.5586403716484,46.6361156232258,46.7135905880888,46.7910821181334,46.8250663585893,
46.9028676038855,46.9806524488782,47.058431481866,47.1238898038469),
 .UNSPECIFIED.);
#586=B_SPLINE_CURVE_WITH_KNOTS('',3,(#73965,#73966,#73967,#73968,#73969,
#73970,#73971,#73972,#73973,#73974,#73975,#73976,#73977),.UNSPECIFIED.,
 .F.,.F.,(4,1,1,1,1,1,1,1,1,1,4),(36.7828738679604,36.7981484151047,37.2970132271321,
37.7958780391594,38.2947428511867,38.793607663214,39.2924724752414,39.7913372872687,
40.290202099296,40.7890669113234,40.8407044966673),.UNSPECIFIED.);
#587=B_SPLINE_CURVE_WITH_KNOTS('',3,(#73978,#73979,#73980,#73981,#73982,
#73983,#73984,#73985,#73986,#73987,#73988,#73989,#73990,#73991,#73992,#73993,
#73994,#73995,#73996,#73997,#73998,#73999,#74000,#74001,#74002,#74003,#74004,
#74005,#74006,#74007,#74008,#74009,#74010,#74011,#74012,#74013,#74014,#74015,
#74016,#74017,#74018,#74019,#74020,#74021,#74022,#74023,#74024,#74025,#74026,
#74027,#74028,#74029,#74030,#74031,#74032,#74033,#74034,#74035,#74036,#74037,
#74038,#74039,#74040,#74041,#74042,#74043,#74044,#74045,#74046,#74047,#74048,
#74049,#74050,#74051,#74052,#74053,#74054,#74055,#74056,#74057,#74058,#74059,
#74060,#74061,#74062,#74063,#74064,#74065,#74066,#74067,#74068,#74069,#74070,
#74071),.UNSPECIFIED.,.F.,.F.,(4,3,3,3,3,3,3,3,3,3,3,3,3,3,3,3,3,3,3,3,
3,3,3,3,3,3,3,3,3,3,3,4),(40.8407044966673,40.9179251802868,40.995132453893,
41.0723426888697,41.149549938454,41.2267761550704,41.2879317233507,41.36542375578,
41.4429015041596,41.5203705484367,41.5978458000141,41.6753207648766,41.7528122949213,
41.786796535378,41.8642885678073,41.9417663161871,42.0192353604645,42.0967106120418,
42.1741855769045,42.2516771069493,42.2856613474054,42.3631533798346,42.4406311282143,
42.5181001724917,42.5955754240691,42.673050388932,42.7505419189767,42.7845261594327,
42.8620191530837,42.9394967034995,43.0169700726562,43.066058970899),
 .UNSPECIFIED.);
#588=B_SPLINE_CURVE_WITH_KNOTS('',3,(#74073,#74074,#74075,#74076,#74077,
#74078,#74079,#74080,#74081,#74082,#74083,#74084,#74085,#74086,#74087,#74088,
#74089,#74090,#74091,#74092,#74093,#74094,#74095,#74096,#74097,#74098,#74099,
#74100,#74101,#74102,#74103,#74104,#74105,#74106,#74107,#74108,#74109,#74110,
#74111,#74112,#74113,#74114,#74115,#74116,#74117,#74118,#74119,#74120,#74121,
#74122,#74123,#74124,#74125,#74126,#74127,#74128,#74129,#74130,#74131,#74132,
#74133,#74134,#74135,#74136,#74137,#74138,#74139,#74140,#74141,#74142,#74143,
#74144,#74145,#74146,#74147,#74148,#74149,#74150,#74151,#74152,#74153,#74154,
#74155,#74156,#74157,#74158,#74159,#74160,#74161,#74162,#74163,#74164,#74165,
#74166),.UNSPECIFIED.,.F.,.F.,(4,3,3,3,3,3,3,3,3,3,3,3,3,3,3,3,3,3,3,3,
3,3,3,3,3,3,3,3,3,3,3,4),(40.8407044966673,40.9181815167146,40.9956442072441,
41.073098197011,41.1505583692719,41.2280183712181,41.3054948721939,41.3375534262887,
41.415045458718,41.4925232070977,41.5699922513747,41.6474675029522,41.7249424678148,
41.8024339978594,41.836418238316,41.9139102707452,41.991388019125,42.0688570634023,
42.1463323149798,42.2238072798424,42.3012988098871,42.3352830503433,42.4127750827726,
42.4902528311523,42.5677218754295,42.6451971270069,42.7226720918697,42.8001636219143,
42.8341478623707,42.9116395331415,42.9891221306656,43.0660676533433),
 .UNSPECIFIED.);
#589=B_SPLINE_CURVE_WITH_KNOTS('',3,(#74167,#74168,#74169,#74170,#74171,
#74172,#74173,#74174,#74175,#74176,#74177,#74178,#74179,#74180,#74181,#74182,
#74183,#74184,#74185,#74186,#74187,#74188,#74189,#74190,#74191,#74192,#74193,
#74194,#74195,#74196,#74197,#74198,#74199,#74200,#74201,#74202,#74203,#74204,
#74205,#74206,#74207,#74208,#74209,#74210,#74211,#74212,#74213,#74214,#74215,
#74216,#74217,#74218,#74219,#74220,#74221,#74222,#74223,#74224,#74225,#74226,
#74227,#74228,#74229,#74230,#74231,#74232,#74233,#74234,#74235,#74236,#74237,
#74238,#74239,#74240,#74241,#74242,#74243,#74244,#74245,#74246,#74247,#74248,
#74249,#74250,#74251,#74252,#74253,#74254,#74255,#74256,#74257,#74258,#74259,
#74260,#74261,#74262,#74263,#74264,#74265,#74266,#74267,#74268,#74269,#74270,
#74271,#74272,#74273,#74274,#74275,#74276,#74277,#74278,#74279,#74280,#74281,
#74282,#74283,#74284,#74285,#74286,#74287,#74288,#74289,#74290,#74291,#74292,
#74293,#74294,#74295,#74296,#74297,#74298,#74299,#74300,#74301,#74302,#74303,
#74304,#74305,#74306,#74307,#74308,#74309,#74310,#74311,#74312,#74313,#74314,
#74315,#74316,#74317,#74318,#74319,#74320,#74321,#74322,#74323,#74324,#74325,
#74326,#74327,#74328,#74329,#74330,#74331,#74332,#74333,#74334,#74335,#74336,
#74337,#74338,#74339,#74340,#74341),.UNSPECIFIED.,.F.,.F.,(4,3,3,3,3,3,
3,3,3,3,3,3,3,3,3,3,3,3,3,3,3,3,3,3,3,3,3,3,3,3,3,3,3,3,3,3,3,3,3,3,3,3,
3,3,3,3,3,3,3,3,3,3,3,3,3,3,3,3,4),(36.782864454183,36.8477701180427,36.925262150472,
37.0027398988517,37.0802089431291,37.1576841947065,37.235159159569,37.3126506896138,
37.34663493007,37.4241269624992,37.501604710879,37.5790737551564,37.6565490067337,
37.7340239715966,37.8115155016411,37.8454997420974,37.9229917745268,38.0004695229064,
38.0779385671842,38.1554138187617,38.2328887836243,38.310380313669,38.3443645541247,
38.4218565865539,38.499334334934,38.5768033792115,38.6542786307892,38.7317535956524,
38.8092451256973,38.843229366152,38.9207213985812,38.998199146961,39.0756681912389,
39.1531434428164,39.2306184076787,39.3081099377237,39.3420941781794,39.4195862106086,
39.4970639589884,39.5745330032661,39.6520082548436,39.7294832197065,39.8069747497514,
39.8409589902067,39.9184510226361,39.9959287710154,40.0733978152927,40.1508730668702,
40.2283480317326,40.3058395617773,40.339823802234,40.4173158346631,40.4947935830427,
40.5722626273201,40.6497378788975,40.7272128437605,40.8047043738045,40.8386886142613,
40.8407044964987),.UNSPECIFIED.);
#590=B_SPLINE_CURVE_WITH_KNOTS('',3,(#74347,#74348,#74349,#74350,#74351,
#74352,#74353,#74354,#74355,#74356,#74357,#74358,#74359,#74360,#74361,#74362,
#74363,#74364,#74365,#74366,#74367,#74368,#74369,#74370,#74371,#74372,#74373,
#74374,#74375,#74376,#74377,#74378,#74379,#74380,#74381,#74382,#74383,#74384,
#74385,#74386,#74387,#74388,#74389,#74390,#74391,#74392,#74393,#74394,#74395,
#74396,#74397,#74398,#74399,#74400,#74401,#74402,#74403,#74404,#74405,#74406,
#74407,#74408,#74409,#74410,#74411,#74412,#74413,#74414,#74415,#74416,#74417,
#74418,#74419,#74420,#74421,#74422,#74423,#74424,#74425,#74426,#74427,#74428,
#74429,#74430,#74431,#74432,#74433,#74434,#74435,#74436,#74437,#74438,#74439,
#74440,#74441,#74442,#74443,#74444,#74445,#74446,#74447,#74448,#74449,#74450,
#74451,#74452,#74453,#74454,#74455,#74456,#74457,#74458,#74459,#74460,#74461,
#74462,#74463,#74464,#74465,#74466,#74467,#74468,#74469,#74470,#74471,#74472,
#74473,#74474,#74475,#74476,#74477,#74478,#74479,#74480,#74481,#74482,#74483,
#74484,#74485,#74486,#74487,#74488,#74489,#74490,#74491,#74492,#74493,#74494,
#74495,#74496,#74497,#74498,#74499,#74500,#74501,#74502,#74503,#74504,#74505,
#74506,#74507,#74508,#74509,#74510,#74511,#74512,#74513,#74514,#74515,#74516,
#74517,#74518),.UNSPECIFIED.,.F.,.F.,(4,3,3,3,3,3,3,3,3,3,3,3,3,3,3,3,3,
3,3,3,3,3,3,3,3,3,3,3,3,3,3,3,3,3,3,3,3,3,3,3,3,3,3,3,3,3,3,3,3,3,3,3,3,
3,3,3,3,4),(30.4997043503953,30.5777209304906,30.6551953822583,30.7334830265175,
30.8117706707768,30.889262703206,30.9667404515857,31.0442094958629,31.1216847474403,
31.1991597123029,31.2766512423475,31.3106354828041,31.3881275152334,31.4656052636131,
31.5430743078904,31.6205495594679,31.6980245243305,31.7755160543752,31.8095002948314,
31.8869923272607,31.9644700756404,32.0419391199176,32.1194143714951,32.1968893363578,
32.2743808664024,32.3083651068588,32.385857139288,32.4633348876678,32.5408039319451,
32.6182791835225,32.6957541483852,32.7732456784298,32.8072299188861,32.8847219513153,
32.9621996996951,33.0396687439724,33.1171439955498,33.1946189604125,33.2721104904572,
33.3060947309134,33.3835867633426,33.4610645117224,33.5385335559996,33.6160088075771,
33.6934837724398,33.7709753024844,33.8049595429408,33.8824515753701,33.9599293237497,
34.0373983680268,34.1148736196042,34.1923485844669,34.2698401145116,34.3038243549681,
34.3822177070359,34.4605943978029,34.5389569593193,34.5575191894877),
 .UNSPECIFIED.);
#591=B_SPLINE_CURVE_WITH_KNOTS('',3,(#74519,#74520,#74521,#74522,#74523,
#74524,#74525,#74526),.UNSPECIFIED.,.F.,.F.,(4,1,1,1,1,4),(34.5575191926081,
34.8026891669954,35.3015539790227,35.8004187910501,36.2992836030774,36.7828738679604),
 .UNSPECIFIED.);
#592=B_SPLINE_CURVE_WITH_KNOTS('',3,(#74528,#74529,#74530,#74531,#74532,
#74533,#74534,#74535,#74536,#74537,#74538,#74539,#74540,#74541,#74542,#74543,
#74544,#74545,#74546,#74547,#74548,#74549,#74550,#74551,#74552,#74553,#74554,
#74555,#74556,#74557,#74558,#74559,#74560,#74561,#74562,#74563,#74564,#74565,
#74566,#74567,#74568,#74569,#74570,#74571,#74572,#74573,#74574,#74575,#74576,
#74577,#74578,#74579,#74580,#74581,#74582,#74583,#74584,#74585,#74586,#74587,
#74588,#74589,#74590,#74591,#74592,#74593,#74594,#74595,#74596,#74597,#74598,
#74599,#74600,#74601,#74602,#74603,#74604,#74605,#74606,#74607,#74608,#74609,
#74610,#74611,#74612,#74613,#74614,#74615,#74616,#74617,#74618,#74619,#74620,
#74621),.UNSPECIFIED.,.F.,.F.,(4,3,3,3,3,3,3,3,3,3,3,3,3,3,3,3,3,3,3,3,
3,3,3,3,3,3,3,3,3,3,3,4),(34.5575191894877,34.6353433852827,34.7131680802738,
34.7910131120779,34.8523108699334,34.9298029023626,35.0072806507426,35.0847496950204,
35.1622249465979,35.2396999114606,35.3171914415054,35.3511756819607,35.4286677143899,
35.5061454627699,35.5836145070471,35.6610897586247,35.7385647234876,35.8160562535323,
35.8500404939881,35.9275325264173,36.0050102747971,36.0824793190741,36.1599545706517,
36.2374295355144,36.314921065559,36.3489053060154,36.4263967590605,36.5038736983943,
36.5813489641976,36.6588188367758,36.7362996359494,36.782864454183),
 .UNSPECIFIED.);
#593=B_SPLINE_CURVE_WITH_KNOTS('',3,(#74622,#74623,#74624,#74625,#74626,
#74627,#74628,#74629,#74630,#74631,#74632,#74633,#74634,#74635,#74636,#74637,
#74638,#74639,#74640,#74641,#74642,#74643,#74644,#74645,#74646,#74647,#74648,
#74649,#74650,#74651,#74652,#74653,#74654,#74655,#74656,#74657,#74658,#74659,
#74660,#74661,#74662,#74663,#74664,#74665,#74666,#74667,#74668,#74669,#74670,
#74671,#74672,#74673,#74674,#74675,#74676,#74677,#74678,#74679,#74680,#74681,
#74682,#74683,#74684,#74685,#74686,#74687,#74688,#74689,#74690,#74691,#74692,
#74693,#74694,#74695,#74696,#74697,#74698,#74699,#74700,#74701,#74702,#74703,
#74704,#74705,#74706,#74707,#74708,#74709,#74710,#74711,#74712,#74713,#74714,
#74715,#74716,#74717,#74718,#74719,#74720,#74721,#74722,#74723,#74724,#74725,
#74726,#74727,#74728,#74729,#74730,#74731,#74732,#74733,#74734,#74735,#74736,
#74737,#74738,#74739,#74740,#74741,#74742,#74743,#74744,#74745,#74746,#74747,
#74748,#74749,#74750,#74751,#74752,#74753,#74754,#74755,#74756,#74757,#74758,
#74759,#74760,#74761,#74762,#74763,#74764,#74765,#74766,#74767,#74768,#74769,
#74770,#74771,#74772,#74773,#74774,#74775,#74776,#74777,#74778,#74779,#74780,
#74781,#74782,#74783,#74784,#74785,#74786,#74787,#74788,#74789,#74790,#74791,
#74792,#74793),.UNSPECIFIED.,.F.,.F.,(4,3,3,3,3,3,3,3,3,3,3,3,3,3,3,3,3,
3,3,3,3,3,3,3,3,3,3,3,3,3,3,3,3,3,3,3,3,3,3,3,3,3,3,3,3,3,3,3,3,3,3,3,3,
3,3,3,3,4),(30.4997098142701,30.5771803637444,30.6546564701863,30.732131006469,
30.8096232719206,30.8613923737148,30.9388844061442,31.016362154524,31.0938311988014,
31.1713064503789,31.2487814152417,31.3262729452865,31.3602571857421,31.4377492181713,
31.5152269665509,31.5926960108281,31.6701712624054,31.747646227268,31.8251377573126,
31.8591219977694,31.9366140301987,32.0140917785784,32.0915608228557,32.1690360744331,
32.2465110392958,32.3240025693406,32.3579868097967,32.4354788422259,32.5129565906057,
32.590425634883,32.6679008864605,32.7453758513231,32.8228673813677,32.8568516218241,
32.9343436542533,33.0118214026331,33.0892904469103,33.1667656984877,33.2442406633505,
33.3217321933952,33.3557164338514,33.4332084662806,33.5106862146603,33.5881552589374,
33.6656305105148,33.7431054753776,33.8205970054223,33.8545812458787,33.9320732783079,
34.0095510266875,34.0870200709647,34.1644953225422,34.2419702874047,34.3194618174493,
34.3534460579061,34.4327535366758,34.5120401040698,34.5575191894205),
 .UNSPECIFIED.);
#594=B_SPLINE_CURVE_WITH_KNOTS('',3,(#74799,#74800,#74801,#74802,#74803,
#74804,#74805,#74806,#74807,#74808,#74809,#74810),.UNSPECIFIED.,.F.,.F.,
(4,1,1,1,1,1,1,1,1,4),(24.2164828558523,24.3265281144215,24.8253929264488,
25.3242577384762,25.8231225505035,26.3219873625308,26.8208521745581,27.3197169865855,
27.8185817986128,28.2743338450134),.UNSPECIFIED.);
#595=B_SPLINE_CURVE_WITH_KNOTS('',3,(#74811,#74812,#74813,#74814,#74815,
#74816,#74817,#74818,#74819,#74820,#74821,#74822,#74823,#74824,#74825,#74826,
#74827,#74828,#74829,#74830,#74831,#74832,#74833,#74834,#74835,#74836,#74837,
#74838,#74839,#74840,#74841,#74842,#74843,#74844,#74845,#74846,#74847,#74848,
#74849,#74850,#74851,#74852,#74853,#74854,#74855,#74856,#74857,#74858,#74859,
#74860,#74861,#74862,#74863,#74864,#74865,#74866,#74867,#74868,#74869,#74870,
#74871,#74872,#74873,#74874,#74875,#74876,#74877,#74878,#74879,#74880,#74881,
#74882,#74883,#74884,#74885,#74886,#74887,#74888,#74889,#74890,#74891,#74892,
#74893,#74894,#74895,#74896,#74897,#74898,#74899,#74900,#74901,#74902,#74903,
#74904,#74905,#74906,#74907),.UNSPECIFIED.,.F.,.F.,(4,3,3,3,3,3,3,3,3,3,
3,3,3,3,3,3,3,3,3,3,3,3,3,3,3,3,3,3,3,3,3,3,4),(28.2743338823081,28.3174466106401,
28.3949386430695,28.4724163914493,28.5498854357268,28.6273606873043,28.7048356521673,
28.7823271822121,28.8163114226675,28.8938034550967,28.9712812034763,29.0487502477537,
29.1262254993311,29.2037004641937,29.2811919942383,29.3151762346948,29.3926682671241,
29.4701460155037,29.547615059781,29.6250903113584,29.7025652762211,29.7800568062657,
29.8140410467221,29.8915330791514,29.969010827531,30.0464798718082,30.1239551233857,
30.2014300882484,30.2789216182931,30.3129058587495,30.3903971270004,30.4678751330957,
30.4997043503953),.UNSPECIFIED.);
#596=B_SPLINE_CURVE_WITH_KNOTS('',3,(#74909,#74910,#74911,#74912,#74913,
#74914,#74915,#74916,#74917,#74918,#74919,#74920,#74921,#74922,#74923,#74924,
#74925,#74926,#74927,#74928,#74929,#74930,#74931,#74932,#74933,#74934,#74935,
#74936,#74937,#74938,#74939,#74940,#74941,#74942,#74943,#74944,#74945,#74946,
#74947,#74948,#74949,#74950,#74951,#74952,#74953,#74954,#74955,#74956,#74957,
#74958,#74959,#74960,#74961,#74962,#74963,#74964,#74965,#74966,#74967,#74968,
#74969,#74970,#74971,#74972,#74973,#74974,#74975,#74976,#74977,#74978,#74979,
#74980,#74981,#74982,#74983,#74984,#74985,#74986,#74987,#74988,#74989,#74990,
#74991,#74992,#74993,#74994,#74995,#74996,#74997,#74998,#74999,#75000,#75001,
#75002,#75003,#75004,#75005),.UNSPECIFIED.,.F.,.F.,(4,3,3,3,3,3,3,3,3,3,
3,3,3,3,3,3,3,3,3,3,3,3,3,3,3,3,3,3,3,3,3,3,4),(28.2743338823081,28.3569496379083,
28.3670683135781,28.4445603460099,28.5220380943922,28.5995071386723,28.6769823902524,
28.7544573551178,28.8319488851651,28.8659331256054,28.9434251580338,29.0209029064128,
29.098371950689,29.1758472022655,29.2533221671273,29.3308136971711,29.3647979376328,
29.4422899700621,29.5197677184421,29.5972367627195,29.674712014297,29.7521869791598,
29.8296785092045,29.8636627496601,29.9411547820895,30.0186325304694,30.0961015747468,
30.1735768263243,30.2510517911872,30.328543321232,30.3625275616874,30.4400203072111,
30.4997098142701),.UNSPECIFIED.);
#597=B_SPLINE_CURVE_WITH_KNOTS('',3,(#75006,#75007,#75008,#75009,#75010,
#75011,#75012,#75013,#75014,#75015,#75016,#75017,#75018,#75019,#75020,#75021,
#75022,#75023,#75024,#75025,#75026,#75027,#75028,#75029,#75030,#75031,#75032,
#75033,#75034,#75035,#75036,#75037,#75038,#75039,#75040,#75041,#75042,#75043,
#75044,#75045,#75046,#75047,#75048,#75049,#75050,#75051,#75052,#75053,#75054,
#75055,#75056,#75057,#75058,#75059,#75060,#75061,#75062,#75063,#75064,#75065,
#75066,#75067,#75068,#75069,#75070,#75071,#75072,#75073,#75074,#75075,#75076,
#75077,#75078,#75079,#75080,#75081,#75082,#75083,#75084,#75085,#75086,#75087,
#75088,#75089,#75090,#75091,#75092,#75093,#75094,#75095,#75096,#75097,#75098,
#75099,#75100,#75101,#75102,#75103,#75104,#75105,#75106,#75107,#75108,#75109,
#75110,#75111,#75112,#75113,#75114,#75115,#75116,#75117,#75118,#75119,#75120,
#75121,#75122,#75123,#75124,#75125,#75126,#75127,#75128,#75129,#75130,#75131,
#75132,#75133,#75134,#75135,#75136,#75137,#75138,#75139,#75140,#75141,#75142,
#75143,#75144,#75145,#75146,#75147,#75148,#75149,#75150,#75151,#75152,#75153,
#75154,#75155,#75156,#75157,#75158,#75159,#75160,#75161,#75162,#75163,#75164,
#75165,#75166,#75167,#75168,#75169,#75170,#75171,#75172,#75173,#75174,#75175,
#75176,#75177),.UNSPECIFIED.,.F.,.F.,(4,3,3,3,3,3,3,3,3,3,3,3,3,3,3,3,3,
3,3,3,3,3,3,3,3,3,3,3,3,3,3,3,3,3,3,3,3,3,3,3,3,3,3,3,3,3,3,3,3,3,3,3,3,
3,3,3,3,4),(24.2164947951915,24.2963223062755,24.3761498173595,24.4536418492143,
24.5311195970121,24.6085886407024,24.6860638916884,24.7635388559585,24.8410303854126,
24.8750146293868,24.9525066621344,25.0299844108363,25.1074534554392,25.1849287073434,
25.2624036725332,25.3398952029039,25.3738794414141,25.4513714737075,25.5288492219499,
25.6063182660886,25.6837935175271,25.7612684822504,25.8387600121567,25.8727442534415,
25.9502362859097,26.0277140343293,26.1051830786465,26.1826583302636,26.2601332951656,
26.3376248252496,26.3716090654688,26.4491010978985,26.5265788462786,26.6040478905561,
26.6815231421342,26.7589981069978,26.8364896370432,26.8704738774961,26.9479659099148,
27.0254436582844,27.1029127025519,27.1803879541189,27.2578629189705,27.3353544490048,
27.3693386895235,27.4468307219618,27.5243084703507,27.6017775146373,27.679252766224,
27.756727731096,27.83421926115,27.8682035015508,27.9453872774562,28.0225556395814,
28.0997214532917,28.1768831987141,28.2540554491615,28.2743338822298),
 .UNSPECIFIED.);
#598=B_SPLINE_CURVE_WITH_KNOTS('',3,(#75183,#75184,#75185,#75186,#75187,
#75188,#75189,#75190,#75191),.UNSPECIFIED.,.F.,.F.,(4,1,1,1,1,1,4),(15.7079632679489,
15.8954480128949,16.3943128249222,16.8931776369496,17.3920424489769,17.8909072610042,
17.9333372203403),.UNSPECIFIED.);
#599=B_SPLINE_CURVE_WITH_KNOTS('',3,(#75193,#75194,#75195,#75196,#75197,
#75198),.UNSPECIFIED.,.F.,.F.,(4,1,1,4),(14.3988535768129,14.8977183888402,
15.3965832008676,15.7079632679489),.UNSPECIFIED.);
#600=B_SPLINE_CURVE_WITH_KNOTS('',3,(#75202,#75203,#75204,#75205,#75206,
#75207,#75208),.UNSPECIFIED.,.F.,.F.,(4,1,1,1,4),(13.8754803054952,14.3492318738749,
14.8480966859023,15.3469614979296,15.7079632679489),.UNSPECIFIED.);
#601=B_SPLINE_CURVE_WITH_KNOTS('',3,(#75209,#75210,#75211,#75212,#75213,
#75214,#75215,#75216,#75217),.UNSPECIFIED.,.F.,.F.,(4,1,1,1,1,1,4),(15.7079632679489,
15.8458263099569,16.3446911219842,16.8435559340116,17.3424207460389,17.8412855580662,
17.9333477466581),.UNSPECIFIED.);
#602=B_SPLINE_CURVE_WITH_KNOTS('',3,(#75223,#75224,#75225,#75226,#75227,
#75228,#75229,#75230),.UNSPECIFIED.,.F.,.F.,(4,2,2,4),(-0.249826015691648,
-0.174054989991414,-0.112681174836296,-5.98438861682063E-5),
 .UNSPECIFIED.);
#603=B_SPLINE_CURVE_WITH_KNOTS('',3,(#75233,#75234,#75235,#75236,#75237,
#75238,#75239,#75240,#75241,#75242,#75243,#75244,#75245,#75246,#75247,#75248,
#75249,#75250,#75251,#75252,#75253,#75254,#75255,#75256,#75257,#75258,#75259,
#75260,#75261,#75262,#75263,#75264,#75265,#75266,#75267,#75268,#75269,#75270,
#75271,#75272,#75273,#75274,#75275,#75276),.UNSPECIFIED.,.F.,.F.,(4,2,2,
2,2,2,2,2,2,2,2,2,2,2,2,2,2,2,2,2,2,4),(-6.11671048338158,-5.96153956264804,
-5.84115877786849,-5.80007352684886,-5.76536661656876,-5.67608165850516,
-5.61674511723677,-5.47922466329569,-5.43073195824578,-5.37491543409902,
-5.30049496163558,-5.27011467092952,-5.19890052636434,-5.12206091177934,
-5.10075658906977,-5.06249072850121,-4.97963646160468,-4.90348514082996,
-4.81921126869143,-4.74227675282595,-4.70012783424564,-4.66100346190723),
 .UNSPECIFIED.);
#604=B_SPLINE_CURVE_WITH_KNOTS('',3,(#75281,#75282,#75283,#75284,#75285,
#75286,#75287,#75288,#75289,#75290,#75291,#75292,#75293,#75294,#75295,#75296,
#75297,#75298,#75299,#75300,#75301,#75302,#75303,#75304,#75305,#75306,#75307,
#75308,#75309,#75310,#75311,#75312,#75313,#75314,#75315,#75316,#75317,#75318,
#75319,#75320,#75321,#75322,#75323,#75324,#75325,#75326,#75327,#75328,#75329,
#75330,#75331,#75332,#75333,#75334,#75335,#75336,#75337,#75338,#75339,#75340,
#75341,#75342,#75343,#75344,#75345,#75346,#75347,#75348,#75349,#75350,#75351,
#75352,#75353,#75354,#75355,#75356,#75357,#75358,#75359,#75360,#75361,#75362,
#75363,#75364,#75365,#75366,#75367,#75368,#75369,#75370,#75371,#75372,#75373,
#75374,#75375,#75376,#75377,#75378,#75379,#75380,#75381,#75382,#75383,#75384,
#75385,#75386,#75387,#75388,#75389,#75390,#75391,#75392,#75393,#75394,#75395,
#75396,#75397,#75398,#75399,#75400,#75401,#75402,#75403,#75404),
 .UNSPECIFIED.,.F.,.F.,(4,2,2,2,2,2,2,2,2,2,2,2,2,2,2,2,2,2,2,2,2,2,2,2,
2,2,2,2,2,2,2,2,2,2,2,2,2,2,2,2,2,2,2,2,2,2,2,2,2,2,2,2,2,2,2,2,2,2,2,2,
2,4),(-4.661040529428,-4.59250079239981,-4.5588280390274,-4.51925590365334,
-4.43950198910759,-4.38022384530102,-4.25820358191914,-4.20180510591333,
-4.12533749912705,-4.03567785246762,-3.96195778728872,-3.89280199334527,
-3.8472816427279,-3.77297244856651,-3.68479577805155,-3.54299662275098,
-3.49717304314424,-3.42207112732758,-3.32867078560331,-3.20988293964267,
-3.15147510198992,-3.07331444426717,-2.98453912420175,-2.91189784048555,
-2.81952245029366,-2.78141079113058,-2.69821153880586,-2.62153686814335,
-2.52615111761924,-2.45542875263231,-2.40669530834557,-2.26969074547352,
-2.18194656422033,-2.1068040420648,-2.06129408857846,-1.99216352691328,
-1.91846521303171,-1.82948024871057,-1.75180578992144,-1.69202736926351,
-1.58198232863079,-1.50512564938352,-1.42139742612079,-1.38353349166211,
-1.29151110712416,-1.21814585852054,-1.15910144667136,-1.07820422203281,
-1.03844509860151,-0.999978242961427,-0.872257699284099,-0.841905751085272,
-0.77267566309266,-0.703753678947113,-0.652879246690581,-0.52137716917312,
-0.491309869279923,-0.421533932405962,-0.357554499970899,-0.324129770168331,
-0.273276533780277,-0.249826015691648),.UNSPECIFIED.);
#605=B_SPLINE_CURVE_WITH_KNOTS('',3,(#75405,#75406,#75407,#75408,#75409,
#75410,#75411,#75412,#75413,#75414,#75415,#75416,#75417,#75418,#75419,#75420,
#75421,#75422,#75423,#75424,#75425,#75426,#75427,#75428,#75429,#75430,#75431,
#75432,#75433,#75434,#75435,#75436,#75437,#75438,#75439,#75440,#75441,#75442,
#75443,#75444,#75445,#75446,#75447,#75448,#75449,#75450,#75451,#75452,#75453,
#75454,#75455,#75456,#75457,#75458,#75459,#75460,#75461,#75462,#75463,#75464,
#75465,#75466,#75467,#75468,#75469,#75470,#75471,#75472,#75473,#75474,#75475,
#75476,#75477,#75478,#75479,#75480,#75481,#75482,#75483,#75484,#75485,#75486,
#75487,#75488,#75489,#75490,#75491,#75492,#75493,#75494,#75495,#75496,#75497,
#75498,#75499,#75500,#75501,#75502,#75503,#75504,#75505,#75506,#75507,#75508,
#75509,#75510,#75511,#75512,#75513,#75514,#75515,#75516,#75517,#75518,#75519,
#75520,#75521,#75522,#75523,#75524,#75525,#75526,#75527,#75528),
 .UNSPECIFIED.,.F.,.F.,(4,2,2,2,2,2,2,2,2,2,2,2,2,2,2,2,2,2,2,2,2,2,2,2,
2,2,2,2,2,2,2,2,2,2,2,2,2,2,2,2,2,2,2,2,2,2,2,2,2,2,2,2,2,2,2,2,2,2,2,2,
2,4),(-4.66100346190723,-4.62037419810526,-4.5611047479869,-4.43901396909629,
-4.38266566505239,-4.30620877569181,-4.21653926920206,-4.14280707990123,
-4.07379689549356,-4.02819886674058,-3.9537384540495,-3.86101999543191,
-3.73754481172534,-3.68200933338862,-3.60630718776622,-3.51625588941678,
-3.44270748925475,-3.35041373882792,-3.31227071068859,-3.22916600496052,
-3.152630467389,-3.05870243760212,-2.98464627030377,-2.93070219305535,-2.80439495350426,
-2.7743415054773,-2.70479137599409,-2.63583136164712,-2.58599116243935,
-2.45147919427703,-2.42137023471592,-2.35121774453874,-2.28694477035531,
-2.23994077889129,-2.19423332184233,-2.11283929689295,-2.03650221126673,
-1.95350491978024,-1.91531982736376,-1.82271481509619,-1.74911013529705,
-1.65920040265371,-1.58322961500161,-1.52738154155305,-1.40443151681069,
-1.37438276335948,-1.34002301095097,-1.25833941339007,-1.21907386153295,
-1.18046317812505,-1.05285490106838,-0.961457005362473,-0.886851249105894,
-0.841215261431666,-0.772329900198776,-0.698570457072661,-0.609018057937201,
-0.532354612408258,-0.475745252674886,-0.354073539092338,-0.294795850899468,
-0.249839284278359),.UNSPECIFIED.);
#606=B_SPLINE_CURVE_WITH_KNOTS('',3,(#75534,#75535,#75536,#75537,#75538,
#75539,#75540,#75541,#75542,#75543,#75544,#75545,#75546,#75547,#75548),
 .UNSPECIFIED.,.F.,.F.,(4,1,1,1,1,1,1,1,1,1,1,1,4),(51.9303482698305,52.3808052628696,
52.8796700748969,53.3785348869242,53.8773996989515,54.3762645109789,54.8751293230062,
55.3739941350335,55.8728589470609,56.3717237590882,56.8705885711155,57.3694533831428,
57.8577774402384),.UNSPECIFIED.);
#607=B_SPLINE_CURVE_WITH_KNOTS('',3,(#75549,#75550,#75551,#75552,#75553,
#75554,#75555,#75556,#75557,#75558,#75559,#75560),.UNSPECIFIED.,.F.,.F.,
(4,2,2,2,2,4),(-4.91076763008672,-4.89054942255246,-4.79539761919939,-4.7359292169242,
-4.67338213757578,-4.661040529428),.UNSPECIFIED.);
#608=B_SPLINE_CURVE_WITH_KNOTS('',3,(#75562,#75563,#75564,#75565,#75566,
#75567,#75568,#75569,#75570,#75571,#75572,#75573),.UNSPECIFIED.,.F.,.F.,
(4,2,2,2,2,4),(-0.249839284278359,-0.192910272014258,-0.153865892167779,
-0.098709197194812,-0.0384561197471015,-0.000114506416299162),
 .UNSPECIFIED.);
#609=B_SPLINE_CURVE_WITH_KNOTS('',3,(#75574,#75575,#75576,#75577,#75578,
#75579,#75580,#75581,#75582,#75583,#75584,#75585,#75586,#75587,#75588,#75589,
#75590,#75591,#75592,#75593,#75594,#75595,#75596,#75597,#75598,#75599,#75600,
#75601,#75602,#75603,#75604,#75605,#75606,#75607,#75608,#75609,#75610,#75611,
#75612,#75613,#75614,#75615,#75616,#75617,#75618,#75619,#75620,#75621,#75622,
#75623,#75624,#75625,#75626,#75627,#75628,#75629,#75630,#75631,#75632,#75633,
#75634,#75635,#75636,#75637,#75638,#75639,#75640,#75641,#75642,#75643,#75644,
#75645,#75646,#75647,#75648,#75649,#75650,#75651,#75652,#75653,#75654,#75655,
#75656,#75657,#75658,#75659,#75660,#75661,#75662,#75663,#75664,#75665,#75666,
#75667,#75668,#75669,#75670,#75671,#75672,#75673,#75674,#75675,#75676,#75677,
#75678,#75679,#75680,#75681,#75682,#75683,#75684,#75685,#75686,#75687,#75688,
#75689,#75690,#75691,#75692,#75693,#75694,#75695,#75696,#75697,#75698,#75699,
#75700,#75701,#75702,#75703,#75704,#75705,#75706,#75707,#75708,#75709,#75710,
#75711,#75712,#75713,#75714,#75715,#75716,#75717,#75718,#75719,#75720,#75721,
#75722,#75723,#75724,#75725,#75726,#75727,#75728,#75729,#75730,#75731,#75732,
#75733,#75734,#75735,#75736,#75737,#75738,#75739,#75740,#75741,#75742,#75743,
#75744,#75745,#75746,#75747,#75748,#75749,#75750,#75751,#75752,#75753,#75754,
#75755,#75756,#75757,#75758,#75759,#75760,#75761,#75762,#75763,#75764,#75765,
#75766,#75767,#75768,#75769,#75770,#75771,#75772,#75773,#75774,#75775,#75776,
#75777,#75778,#75779,#75780,#75781,#75782,#75783,#75784,#75785,#75786,#75787,
#75788,#75789,#75790,#75791,#75792,#75793,#75794,#75795,#75796,#75797,#75798,
#75799,#75800,#75801,#75802,#75803,#75804,#75805,#75806,#75807,#75808,#75809,
#75810,#75811,#75812,#75813,#75814,#75815,#75816,#75817,#75818,#75819,#75820,
#75821,#75822,#75823),.UNSPECIFIED.,.F.,.F.,(4,3,3,3,3,3,3,3,3,3,3,3,3,
3,3,3,3,3,3,3,3,3,3,3,3,3,3,3,3,3,3,3,3,3,3,3,3,3,3,3,3,3,3,3,3,3,3,3,3,
3,3,3,3,3,3,3,3,3,3,3,3,3,3,3,3,3,3,3,3,3,3,3,3,3,3,3,3,3,3,3,3,3,3,4),
(-54.1185379116474,-54.0370154397113,-53.9554652497997,-53.8773996989515,
-53.7969976029293,-53.7166107711432,-53.6320918000885,-53.5517075662432,
-53.4713225283434,-53.3909212255061,-53.3785348869242,-53.2981327907243,
-53.2177459587585,-53.1332269877931,-53.0528427537661,-52.9724577156843,
-52.8920564126664,-52.8796700748969,-52.7992679787358,-52.7188811468092,
-52.6343621758243,-52.5539779418364,-52.4735929037938,-52.3931916008148,
-52.3808052628695,-52.3004031667197,-52.2200163348046,-52.135497363814,
-52.0551131298381,-51.9747280918076,-51.8943267888406,-51.8819404508422,
-51.8015383546724,-51.721151522737,-51.6366325517565,-51.55624831776,-51.4758632797088,
-51.3954619767211,-51.3830756388149,-51.3026735426601,-51.2222867107398,
-51.1377677397518,-51.0573835057707,-50.9769984677349,-50.8965971647625,
-50.8842108267876,-50.8038087306244,-50.7234218986957,-50.6389029277118,
-50.5585186937222,-50.4781336556778,-50.3977323526969,-50.3853460147602,
-50.3049439186006,-50.2245570866755,-50.1400381156899,-50.0596538817039,
-49.9792688436632,-49.8988675406859,-49.8864812027329,-49.8060791065723,
-49.7256922746463,-49.6411733036611,-49.5607890696742,-49.4804040316324,
-49.4000027286542,-49.3876163907056,-49.307214294545,-49.226827462619,-49.1423084916338,
-49.0619242576469,-48.9815392196051,-48.9011379166269,-48.8887515786783,
-48.8083494825178,-48.7279626505919,-48.6434436796066,-48.5630594456198,
-48.4826744075783,-48.4022731045999,-48.3898867666509,-48.3094854295042,
-48.2290975551199,-48.1910843038492),.UNSPECIFIED.);
#610=B_SPLINE_CURVE_WITH_KNOTS('',3,(#75829,#75830,#75831,#75832,#75833,
#75834,#75835,#75836,#75837,#75838,#75839,#75840,#75841,#75842,#75843,#75844,
#75845,#75846,#75847,#75848,#75849,#75850,#75851,#75852,#75853,#75854,#75855,
#75856,#75857,#75858,#75859,#75860,#75861,#75862,#75863,#75864,#75865,#75866,
#75867,#75868,#75869,#75870,#75871,#75872,#75873,#75874,#75875,#75876,#75877,
#75878,#75879,#75880,#75881,#75882,#75883,#75884,#75885,#75886,#75887,#75888,
#75889,#75890,#75891,#75892,#75893,#75894,#75895,#75896,#75897,#75898,#75899,
#75900,#75901,#75902,#75903,#75904,#75905,#75906,#75907,#75908,#75909,#75910,
#75911,#75912,#75913,#75914,#75915,#75916,#75917,#75918,#75919,#75920,#75921,
#75922,#75923,#75924,#75925,#75926,#75927,#75928,#75929,#75930,#75931,#75932,
#75933,#75934,#75935,#75936,#75937,#75938,#75939,#75940,#75941,#75942,#75943,
#75944,#75945,#75946,#75947,#75948,#75949,#75950,#75951,#75952,#75953,#75954,
#75955,#75956,#75957,#75958,#75959,#75960,#75961,#75962,#75963,#75964,#75965,
#75966,#75967,#75968,#75969,#75970,#75971,#75972,#75973,#75974,#75975,#75976,
#75977,#75978,#75979,#75980,#75981,#75982,#75983,#75984,#75985,#75986,#75987,
#75988,#75989,#75990,#75991,#75992,#75993,#75994,#75995,#75996,#75997,#75998,
#75999,#76000,#76001,#76002,#76003,#76004,#76005,#76006,#76007,#76008,#76009,
#76010,#76011,#76012,#76013,#76014,#76015,#76016,#76017,#76018,#76019,#76020,
#76021,#76022,#76023,#76024,#76025,#76026,#76027,#76028,#76029,#76030,#76031,
#76032,#76033,#76034,#76035,#76036,#76037,#76038,#76039,#76040,#76041,#76042,
#76043,#76044,#76045,#76046,#76047,#76048,#76049,#76050,#76051,#76052,#76053,
#76054,#76055,#76056,#76057,#76058,#76059,#76060,#76061,#76062,#76063,#76064,
#76065,#76066,#76067,#76068,#76069,#76070,#76071,#76072,#76073,#76074,#76075,
#76076,#76077,#76078),.UNSPECIFIED.,.F.,.F.,(4,3,3,3,3,3,3,3,3,3,3,3,3,
3,3,3,3,3,3,3,3,3,3,3,3,3,3,3,3,3,3,3,3,3,3,3,3,3,3,3,3,3,3,3,3,3,3,3,3,
3,3,3,3,3,3,3,3,3,3,3,3,3,3,3,3,3,3,3,3,3,3,3,3,3,3,3,3,3,3,3,3,3,3,4),
(45.6471469631167,45.7275310616107,45.8115468840625,45.8955627065143,45.9759648026746,
46.0563516346004,46.1408706055857,46.2212548395724,46.3016398776137,46.3820411805914,
46.3944275185416,46.474829614702,46.5552164466278,46.6397354176131,46.7201196515999,
46.8005046896415,46.8809059926195,46.8932923305689,46.9736944267296,47.0540812586556,
47.1386002296408,47.2189844636279,47.2993695016697,47.3797708046479,47.3921571425963,
47.4725592387567,47.5529460706825,47.6374650416678,47.7178492756546,47.7982343136961,
47.878635616674,47.8910219546236,47.9714240507842,48.0518108827102,48.1363298536954,
48.2167140876824,48.297099125724,48.3775004287023,48.3898867666509,48.4702888628112,
48.5506756947369,48.6351946657222,48.7155788997089,48.7959639377504,48.8763652407283,
48.8887515786782,48.969153674839,49.0495405067652,49.1340594777503,49.2144437117374,
49.2948287497792,49.3752300527577,49.3876163907056,49.4680184868661,49.5484053187922,
49.6329242897774,49.7133085237644,49.793693561806,49.874094864784,49.8864812027329,
49.9668832988924,50.0472701308175,50.1317891018032,50.212173335789,50.2925583738295,
50.3729596768067,50.3853460147602,50.4657481109236,50.5461349428522,50.6306539138361,
50.7110381478257,50.7914231858703,50.871824488851,50.8842108267876,50.9646129229422,
51.0449997548621,51.1295187258503,51.2099029598313,51.290287997867,51.3706893008394,
51.3830756388149,51.4656515093945,51.5482033685856,51.5745921485727),
 .UNSPECIFIED.);
#611=B_SPLINE_CURVE_WITH_KNOTS('',3,(#76079,#76080,#76081,#76082,#76083),
 .UNSPECIFIED.,.F.,.F.,(4,1,4),(51.5745921485727,51.8819404508422,51.9303482698305),
 .UNSPECIFIED.);
#612=B_SPLINE_CURVE_WITH_KNOTS('',3,(#76085,#76086,#76087,#76088,#76089,
#76090,#76091,#76092,#76093,#76094,#76095,#76096,#76097,#76098,#76099,#76100),
 .UNSPECIFIED.,.F.,.F.,(4,3,3,3,3,4),(-48.1910843038492,-48.1106976837031,
-48.030313872139,-47.9499108869887,-47.8910219546236,-47.8353526044678),
 .UNSPECIFIED.);
#613=B_SPLINE_CURVE_WITH_KNOTS('',3,(#76101,#76102,#76103,#76104,#76105,
#76106,#76107,#76108,#76109,#76110,#76111,#76112,#76113,#76114,#76115,#76116,
#76117,#76118,#76119,#76120,#76121,#76122,#76123,#76124,#76125,#76126,#76127,
#76128,#76129,#76130,#76131,#76132,#76133,#76134,#76135,#76136,#76137,#76138,
#76139,#76140,#76141,#76142,#76143,#76144,#76145,#76146,#76147,#76148,#76149,
#76150,#76151,#76152,#76153,#76154,#76155,#76156,#76157,#76158,#76159,#76160,
#76161,#76162,#76163,#76164,#76165,#76166,#76167,#76168,#76169,#76170,#76171,
#76172,#76173,#76174,#76175,#76176,#76177,#76178,#76179,#76180,#76181,#76182,
#76183,#76184,#76185,#76186,#76187,#76188,#76189,#76190,#76191,#76192,#76193,
#76194,#76195,#76196,#76197,#76198,#76199,#76200,#76201,#76202,#76203,#76204,
#76205,#76206,#76207,#76208,#76209,#76210,#76211,#76212),.UNSPECIFIED.,
 .F.,.F.,(4,2,2,2,2,2,2,2,2,2,2,2,2,2,2,2,2,2,2,2,2,2,2,2,2,2,2,2,2,2,2,
2,2,2,2,2,2,2,2,2,2,2,2,2,2,2,2,2,2,2,2,2,2,2,2,4),(-8.82308834836121,-8.69631405692605,
-8.66999828107067,-8.54091357144238,-8.50792268417827,-8.43201046834799,
-8.338862235828,-8.21679152542147,-8.16041651382544,-8.08395624499135,-7.99428699052817,
-7.92057172446897,-7.85131090598304,-7.80584059133933,-7.73170485979139,
-7.63942132907712,-7.5135137114328,-7.47436040599107,-7.43534619183455,
-7.35113770563209,-7.291786734327,-7.15768916435272,-7.10765366824809,-7.03840883283788,
-6.9692180267347,-6.93916039717996,-6.81228266182114,-6.75864265335129,
-6.68492027824907,-6.6174717547749,-6.58742052764269,-6.46581143634332,
-6.40915891083922,-6.33245179385895,-6.24291004586388,-6.16913900776438,
-6.06814460197658,-6.0259275516604,-5.94620168726619,-5.88691766352201,
-5.76524317810062,-5.70862762352981,-5.63195257300178,-5.54239176883554,
-5.46862692200963,-5.39974181860447,-5.35410188266291,-5.27948505219832,
-5.18652146927599,-5.06438139706198,-5.00804798984591,-4.93162521274094,
-4.84193673418545,-4.76822994855434,-4.69885186192799,-4.66124588486828),
 .UNSPECIFIED.);
#614=B_SPLINE_CURVE_WITH_KNOTS('',3,(#76218,#76219,#76220,#76221,#76222,
#76223,#76224,#76225,#76226,#76227,#76228,#76229,#76230,#76231,#76232,#76233,
#76234,#76235,#76236,#76237,#76238,#76239,#76240,#76241,#76242,#76243,#76244,
#76245,#76246,#76247,#76248,#76249,#76250,#76251,#76252,#76253,#76254,#76255,
#76256,#76257,#76258,#76259,#76260,#76261,#76262,#76263,#76264,#76265,#76266,
#76267,#76268,#76269,#76270,#76271,#76272,#76273,#76274,#76275,#76276,#76277,
#76278,#76279,#76280,#76281,#76282,#76283,#76284,#76285,#76286,#76287,#76288,
#76289,#76290,#76291,#76292,#76293,#76294,#76295,#76296,#76297,#76298,#76299,
#76300,#76301,#76302,#76303,#76304,#76305,#76306,#76307,#76308,#76309,#76310,
#76311,#76312,#76313,#76314,#76315,#76316,#76317,#76318,#76319,#76320,#76321,
#76322,#76323,#76324,#76325,#76326,#76327,#76328,#76329,#76330,#76331),
 .UNSPECIFIED.,.F.,.F.,(4,2,2,2,2,2,2,2,2,2,2,2,2,2,2,2,2,2,2,2,2,2,2,2,
2,2,2,2,2,2,2,2,2,2,2,2,2,2,2,2,2,2,2,2,2,2,2,2,2,2,2,2,2,2,2,2,4),(-4.16167409877826,
-4.14888454665581,-4.11080878728497,-4.01816330560154,-3.94527840833286,
-3.91504806802662,-3.84264795681711,-3.78287916929053,-3.73471581770899,
-3.60099813523087,-3.50826304914553,-3.43415092475662,-3.38868875064578,
-3.3194187215629,-3.24570792663102,-3.15604587741013,-3.07959623958393,
-3.02322670589989,-2.90115708907312,-2.80795727498646,-2.73364439917479,
-2.68811150026171,-2.61897598470416,-2.54525427184331,-2.45561283870726,
-2.37911898605323,-2.32270069107514,-2.20070879838926,-2.17065969565455,
-2.13637842611587,-2.05480989617438,-2.01540853311985,-1.97705260970872,
-1.84989807897117,-1.75770150776069,-1.68280150972009,-1.63706104876533,
-1.49460844929561,-1.40530489135814,-1.32815945043843,-1.2709924151342,
-1.15023580496727,-1.05696856452268,-0.982305019221087,-0.936648409373202,
-0.867832919528015,-0.794053713764026,-0.704542709873163,-0.627795627335843,
-0.571091675400024,-0.449573467515136,-0.390294377617773,-0.288476142994649,
-0.249335000370875,-0.114036524571827,-0.0706819242005296,-0.000108410259028435),
 .UNSPECIFIED.);
#615=B_SPLINE_CURVE_WITH_KNOTS('',3,(#76332,#76333,#76334,#76335,#76336,
#76337,#76338,#76339,#76340,#76341,#76342,#76343,#76344,#76345,#76346,#76347,
#76348,#76349,#76350),.UNSPECIFIED.,.F.,.F.,(4,3,3,3,3,3,4),(45.2914068413931,
45.3766260457133,45.3966978944869,45.4771000160926,45.5574858748033,45.637864107376,
45.6471469631167),.UNSPECIFIED.);
#616=B_SPLINE_CURVE_WITH_KNOTS('',3,(#76351,#76352,#76353,#76354,#76355,
#76356,#76357,#76358,#76359,#76360,#76361,#76362,#76363,#76364,#76365,#76366,
#76367,#76368,#76369,#76370,#76371,#76372,#76373,#76374,#76375,#76376,#76377,
#76378,#76379,#76380,#76381,#76382,#76383,#76384,#76385,#76386,#76387,#76388,
#76389,#76390,#76391,#76392,#76393,#76394,#76395,#76396,#76397,#76398,#76399,
#76400,#76401,#76402,#76403,#76404,#76405,#76406,#76407,#76408,#76409,#76410,
#76411,#76412,#76413,#76414,#76415,#76416,#76417,#76418,#76419,#76420,#76421,
#76422,#76423,#76424,#76425,#76426,#76427,#76428,#76429,#76430,#76431,#76432,
#76433,#76434,#76435,#76436,#76437,#76438,#76439,#76440,#76441,#76442,#76443,
#76444,#76445,#76446,#76447,#76448,#76449,#76450,#76451,#76452,#76453,#76454,
#76455,#76456,#76457,#76458,#76459,#76460,#76461,#76462,#76463,#76464,#76465,
#76466,#76467,#76468,#76469,#76470),.UNSPECIFIED.,.F.,.F.,(4,2,2,2,2,2,
2,2,2,2,2,2,2,2,2,2,2,2,2,2,2,2,2,2,2,2,2,2,2,2,2,2,2,2,2,2,2,2,2,2,2,2,
2,2,2,2,2,2,2,2,2,2,2,2,2,2,2,2,2,4),(-4.66124588486828,-4.65344182834346,
-4.57947860386115,-4.48869940087069,-4.41147586212013,-4.32801044803778,
-4.28994307687754,-4.24560544594292,-4.13722203158076,-4.05809115658597,
-3.96022500483084,-3.90631313505404,-3.77993448887484,-3.68712977428591,
-3.60884781406385,-3.55026396953155,-3.43174175045692,-3.3382346457669,
-3.2631698219336,-3.21736953987103,-3.07535718732895,-2.9868208205041,-2.90817316169504,
-2.84909713122432,-2.73132982588684,-2.63447581380076,-2.55859404202909,
-2.50284231628825,-2.37971692288725,-2.32044065727856,-2.24058148245293,
-2.19861559446752,-2.18067847794665,-2.12669884520124,-2.03759783927625,
-1.96140012860537,-1.8784789597153,-1.84025601220625,-1.74728669698988,
-1.67371290461062,-1.58372363507163,-1.50789987830291,-1.45220897795329,
-1.3289842823785,-1.26970952277594,-1.1898420329682,-1.14789481369276,-1.12995121607658,
-1.07593299471434,-0.986902782999391,-0.910709935639108,-0.827792353068139,
-0.789569337301891,-0.696593795183355,-0.623022349692111,-0.533033224461751,
-0.457214579369248,-0.401528548325178,-0.280196426907405,-0.249814737108548),
 .UNSPECIFIED.);
#617=B_SPLINE_CURVE_WITH_KNOTS('',3,(#76475,#76476,#76477,#76478,#76479,
#76480,#76481,#76482,#76483,#76484,#76485,#76486,#76487,#76488,#76489,#76490,
#76491,#76492,#76493,#76494,#76495,#76496,#76497,#76498,#76499,#76500,#76501,
#76502,#76503,#76504,#76505,#76506,#76507,#76508,#76509,#76510,#76511,#76512,
#76513,#76514,#76515,#76516,#76517,#76518,#76519,#76520,#76521,#76522,#76523,
#76524,#76525,#76526,#76527,#76528,#76529,#76530,#76531,#76532,#76533,#76534,
#76535,#76536,#76537,#76538,#76539,#76540,#76541,#76542,#76543,#76544,#76545,
#76546,#76547,#76548,#76549,#76550,#76551,#76552,#76553,#76554,#76555,#76556,
#76557,#76558,#76559,#76560,#76561,#76562,#76563,#76564,#76565,#76566,#76567,
#76568,#76569,#76570,#76571,#76572,#76573,#76574,#76575,#76576,#76577,#76578,
#76579,#76580,#76581,#76582,#76583,#76584,#76585,#76586,#76587,#76588,#76589,
#76590),.UNSPECIFIED.,.F.,.F.,(4,2,2,2,2,2,2,2,2,2,2,2,2,2,2,2,2,2,2,2,
2,2,2,2,2,2,2,2,2,2,2,2,2,2,2,2,2,2,2,2,2,2,2,2,2,2,2,2,2,2,2,2,2,2,2,2,
2,4),(-8.57312334748902,-8.53068440591889,-8.4654296892502,-8.3748028049429,
-8.32771669325542,-8.26328253987196,-8.19317209872651,-8.16306359739018,
-8.02872601189461,-7.97880430771087,-7.90972087403233,-7.84032131490915,
-7.81026567485648,-7.68371741211631,-7.62990290151605,-7.55598834015279,
-7.48859632118536,-7.45854586530168,-7.33728694601201,-7.2804261156745,
-7.20353791991617,-7.11409370843184,-7.04028315253009,-6.97158618850328,
-6.92589708093375,-6.85113848639895,-6.7578405474679,-6.63747357215866,
-6.58006645651545,-6.50271548725764,-6.41351209753925,-6.27111868167746,
-6.22537060865583,-6.15044581089919,-6.05708645490686,-5.93749777875824,
-5.87960385331488,-5.80185639149972,-5.71285790968482,-5.57058277654793,
-5.52481997348399,-5.44985356946362,-5.35715840607209,-5.23506542432103,
-5.17871172553286,-5.10227213746364,-5.01260018449415,-4.93889309841728,
-4.86958586254518,-4.82414441152635,-4.75008766188793,-4.65834226292778,
-4.52079689347961,-4.47443898077894,-4.41144438421492,-4.30925568253923,
-4.23223994902498,-4.16167409877826),.UNSPECIFIED.);
#618=B_SPLINE_CURVE_WITH_KNOTS('',3,(#76592,#76593,#76594,#76595,#76596,
#76597,#76598,#76599,#76600,#76601),.UNSPECIFIED.,.F.,.F.,(4,2,2,2,4),(-0.249814737108548,
-0.220876598911715,-0.110400142751405,-0.0942961602729965,-6.03191603578172E-5),
 .UNSPECIFIED.);
#619=B_SPLINE_CURVE_WITH_KNOTS('',3,(#76602,#76603,#76604,#76605,#76606,
#76607,#76608,#76609,#76610,#76611,#76612,#76613,#76614,#76615,#76616,#76617),
 .UNSPECIFIED.,.F.,.F.,(4,1,1,1,1,1,1,1,1,1,1,1,1,4),(-35.2689819901086,
-34.920536841913,-34.4216720298857,-33.9228072178584,-33.4239424058311,
-32.9250775938037,-32.4262127817764,-31.9273479697491,-31.4284831577217,
-30.9296183456944,-30.4307535336671,-29.9318887216397,-29.4330239096124,
-29.3415126415508),.UNSPECIFIED.);
#620=B_SPLINE_CURVE_WITH_KNOTS('',3,(#76623,#76624,#76625,#76626,#76627,
#76628,#76629,#76630,#76631,#76632,#76633,#76634,#76635,#76636,#76637,#76638,
#76639,#76640,#76641,#76642,#76643,#76644,#76645,#76646,#76647,#76648,#76649,
#76650,#76651,#76652,#76653,#76654,#76655,#76656,#76657,#76658,#76659,#76660,
#76661,#76662,#76663,#76664,#76665,#76666,#76667,#76668,#76669,#76670,#76671,
#76672,#76673,#76674,#76675,#76676,#76677,#76678,#76679,#76680,#76681,#76682,
#76683,#76684,#76685,#76686,#76687,#76688,#76689,#76690,#76691,#76692,#76693,
#76694,#76695,#76696,#76697,#76698,#76699,#76700,#76701,#76702,#76703,#76704,
#76705,#76706,#76707,#76708,#76709,#76710,#76711,#76712,#76713,#76714,#76715,
#76716,#76717,#76718,#76719,#76720,#76721,#76722,#76723,#76724,#76725,#76726,
#76727,#76728,#76729,#76730,#76731,#76732,#76733,#76734,#76735,#76736,#76737,
#76738,#76739,#76740,#76741,#76742,#76743,#76744,#76745,#76746),
 .UNSPECIFIED.,.F.,.F.,(4,2,2,2,2,2,2,2,2,2,2,2,2,2,2,2,2,2,2,2,2,2,2,2,
2,2,2,2,2,2,2,2,2,2,2,2,2,2,2,2,2,2,2,2,2,2,2,2,2,2,2,2,2,2,2,2,2,2,2,2,
2,4),(-4.16167874312325,-4.13977816237221,-4.06388049611118,-4.00811359479904,
-3.88500006385136,-3.8257199464703,-3.74585757730773,-3.70388552452625,
-3.68594859760857,-3.63197326719183,-3.54285304205606,-3.46664983935468,
-3.38372298659274,-3.34549775091462,-3.25252395247419,-3.17894528630053,
-3.08895064772496,-3.01312119614296,-2.95742594007616,-2.83419463348202,
-2.77491606531558,-2.69504356719102,-2.65309339842942,-2.63514875108143,
-2.58112766114741,-2.49209066550481,-2.41589291548282,-2.33296997835701,
-2.29474451174723,-2.20176298173821,-2.12818680192912,-2.03819197996319,
-1.96236827599743,-1.90667856023484,-1.78344247663634,-1.72416520137181,
-1.64429369072946,-1.60234572141077,-1.5844009584494,-1.53037812481442,
-1.44134808067491,-1.36515220491252,-1.28223118400461,-1.24400647602509,
-1.15102635292996,-1.07745181290136,-0.987458799240072,-0.91163698014631,
-0.855948729445594,-0.732714845060695,-0.673438847420675,-0.593569012083775,
-0.551622025519284,-0.533677618286453,-0.479655770120658,-0.392556161143309,
-0.33232033472783,-0.244435098865594,-0.204569805683055,-0.171101035364585,
-0.0522159782253246,-6.02492052133978E-5),.UNSPECIFIED.);
#621=B_SPLINE_CURVE_WITH_KNOTS('',3,(#76747,#76748,#76749,#76750,#76751,
#76752,#76753,#76754,#76755,#76756),.UNSPECIFIED.,.F.,.F.,(4,2,2,2,4),(-8.82288650888697,
-8.71171349505023,-8.67904854995692,-8.59378203487709,-8.57312334748902),
 .UNSPECIFIED.);
#622=B_SPLINE_CURVE_WITH_KNOTS('',3,(#76758,#76759,#76760,#76761),
 .UNSPECIFIED.,.F.,.F.,(4,4),(-29.3415126415508,-28.9857967263874),
 .UNSPECIFIED.);
#623=B_SPLINE_CURVE_WITH_KNOTS('',3,(#76762,#76763,#76764,#76765,#76766,
#76767,#76768,#76769,#76770,#76771,#76772,#76773,#76774,#76775,#76776,#76777,
#76778,#76779,#76780,#76781,#76782,#76783,#76784,#76785,#76786,#76787,#76788,
#76789,#76790,#76791,#76792,#76793,#76794,#76795,#76796,#76797,#76798,#76799,
#76800,#76801,#76802,#76803,#76804,#76805,#76806,#76807,#76808,#76809,#76810,
#76811,#76812,#76813,#76814,#76815,#76816,#76817,#76818,#76819,#76820,#76821,
#76822,#76823,#76824,#76825,#76826,#76827,#76828,#76829,#76830,#76831,#76832,
#76833,#76834,#76835,#76836,#76837,#76838,#76839,#76840,#76841,#76842,#76843,
#76844,#76845,#76846,#76847,#76848,#76849,#76850,#76851,#76852,#76853,#76854,
#76855,#76856,#76857,#76858,#76859,#76860,#76861,#76862,#76863,#76864,#76865,
#76866,#76867,#76868,#76869,#76870,#76871,#76872,#76873,#76874,#76875,#76876,
#76877,#76878,#76879,#76880,#76881,#76882,#76883,#76884,#76885,#76886,#76887,
#76888,#76889,#76890,#76891,#76892,#76893,#76894,#76895,#76896,#76897,#76898,
#76899,#76900,#76901,#76902,#76903,#76904,#76905,#76906,#76907,#76908,#76909,
#76910,#76911,#76912,#76913,#76914,#76915,#76916,#76917,#76918,#76919,#76920,
#76921,#76922,#76923,#76924,#76925,#76926,#76927,#76928,#76929,#76930,#76931,
#76932,#76933,#76934,#76935,#76936,#76937,#76938,#76939,#76940,#76941,#76942,
#76943,#76944,#76945,#76946,#76947,#76948,#76949,#76950,#76951,#76952,#76953,
#76954,#76955,#76956,#76957,#76958,#76959,#76960,#76961,#76962,#76963,#76964,
#76965,#76966,#76967,#76968,#76969,#76970,#76971,#76972,#76973,#76974,#76975,
#76976,#76977,#76978,#76979,#76980,#76981,#76982,#76983,#76984,#76985,#76986,
#76987,#76988,#76989,#76990,#76991,#76992,#76993,#76994,#76995,#76996,#76997,
#76998,#76999,#77000,#77001,#77002,#77003,#77004,#77005,#77006,#77007,#77008,
#77009,#77010,#77011),.UNSPECIFIED.,.F.,.F.,(4,3,3,3,3,3,3,3,3,3,3,3,3,
3,3,3,3,3,3,3,3,3,3,3,3,3,3,3,3,3,3,3,3,3,3,3,3,3,3,3,3,3,3,3,3,3,3,3,3,
3,3,3,3,3,3,3,3,3,3,3,3,3,3,3,3,3,3,3,3,3,3,3,3,3,3,3,3,3,3,3,3,3,3,4),
(-28.985796682929,-28.9341590975851,-28.8537570014243,-28.7733701694982,
-28.6888511985131,-28.608466964526,-28.5280819264842,-28.4476806235058,
-28.4352942855578,-28.3548921893973,-28.2745053574713,-28.1899863864861,
-28.1096021524991,-28.0292171144574,-27.9488158114792,-27.9364294735304,
-27.8560273773699,-27.775640545444,-27.6911215744588,-27.6107373404719,
-27.5303523024302,-27.4499509994519,-27.4375646615031,-27.3571625653427,
-27.2767757334169,-27.1922567624316,-27.1118725284448,-27.0314874904033,
-26.9510861874253,-26.9386998494758,-26.8582977533151,-26.7779109213891,
-26.6933919504039,-26.6130077164169,-26.5326226783752,-26.4522213753969,
-26.4398350374484,-26.3594329412879,-26.279046109362,-26.1945271383768,
-26.1141429043899,-26.0337578663484,-25.9533565633703,-25.9409702254211,
-25.8605681292606,-25.7801812973347,-25.6956623263495,-25.6152780923626,
-25.534893054321,-25.4544917513429,-25.4421054133938,-25.3617033172334,
-25.2813164853074,-25.1967975143222,-25.1164132803353,-25.0360282422938,
-24.9556269393158,-24.9432406013665,-24.8628385052059,-24.7824516732798,
-24.6979327022946,-24.6175484683076,-24.5371634302657,-24.4567621272875,
-24.4443757893391,-24.3639736931787,-24.2835868612527,-24.1990678902675,
-24.1186836562807,-24.0382986182391,-23.9578973152611,-23.9455109773118,
-23.8651088811514,-23.7847220492255,-23.7002030782402,-23.6198188442535,
-23.5394338062118,-23.4590325032338,-23.4466461652845,-23.3662448479451,
-23.285852924114,-23.2054721193945,-23.1250839303849,-23.0583686585911),
 .UNSPECIFIED.);
#624=B_SPLINE_CURVE_WITH_KNOTS('',3,(#77016,#77017,#77018,#77019,#77020,
#77021,#77022,#77023,#77024,#77025,#77026,#77027,#77028,#77029,#77030,#77031,
#77032,#77033,#77034,#77035,#77036,#77037,#77038,#77039,#77040,#77041,#77042,
#77043,#77044,#77045,#77046,#77047,#77048,#77049,#77050,#77051,#77052,#77053,
#77054,#77055,#77056,#77057,#77058,#77059,#77060,#77061,#77062,#77063,#77064,
#77065,#77066,#77067,#77068,#77069,#77070,#77071,#77072,#77073,#77074,#77075,
#77076,#77077,#77078,#77079,#77080,#77081,#77082,#77083,#77084,#77085,#77086,
#77087,#77088,#77089,#77090,#77091,#77092,#77093,#77094,#77095,#77096,#77097,
#77098,#77099,#77100,#77101,#77102,#77103,#77104,#77105,#77106,#77107,#77108,
#77109,#77110,#77111,#77112,#77113,#77114,#77115,#77116,#77117,#77118,#77119,
#77120,#77121,#77122,#77123,#77124,#77125,#77126,#77127,#77128,#77129,#77130,
#77131,#77132,#77133,#77134,#77135),.UNSPECIFIED.,.F.,.F.,(4,2,2,2,2,2,
2,2,2,2,2,2,2,2,2,2,2,2,2,2,2,2,2,2,2,2,2,2,2,2,2,2,2,2,2,2,2,2,2,2,2,2,
2,2,2,2,2,2,2,2,2,2,2,2,2,2,2,2,2,4),(-8.57349042528258,-8.50240203114283,
-8.44311233837328,-8.32177381469027,-8.26494522658923,-8.18808157627475,
-8.09860869091554,-8.02479679024485,-7.95606253684597,-7.91037569565218,
-7.83563020571102,-7.74246179007927,-7.62144835948341,-7.5644236567328,
-7.48739142584248,-7.39800775582466,-7.32415808945513,-7.255568507469,-7.20984296726339,
-7.13498747216309,-7.04250844937971,-6.9192083019533,-6.86355308775394,
-6.78775701139477,-6.70050107791662,-6.62925888618261,-6.55243899098011,
-6.53113648448967,-6.49290220350523,-6.40998705866415,-6.33381030377695,
-6.24537862779375,-6.17187471117095,-6.1290007426219,-6.04156739607458,
-6.0099834571062,-5.94349244325072,-5.85577273817698,-5.80927108606505,
-5.73226979830522,-5.64224811960476,-5.51616143268776,-5.4620834394515,
-5.38788160507939,-5.32056152450713,-5.29050788914231,-5.16974614834047,
-5.11256874790466,-5.03540705044408,-4.94609198457278,-4.80362475543783,
-4.75787902692566,-4.68296669317975,-4.59075784987658,-4.46663687636836,
-4.41145636881902,-4.3956249802366,-4.30333527342906,-4.22974040858213,
-4.16167874312325),.UNSPECIFIED.);
#625=B_SPLINE_CURVE_WITH_KNOTS('',3,(#77137,#77138,#77139,#77140,#77141,
#77142,#77143,#77144,#77145,#77146,#77147,#77148,#77149,#77150,#77151,#77152),
 .UNSPECIFIED.,.F.,.F.,(4,3,3,3,3,4),(-23.0583686585911,-22.9779671089007,
-22.9477813532571,-22.8663024476233,-22.7844569116864,-22.7026113757494),
 .UNSPECIFIED.);
#626=B_SPLINE_CURVE_WITH_KNOTS('',3,(#77153,#77154,#77155,#77156,#77157,
#77158,#77159,#77160,#77161,#77162,#77163,#77164,#77165,#77166,#77167,#77168),
 .UNSPECIFIED.,.F.,.F.,(4,1,1,1,1,1,1,1,1,1,1,1,1,4),(-22.7026113757494,
-22.4489165412298,-21.9500517292025,-21.4511869171751,-20.9523221051478,
-20.4534572931205,-19.9545924810932,-19.4557276690658,-18.9568628570385,
-18.4579980450112,-17.9591332329838,-17.4602684209565,-16.9614036089292,
-16.7751485430145),.UNSPECIFIED.);
#627=B_SPLINE_CURVE_WITH_KNOTS('',3,(#77174,#77175,#77176,#77177,#77178,
#77179,#77180,#77181,#77182,#77183,#77184,#77185,#77186,#77187,#77188,#77189,
#77190,#77191,#77192,#77193,#77194,#77195,#77196,#77197,#77198,#77199,#77200,
#77201,#77202,#77203,#77204,#77205,#77206,#77207,#77208,#77209,#77210,#77211,
#77212,#77213,#77214,#77215,#77216,#77217,#77218,#77219,#77220,#77221,#77222,
#77223,#77224,#77225,#77226,#77227,#77228,#77229,#77230,#77231,#77232,#77233,
#77234,#77235,#77236,#77237,#77238,#77239,#77240,#77241,#77242,#77243,#77244,
#77245,#77246,#77247,#77248,#77249,#77250,#77251,#77252,#77253,#77254,#77255,
#77256,#77257,#77258,#77259,#77260,#77261,#77262,#77263,#77264,#77265,#77266,
#77267,#77268,#77269,#77270,#77271,#77272,#77273,#77274,#77275,#77276,#77277,
#77278,#77279,#77280,#77281,#77282,#77283,#77284,#77285,#77286,#77287),
 .UNSPECIFIED.,.F.,.F.,(4,2,2,2,2,2,2,2,2,2,2,2,2,2,2,2,2,2,2,2,2,2,2,2,
2,2,2,2,2,2,2,2,2,2,2,2,2,2,2,2,2,2,2,2,2,2,2,2,2,2,2,2,2,2,2,2,4),(-4.16151590151851,
-4.0760948985585,-4.00123840793195,-3.95551321653237,-3.88694412086877,
-3.8130973004708,-3.72373618742032,-3.64669644708721,-3.58965455941888,
-3.46868919783547,-3.40940726048669,-3.32975477505438,-3.2874224169687,
-3.2696219553045,-3.2164269161219,-3.12595598025145,-3.04968479711686,-2.966724037557,
-2.92852260043549,-2.83575016541184,-2.76216092585789,-2.67221648331477,
-2.59631384592066,-2.54053874000987,-2.4174649850203,-2.38741627088776,
-2.35304615139757,-2.27134755770366,-2.23209950901699,-2.19345460782918,
-2.06595660720629,-1.97365271457811,-1.89516962604998,-1.83631426962606,
-1.71822474841647,-1.62467705543961,-1.54955199322482,-1.5037315584742,
-1.36190743973524,-1.27367653035868,-1.19947794667645,-1.15398541021193,
-1.08477368485643,-1.01105839226976,-0.92140554879589,-0.844936999934219,
-0.788546545693046,-0.666510947040339,-0.57375356441514,-0.498854038590726,
-0.45311362129568,-0.369065778336818,-0.301465506272486,-0.240428505417184,
-0.145854057242879,-0.113723193842431,-6.03189471992543E-5),
 .UNSPECIFIED.);
#628=B_SPLINE_CURVE_WITH_KNOTS('',3,(#77288,#77289,#77290,#77291,#77292,
#77293,#77294,#77295,#77296,#77297),.UNSPECIFIED.,.F.,.F.,(4,2,2,2,4),(-8.82332564681183,
-8.77464235640149,-8.64341940293209,-8.60415258924592,-8.57349042528258),
 .UNSPECIFIED.);
#629=B_SPLINE_CURVE_WITH_KNOTS('',3,(#77299,#77300,#77301,#77302,#77303),
 .UNSPECIFIED.,.F.,.F.,(4,1,4),(-16.7751485430145,-16.4625387969019,-16.4194260685698),
 .UNSPECIFIED.);
#630=B_SPLINE_CURVE_WITH_KNOTS('',3,(#77304,#77305,#77306,#77307,#77308,
#77309,#77310,#77311,#77312,#77313,#77314,#77315,#77316,#77317,#77318,#77319,
#77320,#77321,#77322,#77323,#77324,#77325,#77326,#77327,#77328,#77329,#77330,
#77331,#77332,#77333,#77334,#77335,#77336,#77337,#77338,#77339,#77340,#77341,
#77342,#77343,#77344,#77345,#77346,#77347,#77348,#77349,#77350,#77351,#77352,
#77353,#77354,#77355,#77356,#77357,#77358,#77359,#77360,#77361,#77362,#77363,
#77364,#77365,#77366,#77367,#77368,#77369,#77370,#77371,#77372,#77373,#77374,
#77375,#77376,#77377,#77378,#77379,#77380,#77381,#77382,#77383,#77384,#77385,
#77386,#77387,#77388,#77389,#77390,#77391,#77392,#77393,#77394,#77395,#77396,
#77397,#77398,#77399,#77400,#77401,#77402,#77403,#77404,#77405,#77406,#77407,
#77408,#77409,#77410,#77411,#77412,#77413,#77414,#77415,#77416,#77417,#77418,
#77419,#77420,#77421,#77422,#77423,#77424,#77425,#77426,#77427,#77428,#77429,
#77430,#77431,#77432,#77433,#77434,#77435,#77436,#77437,#77438,#77439,#77440,
#77441,#77442,#77443,#77444,#77445,#77446,#77447,#77448,#77449,#77450,#77451,
#77452,#77453,#77454,#77455,#77456,#77457,#77458,#77459,#77460,#77461,#77462,
#77463,#77464,#77465,#77466,#77467,#77468,#77469,#77470,#77471,#77472,#77473,
#77474,#77475,#77476,#77477,#77478,#77479,#77480,#77481,#77482,#77483,#77484,
#77485,#77486,#77487,#77488,#77489,#77490,#77491,#77492,#77493,#77494,#77495,
#77496,#77497,#77498,#77499,#77500,#77501,#77502,#77503,#77504,#77505,#77506,
#77507,#77508,#77509,#77510,#77511,#77512,#77513,#77514,#77515,#77516,#77517,
#77518,#77519,#77520,#77521,#77522,#77523,#77524,#77525,#77526,#77527,#77528,
#77529,#77530,#77531,#77532,#77533,#77534,#77535,#77536,#77537,#77538,#77539,
#77540,#77541,#77542,#77543,#77544,#77545,#77546,#77547,#77548,#77549,#77550),
 .UNSPECIFIED.,.F.,.F.,(4,3,3,3,3,3,3,3,3,3,3,3,3,3,3,3,3,3,3,3,3,3,3,3,
3,3,3,3,3,3,3,3,3,3,3,3,3,3,3,3,3,3,3,3,3,3,3,3,3,3,3,3,3,3,3,3,3,3,3,3,
3,3,3,3,3,3,3,3,3,3,3,3,3,3,3,3,3,3,3,3,3,3,4),(-16.4194260628912,-16.3392758127687,
-16.259140303397,-16.1790020076008,-16.0988669317824,-16.0187124343916,
-15.9636739848745,-15.8832718887138,-15.8028850567879,-15.7183660858027,
-15.6379818518158,-15.5575968137742,-15.4771955107962,-15.4648091728472,
-15.3844070766868,-15.3040202447606,-15.2195012737754,-15.1391170397884,
-15.0587320017468,-14.9783306987688,-14.9659443608199,-14.8855422646602,
-14.8051554327346,-14.7206364617491,-14.640252227763,-14.5598671897221,
-14.4794658867447,-14.4670795487925,-14.3866774526294,-14.3062906207008,
-14.2217716497169,-14.1413874157274,-14.0610023776838,-13.9806010747033,
-13.9682147367652,-13.8878126406106,-13.8074258086903,-13.7229068377022,
-13.6425226037211,-13.5621375656852,-13.4817362627123,-13.4693499247379,
-13.3889478285678,-13.3085609966321,-13.2240420256517,-13.1436577916554,
-13.0632727536049,-12.9828714506176,-12.9704851127106,-12.890083016561,
-12.8096961846458,-12.7251772136551,-12.6447929796791,-12.5644079416484,
-12.4840066386806,-12.4716203006832,-12.391218204522,-12.3108313725956,
-12.2263124016107,-12.1459281676232,-12.065543129581,-11.9851418266027,
-11.9727554886559,-11.8923533924557,-11.8119665604902,-11.7274475895248,
-11.647063355498,-11.5666783174163,-11.4862770143991,-11.4738906766286,
-11.3934885806086,-11.3131017488229,-11.2285827777675,-11.1481985439209,
-11.0678135060188,-10.9874122031781,-10.9750258646012,-10.8946239524111,
-10.8142373647188,-10.7336745609209,-10.6532917024683,-10.5726389259978,
-10.4919861495273),.UNSPECIFIED.);
#631=B_SPLINE_CURVE_WITH_KNOTS('',3,(#77556,#77557,#77558,#77559,#77560,
#77561,#77562,#77563,#77564,#77565,#77566,#77567,#77568,#77569,#77570,#77571,
#77572,#77573,#77574,#77575,#77576,#77577,#77578,#77579,#77580,#77581,#77582,
#77583,#77584,#77585,#77586,#77587,#77588,#77589,#77590,#77591,#77592,#77593,
#77594,#77595,#77596,#77597,#77598,#77599,#77600,#77601,#77602,#77603,#77604,
#77605,#77606,#77607,#77608,#77609,#77610,#77611,#77612,#77613,#77614,#77615,
#77616,#77617,#77618,#77619,#77620,#77621,#77622,#77623,#77624,#77625,#77626,
#77627,#77628,#77629,#77630,#77631,#77632,#77633),.UNSPECIFIED.,.F.,.F.,
(4,2,2,2,2,2,2,2,2,2,2,2,2,2,2,2,2,2,2,2,2,2,2,2,2,2,2,2,2,2,2,2,2,2,2,
2,2,2,4),(5.98638844770362E-5,0.112872266003416,0.17427999276801,0.26938684905027,
0.322521957986195,0.353461345058414,0.432508794039687,0.525454262701712,
0.642595895792396,0.701573004104969,0.778521202305748,0.86855015668362,
1.00913121847656,1.05572572809319,1.13026329894176,1.22281910204197,1.3487438846434,
1.40270123548857,1.47894075605843,1.568867084826,1.70711663583873,1.75540521681487,
1.83515681926088,1.92042700563513,2.05966626718135,2.10632096964438,2.17059611351698,
2.24074969883762,2.27086609193784,2.40513588310623,2.45508146207408,2.52395462171003,
2.59276459723876,2.62283023188887,2.7517686900946,2.789975913623,2.82944959587034,
2.91095381420802,2.95510205588621),.UNSPECIFIED.);
#632=B_SPLINE_CURVE_WITH_KNOTS('',3,(#77637,#77638,#77639,#77640,#77641,
#77642,#77643,#77644,#77645,#77646,#77647,#77648,#77649,#77650,#77651,#77652,
#77653,#77654,#77655,#77656,#77657,#77658,#77659,#77660,#77661,#77662,#77663,
#77664,#77665,#77666,#77667,#77668,#77669,#77670,#77671,#77672,#77673,#77674,
#77675,#77676,#77677,#77678,#77679,#77680,#77681,#77682,#77683,#77684,#77685,
#77686,#77687,#77688,#77689,#77690,#77691,#77692,#77693,#77694,#77695,#77696,
#77697,#77698,#77699,#77700,#77701,#77702,#77703,#77704,#77705,#77706,#77707,
#77708,#77709,#77710,#77711,#77712,#77713,#77714,#77715,#77716,#77717,#77718,
#77719,#77720,#77721,#77722,#77723,#77724,#77725,#77726,#77727,#77728,#77729,
#77730,#77731,#77732,#77733,#77734,#77735,#77736,#77737,#77738,#77739,#77740,
#77741,#77742,#77743,#77744,#77745,#77746,#77747,#77748,#77749,#77750,#77751,
#77752,#77753,#77754,#77755,#77756,#77757,#77758,#77759,#77760,#77761,#77762,
#77763,#77764,#77765,#77766,#77767,#77768,#77769,#77770,#77771,#77772,#77773,
#77774,#77775,#77776,#77777,#77778,#77779,#77780,#77781,#77782,#77783,#77784,
#77785,#77786,#77787,#77788,#77789,#77790,#77791,#77792,#77793,#77794,#77795,
#77796,#77797,#77798,#77799,#77800,#77801,#77802,#77803,#77804,#77805,#77806,
#77807,#77808,#77809,#77810,#77811,#77812,#77813,#77814,#77815,#77816,#77817,
#77818,#77819,#77820,#77821,#77822,#77823,#77824,#77825,#77826,#77827,#77828,
#77829,#77830,#77831,#77832,#77833,#77834,#77835,#77836,#77837,#77838,#77839,
#77840,#77841,#77842,#77843,#77844,#77845,#77846,#77847,#77848,#77849,#77850,
#77851,#77852,#77853,#77854,#77855,#77856,#77857,#77858,#77859,#77860,#77861,
#77862,#77863,#77864,#77865,#77866,#77867,#77868,#77869,#77870,#77871),
 .UNSPECIFIED.,.F.,.F.,(4,3,3,3,3,3,3,3,3,3,3,3,3,3,3,3,3,3,3,3,3,3,3,3,
3,3,3,3,3,3,3,3,3,3,3,3,3,3,3,3,3,3,3,3,3,3,3,3,3,3,3,3,3,3,3,3,3,3,3,3,
3,3,3,3,3,3,3,3,3,3,3,3,3,3,3,3,3,3,4),(2.02057256326897,2.10082259985238,
2.1810574358235,2.26129496682187,2.34152807110776,2.4217816632337,2.49432406013665,
2.57472542136099,2.65511153505957,2.73963086933567,2.82001443873895,2.90039883353079,
2.98079952696405,2.99318887216398,3.07358729627662,3.15397039737693,3.23849121908052,
3.3188716377365,3.39925284699051,3.47965032437132,3.4920536841913,3.57245925188446,
3.6528496035864,3.73736682674446,3.8177546421867,3.89814326818861,3.97854814754071,
3.99091849621863,4.071318441516,4.15170309472865,4.23622314810798,4.31660517019189,
4.39698799400358,4.47738709226745,4.48978330824596,4.57018642790357,4.65057429574128,
4.73509275187428,4.81547803548217,4.89586412354026,4.97626647102544,4.98864812027329,
5.06904985871735,5.14943632904741,5.23395547986071,5.31433934859764,5.39472402163805,
5.47512496207277,5.48751293230062,5.56791508317406,5.64830197006663,5.73282091363196,
5.81320520230256,5.89359029470323,5.97399165126986,5.98637774432795,6.06677988419513,
6.14716676060536,6.23168570954284,6.3120699892127,6.39245507316294,6.4728564221019,
6.48524255635528,6.56564459930079,6.64603137725135,6.73055037503416,6.81093455404784,
6.89131953699836,6.97172078503834,6.98410736838261,7.06450950077892,7.14489636941888,
7.22941532216664,7.30979959344878,7.39018466883242,7.47058600900235,7.48297218040994,
7.56803809318229,7.59229499831558),.UNSPECIFIED.);
#633=B_SPLINE_CURVE_WITH_KNOTS('',3,(#77872,#77873,#77874,#77875,#77876,
#77877,#77878,#77879,#77880,#77881),.UNSPECIFIED.,.F.,.F.,(4,2,2,2,4),(-8.82240336587914,
-8.75464221200688,-8.71131988181848,-8.5760612850891,-8.57259242800733),
 .UNSPECIFIED.);
#634=B_SPLINE_CURVE_WITH_KNOTS('',3,(#77883,#77884,#77885,#77886,#77887,
#77888,#77889,#77890,#77891,#77892,#77893,#77894,#77895,#77896,#77897,#77898,
#77899,#77900,#77901,#77902,#77903,#77904,#77905,#77906,#77907,#77908,#77909,
#77910,#77911,#77912,#77913,#77914,#77915,#77916,#77917,#77918,#77919,#77920,
#77921,#77922,#77923,#77924,#77925,#77926,#77927,#77928,#77929,#77930,#77931,
#77932,#77933,#77934,#77935,#77936,#77937,#77938,#77939,#77940,#77941,#77942,
#77943,#77944,#77945,#77946,#77947,#77948,#77949,#77950,#77951,#77952,#77953,
#77954,#77955,#77956,#77957,#77958,#77959,#77960,#77961,#77962,#77963,#77964,
#77965,#77966,#77967,#77968,#77969,#77970,#77971,#77972,#77973,#77974,#77975,
#77976,#77977,#77978,#77979,#77980,#77981,#77982,#77983,#77984,#77985,#77986,
#77987,#77988,#77989,#77990,#77991,#77992,#77993,#77994,#77995,#77996,#77997,
#77998,#77999,#78000,#78001,#78002,#78003,#78004),.UNSPECIFIED.,.F.,.F.,
(4,2,2,2,2,2,2,2,2,2,2,2,2,2,2,2,2,2,2,2,2,2,2,2,2,2,2,2,2,2,2,2,2,2,2,
2,2,2,2,2,2,2,2,2,2,2,2,2,2,2,2,2,2,2,2,2,2,2,2,2,4),(-8.57259242800733,
-8.53729965094587,-8.43520820880102,-8.37593118628754,-8.25380929012716,
-8.19747433468778,-8.12105231428395,-8.03137279657271,-7.95767040886687,
-7.88831042464076,-7.8428969754146,-7.76891951015125,-7.67588154933796,
-7.55225135353314,-7.49680633626482,-7.42121497421589,-7.33369877963596,
-7.26237150015515,-7.18572502564829,-7.16444605238263,-7.12621153300411,
-7.04331970134402,-6.96717415540716,-6.88292187172238,-6.80598449312008,
-6.76381982603942,-6.6840742636716,-6.62479665950097,-6.50284700212666,
-6.44640880715542,-6.36989366829346,-6.28026205719654,-6.20653855628664,
-6.13747365600876,-6.09190808188494,-6.01749692196664,-5.92495083604497,
-5.80074844958054,-5.76104140745546,-5.7222491520745,-5.64011050399418,
-5.58055857778821,-5.50752992928515,-5.4149653039514,-5.3768796683347,-5.29357358862069,
-5.21665981691337,-5.11823587924998,-5.04848179424069,-4.94719446510772,
-4.86795408371006,-4.79510534412133,-4.71155856194044,-4.67307790121227,
-4.58820042118712,-4.51396150418326,-4.41127049403132,-4.34748944243495,
-4.29183640423953,-4.1685528105975,-4.16151590151851),.UNSPECIFIED.);
#635=B_SPLINE_CURVE_WITH_KNOTS('',3,(#78006,#78007,#78008,#78009,#78010,
#78011,#78012,#78013,#78014,#78015,#78016,#78017,#78018,#78019,#78020,#78021,
#78022,#78023,#78024),.UNSPECIFIED.,.F.,.F.,(4,3,3,3,3,3,4),(-10.4919861495273,
-10.4761610525739,-10.3958161762845,-10.3154846813862,-10.2351643727366,
-10.1548434234609,-10.1362407613902),.UNSPECIFIED.);
#636=B_SPLINE_CURVE_WITH_KNOTS('',3,(#78025,#78026,#78027,#78028,#78029,
#78030,#78031,#78032,#78033,#78034,#78035,#78036,#78037,#78038,#78039,#78040,
#78041,#78042,#78043,#78044,#78045,#78046,#78047,#78048,#78049,#78050,#78051,
#78052,#78053,#78054,#78055,#78056,#78057,#78058,#78059,#78060,#78061,#78062,
#78063,#78064,#78065,#78066,#78067,#78068,#78069,#78070,#78071,#78072,#78073,
#78074,#78075,#78076,#78077,#78078,#78079,#78080,#78081,#78082,#78083,#78084,
#78085,#78086,#78087,#78088,#78089,#78090,#78091,#78092,#78093,#78094,#78095,
#78096,#78097,#78098,#78099,#78100,#78101,#78102,#78103,#78104,#78105,#78106,
#78107,#78108,#78109,#78110,#78111,#78112,#78113,#78114,#78115,#78116,#78117,
#78118,#78119,#78120,#78121,#78122,#78123,#78124,#78125,#78126,#78127,#78128,
#78129,#78130,#78131,#78132,#78133,#78134,#78135,#78136,#78137,#78138,#78139,
#78140,#78141,#78142),.UNSPECIFIED.,.F.,.F.,(4,2,2,2,2,2,2,2,2,2,2,2,2,
2,2,2,2,2,2,2,2,2,2,2,2,2,2,2,2,2,2,2,2,2,2,2,2,2,2,2,2,2,2,2,2,2,2,2,2,
2,2,2,2,2,2,2,2,2,4),(2.95510205588621,2.97035363036219,3.10736320582023,
3.15609175226186,3.22339274075777,3.29265531967367,3.32273466702341,3.45362622282612,
3.50519056950469,3.55844947430104,3.67978864312186,3.73906508705386,3.81875203655083,
3.86102586139961,3.87884392100704,3.93214053233551,4.02242288404177,4.09868923957733,
4.1816464942187,4.21985009140902,4.31262834795997,4.38621338445752,4.47615734771452,
4.55206305528035,4.6078319546552,4.73090708109962,4.76095566059319,4.79532696224168,
4.87702784019752,4.91627446572275,4.95491957120443,5.08240563930163,5.17462078794299,
5.25322582800885,5.31224286836276,5.43007617379252,5.5273886842897,5.60261488919278,
5.65768693245673,5.78196344984821,5.81201248750418,5.88290559383789,5.95079825585252,
5.99991511847723,6.1360309526222,6.1661595287973,6.23675661414532,6.29956647113604,
6.34583513868145,6.48478600973137,6.51486821003581,6.5843340908246,6.65092249030151,
6.69922257791544,6.79604535805604,6.86019450396185,6.96870586689564,7.00937776730152,
7.11659720232867),.UNSPECIFIED.);
#637=B_SPLINE_CURVE_WITH_KNOTS('',3,(#78145,#78146,#78147,#78148,#78149,
#78150,#78151,#78152,#78153,#78154,#78155,#78156),.UNSPECIFIED.,.F.,.F.,
(4,1,1,1,1,1,1,1,1,4),(17.9333477466581,18.3401503700936,18.8390151821209,
19.3378799941482,19.8367448061755,20.3356096182029,20.8344744302302,21.3333392422575,
21.8322040542849,21.9911485751285),.UNSPECIFIED.);
#638=B_SPLINE_CURVE_WITH_KNOTS('',3,(#78157,#78158,#78159,#78160,#78161,
#78162,#78163,#78164),.UNSPECIFIED.,.F.,.F.,(4,1,1,1,1,4),(21.9911485751285,
22.3310688663122,22.8299336783395,23.3287984903668,23.8276633023942,24.2164828558523),
 .UNSPECIFIED.);
#639=B_SPLINE_CURVE_WITH_KNOTS('',3,(#78166,#78167,#78168,#78169,#78170,
#78171,#78172,#78173,#78174,#78175,#78176,#78177,#78178,#78179,#78180,#78181,
#78182,#78183,#78184,#78185,#78186,#78187,#78188,#78189,#78190,#78191,#78192,
#78193,#78194,#78195,#78196,#78197,#78198,#78199,#78200,#78201,#78202,#78203,
#78204,#78205,#78206,#78207,#78208,#78209,#78210,#78211,#78212,#78213,#78214,
#78215,#78216,#78217,#78218,#78219,#78220,#78221,#78222,#78223,#78224,#78225,
#78226,#78227,#78228,#78229,#78230,#78231,#78232,#78233,#78234,#78235,#78236,
#78237,#78238,#78239,#78240,#78241,#78242,#78243,#78244,#78245,#78246,#78247,
#78248,#78249,#78250,#78251,#78252,#78253,#78254,#78255,#78256,#78257,#78258,
#78259),.UNSPECIFIED.,.F.,.F.,(4,3,3,3,3,3,3,3,3,3,3,3,3,3,3,3,3,3,3,3,
3,3,3,3,3,3,3,3,3,3,3,4),(21.9911485751285,22.068343866769,22.1464305423893,
22.2236230042503,22.3021567867503,22.3806905692502,22.4581826086602,22.5356603640975,
22.6131294154855,22.6906046742007,22.7680796462036,22.8455711833453,22.8795553812775,
22.9570474121103,23.0345251588809,23.1119942015404,23.1894694515018,23.2669444147519,
23.3444359431996,23.3784201933048,23.4559122253536,23.5333899733441,23.6108590172257,
23.6883342683997,23.7658092328552,23.8433007624899,23.8772850053322,23.9547763215957,
24.0322561410154,24.1097256822953,24.1871964328171,24.2164947951915),
 .UNSPECIFIED.);
#640=B_SPLINE_CURVE_WITH_KNOTS('',3,(#78260,#78261,#78262,#78263,#78264,
#78265,#78266,#78267,#78268,#78269,#78270,#78271),.UNSPECIFIED.,.F.,.F.,
(4,1,1,1,1,1,1,1,1,4),(17.9333372203403,18.3897720730315,18.8886368850589,
19.3875016970862,19.8863665091135,20.3852313211409,20.8840961331682,21.3829609451955,
21.8818257572228,21.9911485751285),.UNSPECIFIED.);
#641=B_SPLINE_CURVE_WITH_KNOTS('',3,(#78817,#78818,#78819,#78820,#78821,
#78822,#78823,#78824,#78825,#78826,#78827,#78828,#78829,#78830,#78831,#78832,
#78833,#78834,#78835,#78836,#78837,#78838,#78839,#78840,#78841,#78842,#78843,
#78844,#78845,#78846,#78847,#78848,#78849,#78850,#78851,#78852,#78853,#78854,
#78855,#78856,#78857,#78858,#78859,#78860,#78861,#78862,#78863,#78864,#78865,
#78866,#78867,#78868,#78869,#78870,#78871,#78872,#78873,#78874,#78875,#78876,
#78877,#78878,#78879,#78880,#78881,#78882,#78883,#78884,#78885,#78886,#78887,
#78888,#78889,#78890,#78891,#78892,#78893,#78894,#78895,#78896,#78897,#78898,
#78899,#78900,#78901,#78902,#78903,#78904,#78905,#78906,#78907,#78908,#78909,
#78910,#78911,#78912,#78913,#78914,#78915,#78916,#78917,#78918,#78919,#78920,
#78921,#78922,#78923,#78924,#78925),.UNSPECIFIED.,.F.,.F.,(4,3,3,3,3,3,
3,3,3,3,3,3,3,3,3,3,3,3,3,3,3,3,3,3,3,3,3,3,3,3,3,3,3,3,3,3,4),(0.,0.0625522493162699,
0.125874299720649,0.189091179003679,0.251402665927997,0.304861832460781,
0.312371519783548,0.319581198043962,0.381443894429711,0.400771352782656,
0.462797545190397,0.524803898749766,0.586273327225432,0.612528497889583,
0.622823345007737,0.683558995678567,0.743895619283012,0.78830142952157,
0.848926514486215,0.905948440174609,0.913190739602521,0.920001699659024,
0.979766588587133,1.0391809686788,1.09912111202513,1.15906125537146,1.16229775674676,
1.19633653842214,1.2080220062924,1.26652171470092,1.32480529034897,1.36956433288647,
1.37830538556316,1.43585682539719,1.49260862883067,1.52200397117569,1.53973642054051),
 .UNSPECIFIED.);
#642=B_SPLINE_CURVE_WITH_KNOTS('',3,(#78926,#78927,#78928,#78929,#78930,
#78931,#78932,#78933,#78934,#78935,#78936,#78937,#78938,#78939,#78940,#78941,
#78942,#78943,#78944,#78945,#78946,#78947,#78948,#78949,#78950,#78951,#78952,
#78953,#78954,#78955,#78956,#78957,#78958,#78959,#78960,#78961,#78962,#78963,
#78964,#78965,#78966,#78967,#78968,#78969,#78970,#78971,#78972,#78973,#78974,
#78975,#78976,#78977,#78978,#78979,#78980,#78981,#78982,#78983,#78984,#78985,
#78986,#78987,#78988,#78989,#78990,#78991,#78992,#78993,#78994,#78995,#78996,
#78997,#78998,#78999,#79000,#79001,#79002,#79003,#79004,#79005,#79006,#79007,
#79008,#79009,#79010,#79011,#79012,#79013,#79014,#79015,#79016,#79017,#79018,
#79019,#79020,#79021,#79022,#79023,#79024,#79025,#79026,#79027,#79028,#79029,
#79030,#79031,#79032,#79033,#79034),.UNSPECIFIED.,.F.,.F.,(4,3,3,3,3,3,
3,3,3,3,3,3,3,3,3,3,3,3,3,3,3,3,3,3,3,3,3,3,3,3,3,3,3,3,3,3,4),(8.90323594776316E-15,
0.0558396431186415,0.113060832821276,0.170735773687653,0.22842886876104,
0.270961174530826,0.278040176691813,0.336849357119395,0.358599321240352,
0.416882186454614,0.475694476083339,0.534694628727055,0.561661453860504,
0.569038253759618,0.628817425890107,0.689165334561057,0.730812179732138,
0.790964330629484,0.850856995814571,0.860790218443922,0.921184370420933,
0.98262723491039,1.04424837715007,1.10546557987407,1.11637421967215,1.14126170877834,
1.15446357064426,1.16482862059503,1.22654809014449,1.28893143939649,1.32131544761034,
1.33677901974891,1.35296500609063,1.3818151014266,1.44819457339889,1.51457404537117,
1.53495742839389),.UNSPECIFIED.);
#643=B_SPLINE_CURVE_WITH_KNOTS('',3,(#79035,#79036,#79037,#79038),
 .UNSPECIFIED.,.F.,.F.,(4,4),(-0.00103132579068994,0.),.UNSPECIFIED.);
#644=B_SPLINE_CURVE_WITH_KNOTS('',3,(#79571,#79572,#79573,#79574,#79575,
#79576,#79577,#79578,#79579,#79580,#79581,#79582,#79583,#79584,#79585,#79586,
#79587,#79588,#79589,#79590,#79591,#79592,#79593,#79594,#79595,#79596,#79597,
#79598,#79599,#79600,#79601,#79602,#79603,#79604,#79605,#79606,#79607,#79608,
#79609,#79610,#79611,#79612,#79613,#79614,#79615,#79616,#79617,#79618,#79619,
#79620,#79621,#79622,#79623,#79624,#79625,#79626,#79627,#79628,#79629,#79630,
#79631,#79632,#79633,#79634,#79635,#79636,#79637,#79638,#79639,#79640,#79641,
#79642,#79643,#79644,#79645,#79646,#79647,#79648,#79649,#79650,#79651,#79652,
#79653,#79654,#79655,#79656,#79657,#79658,#79659,#79660,#79661,#79662,#79663,
#79664,#79665,#79666,#79667,#79668,#79669,#79670,#79671,#79672,#79673,#79674,
#79675,#79676,#79677,#79678,#79679,#79680,#79681,#79682),.UNSPECIFIED.,
 .F.,.F.,(4,3,3,3,3,3,3,3,3,3,3,3,3,3,3,3,3,3,3,3,3,3,3,3,3,3,3,3,3,3,3,
3,3,3,3,3,3,4),(0.,0.0558126623480815,0.11299849537912,0.170655392453315,
0.228379672699063,0.260934534205675,0.270961389638314,0.278040383899749,
0.336849596436437,0.358599321240349,0.416882127265502,0.475694380857889,
0.534694534057781,0.561660852466186,0.569038190842159,0.628817317058425,
0.689165218184891,0.730812179732113,0.790889891999659,0.831575432958716,
0.850857020400834,0.862299587265291,0.925818245366998,0.987287649254916,
1.05183093446352,1.11300183721899,1.11637421967212,1.15284176874186,1.16300105616543,
1.22467697484842,1.28717878211968,1.33420062353113,1.34388635491295,1.35388326449023,
1.4171375655674,1.48044101623512,1.51457404537113,1.53495742827616),
 .UNSPECIFIED.);
#645=B_SPLINE_CURVE_WITH_KNOTS('',3,(#79683,#79684,#79685,#79686,#79687,
#79688,#79689,#79690,#79691,#79692,#79693,#79694,#79695,#79696,#79697,#79698,
#79699,#79700,#79701,#79702,#79703,#79704,#79705,#79706,#79707,#79708,#79709,
#79710,#79711,#79712,#79713,#79714,#79715,#79716,#79717,#79718,#79719,#79720,
#79721,#79722,#79723,#79724,#79725,#79726,#79727,#79728,#79729,#79730,#79731,
#79732,#79733,#79734,#79735,#79736,#79737,#79738,#79739,#79740,#79741,#79742,
#79743,#79744,#79745,#79746,#79747,#79748,#79749,#79750,#79751,#79752,#79753,
#79754,#79755,#79756,#79757,#79758,#79759,#79760,#79761,#79762,#79763,#79764,
#79765,#79766,#79767,#79768,#79769,#79770,#79771,#79772,#79773,#79774,#79775,
#79776,#79777,#79778,#79779,#79780,#79781,#79782,#79783,#79784,#79785,#79786,
#79787,#79788,#79789,#79790,#79791,#79792,#79793,#79794,#79795,#79796,#79797,
#79798,#79799,#79800,#79801,#79802,#79803),.UNSPECIFIED.,.F.,.F.,(4,3,3,
3,3,3,3,3,3,3,3,3,3,3,3,3,3,3,3,3,3,3,3,3,3,3,3,3,3,3,3,3,3,3,3,3,3,3,3,
3,4),(0.,0.0627294749945631,0.125990888525662,0.189264306022852,0.251655622871188,
0.288934555349053,0.304522706022472,0.312082966773186,0.319531623860181,
0.345855736736584,0.400771352782651,0.462797530992162,0.52480388993571,
0.586273333423623,0.604978113100597,0.616083231103068,0.625115386768979,
0.685851984651888,0.746175682300948,0.788301429521589,0.848926515362853,
0.905948442014449,0.913190741906353,0.936167503816501,0.995683676192635,
1.05501285749589,1.11339979822315,1.15906127253955,1.16229775674677,1.18477939514858,
1.1980518199991,1.20870860039415,1.26720629382776,1.32564380364759,1.35222581692638,
1.37013678512747,1.38085187373706,1.43838931773557,1.49511977718729,1.52200397117572,
1.53973642054053),.UNSPECIFIED.);
#646=B_SPLINE_CURVE_WITH_KNOTS('',3,(#79848,#79849,#79850,#79851,#79852,
#79853),.UNSPECIFIED.,.F.,.F.,(4,1,1,4),(49.3488291411432,49.5892427616085,
50.5821441800112,51.5750455984138),.UNSPECIFIED.);
#647=B_SPLINE_CURVE_WITH_KNOTS('',3,(#79856,#79857,#79858,#79859,#79860,
#79861,#79862,#79863,#79864,#79865,#79866,#79867,#79868,#79869,#79870,#79871,
#79872,#79873,#79874,#79875,#79876,#79877,#79878,#79879,#79880,#79881,#79882,
#79883,#79884,#79885,#79886,#79887,#79888,#79889,#79890,#79891,#79892,#79893,
#79894,#79895,#79896,#79897,#79898,#79899,#79900,#79901,#79902,#79903,#79904,
#79905,#79906,#79907,#79908,#79909,#79910,#79911,#79912,#79913,#79914,#79915,
#79916,#79917,#79918,#79919,#79920,#79921,#79922,#79923,#79924,#79925,#79926,
#79927,#79928,#79929,#79930,#79931,#79932,#79933,#79934,#79935,#79936,#79937,
#79938,#79939,#79940,#79941,#79942,#79943,#79944,#79945,#79946,#79947,#79948,
#79949),.UNSPECIFIED.,.F.,.F.,(4,3,3,3,3,3,3,3,3,3,3,3,3,3,3,3,3,3,3,3,
3,3,3,3,3,3,3,3,3,3,3,4),(49.3502889463907,49.4441975015053,49.5380445228534,
49.6318612588435,49.7256734628368,49.8195068771829,49.913444511682,50.0074415682785,
50.1015879207077,50.1428511894672,50.2372867432903,50.3315945427791,50.4258028696877,
50.5199427300037,50.6140476054246,50.7081429068457,50.8022540299028,50.896462754224,
50.9907255754947,51.0851349132109,51.1357526078699,51.2296146641935,51.3233516059659,
51.4201041343669,51.513680825887,51.6072278995691,51.700771432585,51.7943374920094,
51.888005499378,51.9817348168191,52.0756045098968,52.0973718331741),
 .UNSPECIFIED.);
#648=B_SPLINE_CURVE_WITH_KNOTS('',3,(#79955,#79956,#79957,#79958,#79959,
#79960,#79961,#79962,#79963,#79964,#79965,#79966,#79967,#79968,#79969,#79970,
#79971,#79972,#79973,#79974,#79975,#79976,#79977,#79978,#79979,#79980,#79981,
#79982,#79983,#79984,#79985,#79986,#79987,#79988,#79989,#79990,#79991,#79992,
#79993,#79994,#79995,#79996,#79997,#79998,#79999,#80000,#80001,#80002,#80003,
#80004,#80005,#80006,#80007,#80008,#80009,#80010,#80011,#80012,#80013,#80014,
#80015,#80016,#80017,#80018,#80019,#80020,#80021,#80022,#80023,#80024,#80025,
#80026,#80027,#80028,#80029,#80030,#80031,#80032,#80033,#80034,#80035,#80036,
#80037,#80038,#80039,#80040,#80041,#80042,#80043,#80044,#80045,#80046,#80047,
#80048,#80049,#80050,#80051,#80052,#80053,#80054,#80055,#80056,#80057,#80058,
#80059,#80060,#80061,#80062,#80063,#80064,#80065,#80066,#80067,#80068,#80069,
#80070,#80071,#80072,#80073,#80074,#80075,#80076,#80077,#80078,#80079,#80080,
#80081,#80082,#80083,#80084,#80085,#80086,#80087,#80088,#80089,#80090),
 .UNSPECIFIED.,.F.,.F.,(4,3,3,3,3,3,3,3,3,3,3,3,3,3,3,3,3,3,3,3,3,3,3,3,
3,3,3,3,3,3,3,3,3,3,3,3,3,3,3,3,3,3,3,3,3,4),(43.0667307346193,43.1606648282567,
43.2546046786335,43.3489120717733,43.4429916665771,43.5374129588849,43.6318342511926,
43.7260822914796,43.8202029945269,43.914224891448,44.0081800799522,44.1021014472809,
44.196014628203,44.2899452434255,44.3839769975109,44.4780646004317,44.5723031556115,
44.6247356695953,44.7190190327073,44.8131750079831,44.9072320802411,45.0012221569066,
45.0951782216785,45.1891258678985,45.2830906746415,45.3771559987717,45.4712768690749,
45.5655478938942,45.6176370879979,45.711922765816,45.806081403107,45.9001414759278,
45.9941350390331,46.0880948887982,46.1820466118188,46.2760157806679,46.3700858699236,
46.4642117401044,46.5584880801834,46.6105385064006,46.7087956950124,46.8068761968379,
46.9047435082123,47.0024820457555,47.1000741433132,47.1238898038469),
 .UNSPECIFIED.);
#649=B_SPLINE_CURVE_WITH_KNOTS('',3,(#80091,#80092,#80093,#80094,#80095,
#80096),.UNSPECIFIED.,.F.,.F.,(4,1,1,4),(47.1238910225188,47.6034399248032,
48.5963413432059,49.3488291411432),.UNSPECIFIED.);
#650=B_SPLINE_CURVE_WITH_KNOTS('',3,(#80098,#80099,#80100,#80101,#80102,
#80103,#80104,#80105,#80106,#80107,#80108,#80109,#80110,#80111,#80112,#80113,
#80114,#80115,#80116,#80117,#80118,#80119,#80120,#80121,#80122,#80123,#80124,
#80125,#80126,#80127,#80128,#80129,#80130,#80131,#80132,#80133,#80134,#80135,
#80136,#80137,#80138,#80139,#80140,#80141,#80142,#80143,#80144,#80145,#80146,
#80147,#80148,#80149,#80150,#80151,#80152,#80153,#80154,#80155,#80156,#80157,
#80158,#80159,#80160,#80161,#80162,#80163,#80164,#80165,#80166,#80167,#80168,
#80169,#80170,#80171,#80172,#80173,#80174,#80175,#80176),.UNSPECIFIED.,
 .F.,.F.,(4,3,3,3,3,3,3,3,3,3,3,3,3,3,3,3,3,3,3,3,3,3,3,3,3,3,4),(47.1238898038469,
47.1641469342593,47.2584303658851,47.3525864090342,47.4466435484464,47.5406336909398,
47.634589820696,47.728537530985,47.822502400809,47.9165677861539,48.010688716705,
48.104959799685,48.1570483526619,48.2513343067316,48.3454932219898,48.4395535740984,
48.5335474172898,48.6275075475247,48.7214595510516,48.8154290000951,48.9094993673677,
49.003625514735,49.0979021279899,49.1499497710646,49.2441083896016,49.3381288760954,
49.3502889463907),.UNSPECIFIED.);
#651=B_SPLINE_CURVE_WITH_KNOTS('',3,(#80177,#80178,#80179,#80180,#80181,
#80182,#80183,#80184,#80185,#80186,#80187,#80188,#80189,#80190,#80191,#80192,
#80193,#80194,#80195,#80196,#80197,#80198,#80199,#80200,#80201,#80202,#80203,
#80204,#80205,#80206,#80207,#80208,#80209,#80210,#80211,#80212,#80213,#80214,
#80215,#80216,#80217,#80218,#80219,#80220,#80221,#80222,#80223,#80224,#80225,
#80226,#80227,#80228,#80229,#80230,#80231,#80232,#80233,#80234,#80235,#80236,
#80237,#80238,#80239,#80240,#80241,#80242,#80243,#80244,#80245,#80246,#80247,
#80248,#80249,#80250,#80251,#80252,#80253,#80254,#80255,#80256,#80257,#80258,
#80259,#80260,#80261,#80262,#80263,#80264,#80265,#80266,#80267,#80268,#80269,
#80270,#80271,#80272,#80273,#80274,#80275,#80276,#80277,#80278,#80279,#80280,
#80281,#80282,#80283,#80284,#80285,#80286,#80287,#80288,#80289,#80290,#80291,
#80292,#80293,#80294,#80295,#80296,#80297,#80298,#80299,#80300,#80301,#80302,
#80303,#80304,#80305,#80306,#80307,#80308,#80309,#80310,#80311,#80312,#80313,
#80314,#80315),.UNSPECIFIED.,.F.,.F.,(4,3,3,3,3,3,3,3,3,3,3,3,3,3,3,3,3,
3,3,3,3,3,3,3,3,3,3,3,3,3,3,3,3,3,3,3,3,3,3,3,3,3,3,3,3,3,4),(43.066026510645,
43.1602903327225,43.1925412606487,43.2868033581566,43.3809381432706,43.474974128012,
43.5689433550273,43.6628787250892,43.7568058560264,43.8507503515564,43.9447957961315,
44.0388970021702,44.1331488907006,44.1854426790513,44.2797089639737,44.3738479257847,
44.4678880710968,44.5618614178521,44.6558008808659,44.7497320731119,44.8436805934253,
44.9377299831535,45.0318350950528,45.1260907899365,45.178344097454,45.2726125610302,
45.3667537503311,45.460796168269,45.5547718447446,45.6487136718209,45.7426472593229,
45.8365982029629,45.9306500434892,46.0247576252696,46.1190157953705,46.1712455158566,
46.2648963642522,46.3584203227472,46.4541040078507,46.5474647315296,46.6407947083202,
46.7341202531852,46.8315626407827,46.9250123202102,47.0185242448006,47.1121721912856,
47.1238898035752),.UNSPECIFIED.);
#652=B_SPLINE_CURVE_WITH_KNOTS('',3,(#80321,#80322,#80323,#80324,#80325,
#80326,#80327,#80328),.UNSPECIFIED.,.F.,.F.,(4,1,1,1,1,4),(36.7839151923342,
37.6744257407767,38.6673271591794,39.660228577582,40.6531299959847,40.8407044966673),
 .UNSPECIFIED.);
#653=B_SPLINE_CURVE_WITH_KNOTS('',3,(#80329,#80330,#80331,#80332,#80333,
#80334,#80335,#80336,#80337,#80338,#80339,#80340,#80341,#80342,#80343,#80344,
#80345,#80346,#80347,#80348,#80349,#80350,#80351,#80352,#80353,#80354,#80355,
#80356,#80357,#80358,#80359,#80360,#80361,#80362,#80363,#80364,#80365,#80366,
#80367,#80368,#80369,#80370,#80371,#80372,#80373,#80374,#80375,#80376,#80377,
#80378,#80379,#80380,#80381,#80382,#80383,#80384,#80385,#80386,#80387,#80388,
#80389,#80390,#80391,#80392,#80393,#80394,#80395,#80396,#80397,#80398,#80399,
#80400,#80401,#80402,#80403,#80404),.UNSPECIFIED.,.F.,.F.,(4,3,3,3,3,3,
3,3,3,3,3,3,3,3,3,3,3,3,3,3,3,3,3,3,3,4),(40.8407044966673,40.9334408145624,
41.0260857744486,41.1186819489494,41.2112563620308,41.3038360103078,41.3965054992974,
41.4892224724316,41.5820894658992,41.6460314143873,41.7402976892404,41.8344366411228,
41.9284767766575,42.0224501138978,42.1163895675618,42.2103207506336,42.3042692619587,
42.3983186430323,42.4924237464531,42.5866794332149,42.63893283279,42.7332102399409,
42.8273362432537,42.9213747388378,43.0153461234074,43.0667307346193),
 .UNSPECIFIED.);
#654=B_SPLINE_CURVE_WITH_KNOTS('',3,(#80406,#80407,#80408,#80409,#80410,
#80411,#80412,#80413,#80414,#80415,#80416,#80417,#80418,#80419,#80420,#80421,
#80422,#80423,#80424,#80425,#80426,#80427,#80428,#80429,#80430,#80431,#80432,
#80433,#80434,#80435,#80436,#80437,#80438,#80439,#80440,#80441,#80442,#80443,
#80444,#80445,#80446,#80447,#80448,#80449,#80450,#80451,#80452,#80453,#80454,
#80455,#80456,#80457,#80458,#80459,#80460,#80461,#80462,#80463,#80464,#80465,
#80466,#80467,#80468,#80469,#80470,#80471,#80472,#80473,#80474,#80475,#80476,
#80477,#80478,#80479,#80480,#80481),.UNSPECIFIED.,.F.,.F.,(4,3,3,3,3,3,
3,3,3,3,3,3,3,3,3,3,3,3,3,3,3,3,3,3,3,4),(40.8407044968899,40.9467955495431,
41.0533560438878,41.1605004844307,41.2067384238434,41.3010029060945,41.3951400761373,
41.4891784428115,41.5831500375655,41.6770877656947,41.7710172421922,41.8649640679288,
41.9590118053357,42.0531152864055,42.1473693999084,42.199639842246,42.2939131189821,
42.39042729294,42.4844558453375,42.57842255729,42.6723530801146,42.7707714377472,
42.8647438450981,42.9587494742861,43.0528504703067,43.066026510645),
 .UNSPECIFIED.);
#655=B_SPLINE_CURVE_WITH_KNOTS('',3,(#80482,#80483,#80484,#80485,#80486,
#80487,#80488,#80489,#80490,#80491,#80492,#80493,#80494,#80495,#80496,#80497,
#80498,#80499,#80500,#80501,#80502,#80503,#80504,#80505,#80506,#80507,#80508,
#80509,#80510,#80511,#80512,#80513,#80514,#80515,#80516,#80517,#80518,#80519,
#80520,#80521,#80522,#80523,#80524,#80525,#80526,#80527,#80528,#80529,#80530,
#80531,#80532,#80533,#80534,#80535,#80536,#80537,#80538,#80539,#80540,#80541,
#80542,#80543,#80544,#80545,#80546,#80547,#80548,#80549,#80550,#80551,#80552,
#80553,#80554,#80555,#80556,#80557,#80558,#80559,#80560,#80561,#80562,#80563,
#80564,#80565,#80566,#80567,#80568,#80569,#80570,#80571,#80572,#80573,#80574,
#80575,#80576,#80577,#80578,#80579,#80580,#80581,#80582,#80583,#80584,#80585,
#80586,#80587,#80588,#80589,#80590,#80591,#80592,#80593,#80594,#80595,#80596,
#80597,#80598,#80599,#80600,#80601,#80602,#80603,#80604,#80605,#80606,#80607,
#80608,#80609,#80610,#80611,#80612,#80613,#80614,#80615,#80616,#80617),
 .UNSPECIFIED.,.F.,.F.,(4,3,3,3,3,3,3,3,3,3,3,3,3,3,3,3,3,3,3,3,3,3,3,3,
3,3,3,3,3,3,3,3,3,3,3,3,3,3,3,3,3,3,3,3,3,4),(36.7832060675778,36.8771460542011,
36.9711833912529,37.0652707662042,37.159515690071,37.2351327502328,37.3293970162946,
37.423533972185,37.5175721269988,37.6115435141369,37.7054810373499,37.7994103118647,
37.8933569387886,37.987404483374,38.0815077747294,38.1757617052137,38.2280341686354,
38.3222984827916,38.4164354864537,38.5104736886573,38.6044451224285,38.6983826917895,
38.7923120119137,38.8862586838546,38.980306272289,39.0744096068966,39.1686635792801,
39.2209355870381,39.3152000037845,39.4093371109173,39.5033754173212,39.5973469559382,
39.6912846305034,39.785214056058,39.8791608335229,39.9732085269791,40.0673119664767,
40.1615660425125,40.2138370054407,40.3087260587235,40.4034841190128,40.498136016373,
40.5927004180163,40.6872130009825,40.7817120507751,40.8407044966673),
 .UNSPECIFIED.);
#656=B_SPLINE_CURVE_WITH_KNOTS('',3,(#80623,#80624,#80625,#80626,#80627,
#80628,#80629,#80630,#80631,#80632,#80633,#80634,#80635,#80636,#80637,#80638,
#80639,#80640,#80641,#80642,#80643,#80644,#80645,#80646,#80647,#80648,#80649,
#80650,#80651,#80652,#80653,#80654,#80655,#80656,#80657,#80658,#80659,#80660,
#80661,#80662,#80663,#80664,#80665,#80666,#80667,#80668,#80669,#80670,#80671,
#80672,#80673,#80674,#80675,#80676,#80677,#80678,#80679,#80680,#80681,#80682,
#80683,#80684,#80685,#80686,#80687,#80688,#80689,#80690,#80691,#80692,#80693,
#80694,#80695,#80696,#80697,#80698,#80699,#80700,#80701,#80702,#80703,#80704,
#80705,#80706,#80707,#80708,#80709,#80710,#80711,#80712,#80713,#80714,#80715,
#80716,#80717,#80718,#80719,#80720,#80721,#80722,#80723,#80724,#80725,#80726,
#80727,#80728,#80729,#80730,#80731,#80732,#80733,#80734,#80735,#80736,#80737,
#80738,#80739,#80740,#80741,#80742,#80743,#80744,#80745,#80746,#80747,#80748,
#80749,#80750,#80751,#80752,#80753,#80754,#80755,#80756,#80757,#80758,#80759,
#80760,#80761),.UNSPECIFIED.,.F.,.F.,(4,3,3,3,3,3,3,3,3,3,3,3,3,3,3,3,3,
3,3,3,3,3,3,3,3,3,3,3,3,3,3,3,3,3,3,3,3,3,3,3,3,3,3,3,3,3,4),(30.4995771796439,
30.5936923469732,30.6879535757028,30.7241158119582,30.8183801128246,30.9125171034347,
31.0065552928383,31.1005267142311,31.1944642714788,31.2883935797674,31.382340240163,
31.4763878175595,31.5704911414002,31.6647451035425,31.7170172303608,31.8112815307376,
31.9054185209583,31.999456710072,32.0934281313241,32.1873656885236,32.2812949968564,
32.3752416573885,32.4692892350613,32.5633925592575,32.6576465218765,32.7099186487635,
32.8041829508008,32.8983199426043,32.9923581332224,33.0863295558569,33.1802671143628,
33.2741964239248,33.3681430856079,33.4621906643065,33.5562939894593,33.6505479529175,
33.7028200671661,33.7957345289545,33.8909576115212,33.983639100071,34.0762648437623,
34.1688618579209,34.2660261908126,34.358690879243,34.4513987244999,34.5442184709287,
34.5575191894877),.UNSPECIFIED.);
#657=B_SPLINE_CURVE_WITH_KNOTS('',3,(#80762,#80763,#80764,#80765,#80766,
#80767,#80768),.UNSPECIFIED.,.F.,.F.,(4,1,1,1,4),(34.5575191894877,34.6957214855688,
35.6886229039714,36.6815243223741,36.7839151923342),.UNSPECIFIED.);
#658=B_SPLINE_CURVE_WITH_KNOTS('',3,(#80770,#80771,#80772,#80773,#80774,
#80775,#80776,#80777,#80778,#80779,#80780,#80781,#80782,#80783,#80784,#80785,
#80786,#80787,#80788,#80789,#80790,#80791,#80792,#80793,#80794,#80795,#80796,
#80797,#80798,#80799,#80800,#80801,#80802,#80803,#80804,#80805,#80806,#80807,
#80808,#80809,#80810,#80811,#80812,#80813,#80814,#80815,#80816,#80817,#80818,
#80819,#80820,#80821,#80822,#80823,#80824,#80825,#80826,#80827,#80828,#80829,
#80830,#80831,#80832,#80833,#80834,#80835,#80836,#80837,#80838,#80839,#80840,
#80841,#80842,#80843,#80844,#80845),.UNSPECIFIED.,.F.,.F.,(4,3,3,3,3,3,
3,3,3,3,3,3,3,3,3,3,3,3,3,3,3,3,3,3,3,4),(34.5575191894877,34.6509762726237,
34.7444023855498,34.8378236978267,34.9312663680164,35.024813540936,35.1184210075462,
35.2121773967878,35.2493299134275,35.3435942154267,35.4377312071913,35.5317693977697,
35.6257408203635,35.7196783788279,35.8136076883481,35.907554349989,36.0016019286447,
36.0957052537543,36.1899592171693,36.2422313318301,36.3364903162625,36.4306275703372,
36.5246573126976,36.6186236502166,36.7125643032859,36.7832060675778),
 .UNSPECIFIED.);
#659=B_SPLINE_CURVE_WITH_KNOTS('',3,(#80846,#80847,#80848,#80849,#80850,
#80851,#80852,#80853,#80854,#80855,#80856,#80857,#80858,#80859,#80860,#80861,
#80862,#80863,#80864,#80865,#80866,#80867,#80868,#80869,#80870,#80871,#80872,
#80873,#80874,#80875,#80876,#80877,#80878,#80879,#80880,#80881,#80882,#80883,
#80884,#80885,#80886,#80887,#80888,#80889,#80890,#80891,#80892,#80893,#80894,
#80895,#80896,#80897,#80898,#80899,#80900,#80901,#80902,#80903,#80904,#80905,
#80906,#80907,#80908,#80909,#80910,#80911,#80912,#80913,#80914,#80915,#80916,
#80917,#80918,#80919,#80920,#80921,#80922,#80923,#80924,#80925,#80926,#80927,
#80928,#80929,#80930,#80931,#80932,#80933,#80934,#80935,#80936,#80937,#80938,
#80939,#80940,#80941,#80942,#80943,#80944,#80945,#80946,#80947,#80948,#80949,
#80950,#80951,#80952,#80953,#80954,#80955,#80956,#80957,#80958,#80959,#80960,
#80961,#80962,#80963,#80964,#80965,#80966,#80967,#80968,#80969,#80970,#80971,
#80972,#80973,#80974,#80975,#80976,#80977,#80978,#80979,#80980,#80981),
 .UNSPECIFIED.,.F.,.F.,(4,3,3,3,3,3,3,3,3,3,3,3,3,3,3,3,3,3,3,3,3,3,3,3,
3,3,3,3,3,3,3,3,3,3,3,3,3,3,3,3,3,3,3,3,3,4),(30.5007342570418,30.5978580048887,
30.6918155551803,30.7857475823672,30.8796796947812,30.9736374934577,31.0677006444832,
31.1618270355242,31.2560954931774,31.2777242398169,31.37198855852,31.4661255672314,
31.5601637749738,31.6541352149827,31.748072791011,31.8420021182216,31.9359487976573,
32.0299963941584,32.1240997371679,32.2183537183927,32.2706256582195,32.3648899598653,
32.4590269513488,32.5530651417179,32.6470365642101,32.7409741226399,32.834903432192,
32.9288500939313,33.0228976727864,33.1170009981526,33.2112549619117,33.2635270766222,
33.3577913774699,33.4519283680602,33.5459665574427,33.6399379788128,33.733875536037,
33.8278048443011,33.9217515046713,34.0157990820411,34.1099024058543,34.2041563679683,
34.2564284950248,34.3705294643042,34.483246885964,34.5575191893194),
 .UNSPECIFIED.);
#660=B_SPLINE_CURVE_WITH_KNOTS('',3,(#80987,#80988,#80989,#80990,#80991,
#80992,#80993,#80994,#80995,#80996,#80997,#80998,#80999,#81000,#81001,#81002,
#81003,#81004,#81005,#81006,#81007,#81008,#81009,#81010,#81011,#81012,#81013,
#81014,#81015,#81016,#81017,#81018,#81019,#81020,#81021,#81022,#81023,#81024,
#81025,#81026,#81027,#81028,#81029,#81030,#81031,#81032,#81033,#81034,#81035,
#81036,#81037,#81038,#81039,#81040,#81041,#81042,#81043,#81044,#81045,#81046,
#81047,#81048,#81049,#81050,#81051,#81052,#81053,#81054,#81055,#81056,#81057,
#81058,#81059,#81060,#81061,#81062,#81063,#81064,#81065,#81066,#81067,#81068,
#81069,#81070,#81071,#81072,#81073,#81074,#81075,#81076,#81077,#81078,#81079,
#81080,#81081,#81082,#81083,#81084,#81085,#81086,#81087,#81088,#81089,#81090,
#81091,#81092,#81093,#81094,#81095,#81096,#81097,#81098,#81099,#81100,#81101,
#81102,#81103,#81104,#81105,#81106,#81107,#81108,#81109,#81110,#81111,#81112,
#81113,#81114,#81115,#81116,#81117,#81118,#81119,#81120,#81121,#81122),
 .UNSPECIFIED.,.F.,.F.,(4,3,3,3,3,3,3,3,3,3,3,3,3,3,3,3,3,3,3,3,3,3,3,3,
3,3,3,3,3,3,3,3,3,3,3,3,3,3,3,3,3,3,3,3,3,4),(24.2171287697742,24.3110579972788,
24.4049972141539,24.4990332006161,24.5931183154433,24.6873621161442,24.7667073015423,
24.8609713392762,24.9551080626337,25.0491459810612,25.1431171270508,25.2370544062596,
25.3309834342141,25.4249298123192,25.5189771061484,25.6130801452853,25.7073338237151,
25.7596087199449,25.8538731317554,25.948010234554,26.0420485372264,26.1360200730218,
26.2299577453297,26.3238871691935,26.4178339455366,26.5118816387426,26.605985078483,
26.7002391555322,26.7525101383476,26.8467744489231,26.9409114497427,27.0349496498394,
27.1289210826045,27.2228586516417,27.3167879721236,27.4107346451031,27.5047822356061,
27.598885572868,27.6931395487985,27.7454115567502,27.8431501300116,27.9407221181963,
28.0380986592781,28.1353586621332,28.2324911809566,28.2743338823081),
 .UNSPECIFIED.);
#661=B_SPLINE_CURVE_WITH_KNOTS('',3,(#81123,#81124,#81125,#81126,#81127,
#81128,#81129,#81130,#81131,#81132,#81133,#81134,#81135,#81136,#81137,#81138,
#81139,#81140,#81141,#81142,#81143,#81144,#81145,#81146,#81147,#81148,#81149,
#81150,#81151,#81152,#81153,#81154,#81155,#81156,#81157,#81158,#81159,#81160,
#81161,#81162,#81163,#81164,#81165,#81166,#81167,#81168,#81169,#81170,#81171,
#81172,#81173,#81174,#81175,#81176,#81177,#81178,#81179,#81180,#81181,#81182,
#81183,#81184,#81185,#81186,#81187,#81188,#81189,#81190,#81191,#81192,#81193,
#81194,#81195,#81196,#81197,#81198),.UNSPECIFIED.,.F.,.F.,(4,3,3,3,3,3,
3,3,3,3,3,3,3,3,3,3,3,3,3,3,3,3,3,3,3,4),(28.2743338824719,28.3741025974733,
28.4742017672452,28.5744720132341,28.6750305538962,28.7383129751529,28.8325772935425,
28.9267143019364,29.0207525093578,29.1147239490417,29.2086615247428,29.3025908516243,
29.3965375307294,29.4905851268997,29.5846884695777,29.6789424504733,29.7312143935555,
29.8272597418166,29.9213793242568,30.0154088681281,30.1093740916754,30.2069248636675,
30.3008613502571,30.3948068071614,30.4888131270942,30.4995771796439),
 .UNSPECIFIED.);
#662=B_SPLINE_CURVE_WITH_KNOTS('',3,(#81200,#81201,#81202,#81203,#81204,
#81205,#81206,#81207,#81208,#81209,#81210,#81211,#81212,#81213,#81214,#81215,
#81216,#81217,#81218,#81219,#81220,#81221,#81222,#81223,#81224,#81225,#81226,
#81227,#81228,#81229,#81230,#81231,#81232,#81233,#81234,#81235,#81236,#81237,
#81238,#81239,#81240,#81241,#81242,#81243,#81244,#81245,#81246,#81247,#81248,
#81249,#81250,#81251,#81252,#81253,#81254,#81255,#81256,#81257,#81258,#81259,
#81260,#81261,#81262,#81263,#81264,#81265,#81266,#81267,#81268,#81269,#81270,
#81271,#81272,#81273,#81274,#81275,#81276,#81277,#81278),.UNSPECIFIED.,
 .F.,.F.,(4,3,3,3,3,3,3,3,3,3,3,3,3,3,3,3,3,3,3,3,3,3,3,3,3,3,4),(28.2743338823081,
28.299019984609,28.3932843983051,28.4874215030106,28.5814598076082,28.675431345349,
28.7693690196139,28.8632984454436,28.9572452237596,29.0512929189365,29.1453963606499,
29.2396504396559,29.2919214030116,29.386185713534,29.4803227143046,29.5743609143565,
29.6683323470838,29.7622699160872,29.8561992365394,29.9501459094934,30.0441934999777,
30.138296837225,30.2325508131468,30.2848228214142,30.3790955387993,30.4732292275596,
30.5007342570418),.UNSPECIFIED.);
#663=B_SPLINE_CURVE_WITH_KNOTS('',3,(#81279,#81280,#81281,#81282,#81283,
#81284,#81285,#81286),.UNSPECIFIED.,.F.,.F.,(4,1,1,1,1,4),(24.2163565526082,
24.3274143109984,25.320315729401,26.3132171478037,27.3061185662063,28.2743305212408),
 .UNSPECIFIED.);
#664=B_SPLINE_CURVE_WITH_KNOTS('',3,(#81292,#81293,#81294,#81295,#81296,
#81297,#81298,#81299,#81300,#81301,#81302,#81303,#81304,#81305,#81306,#81307,
#81308,#81309,#81310,#81311,#81312,#81313,#81314,#81315,#81316,#81317,#81318,
#81319,#81320,#81321,#81322,#81323,#81324,#81325,#81326,#81327,#81328,#81329,
#81330,#81331,#81332,#81333,#81334,#81335,#81336,#81337,#81338,#81339,#81340,
#81341,#81342,#81343,#81344,#81345,#81346,#81347,#81348,#81349,#81350,#81351,
#81352,#81353,#81354,#81355,#81356,#81357,#81358,#81359,#81360,#81361,#81362,
#81363,#81364,#81365,#81366,#81367),.UNSPECIFIED.,.F.,.F.,(4,3,3,3,3,3,
3,3,3,3,3,3,3,3,3,3,3,3,3,3,3,3,3,3,3,4),(15.7079632679489,15.8009237578477,
15.893857092563,15.9867898679795,16.0797486734675,16.1728168231926,16.2659501333692,
16.3592325081837,16.3842029637772,16.4785800153725,16.5728296354092,16.6669801677573,
16.7610630054697,16.8551113545885,16.9491506824622,17.0432064416485,17.1373610257028,
17.2315703227792,17.3259275836065,17.3771043821798,17.4715162278345,17.5658095311508,
17.6600005887434,17.7541304460648,17.8482419729085,17.9335626655157),
 .UNSPECIFIED.);
#665=B_SPLINE_CURVE_WITH_KNOTS('',3,(#81369,#81370,#81371,#81372,#81373),
 .UNSPECIFIED.,.F.,.F.,(4,1,4),(14.3984001269719,15.3913015453745,15.7079549076759),
 .UNSPECIFIED.);
#666=B_SPLINE_CURVE_WITH_KNOTS('',3,(#81377,#81378,#81379,#81380,#81381,
#81382,#81383,#81384,#81385,#81386,#81387,#81388,#81389,#81390,#81391,#81392,
#81393,#81394,#81395,#81396,#81397,#81398,#81399,#81400,#81401,#81402,#81403,
#81404,#81405,#81406,#81407,#81408,#81409,#81410,#81411,#81412,#81413,#81414,
#81415,#81416,#81417,#81418,#81419,#81420,#81421,#81422,#81423,#81424,#81425,
#81426,#81427,#81428,#81429,#81430,#81431,#81432,#81433,#81434,#81435,#81436,
#81437,#81438,#81439,#81440),.UNSPECIFIED.,.F.,.F.,(4,3,3,3,3,3,3,3,3,3,
3,3,3,3,3,3,3,3,3,3,3,4),(13.8759339789434,13.969800122518,14.0635399756423,
14.1603091183765,14.2538857926958,14.3474317737851,14.4409731412004,14.5345359634685,
14.6281992027686,14.721922831302,14.8157856207819,14.8376931175158,14.9307866091373,
15.0279336914888,15.1207996479157,15.213612609684,15.306399441868,15.3991869778596,
15.4920484539258,15.5849536355179,15.6779807201868,15.7079632679489),
 .UNSPECIFIED.);
#667=B_SPLINE_CURVE_WITH_KNOTS('',3,(#81441,#81442,#81443,#81444,#81445,
#81446,#81447),.UNSPECIFIED.,.F.,.F.,(4,1,1,1,4),(15.7079632679489,15.8305945359184,
16.8234959543211,17.8163973727237,17.9344169320433),.UNSPECIFIED.);
#668=B_SPLINE_CURVE_WITH_KNOTS('',3,(#81453,#81454,#81455,#81456,#81457,
#81458),.UNSPECIFIED.,.F.,.F.,(4,1,1,4),(49.348829680871,49.5892427616085,
50.5821441800112,51.5750455984138),.UNSPECIFIED.);
#669=B_SPLINE_CURVE_WITH_KNOTS('',3,(#81461,#81462,#81463,#81464,#81465,
#81466,#81467,#81468,#81469,#81470,#81471,#81472,#81473,#81474,#81475,#81476,
#81477,#81478,#81479,#81480,#81481,#81482,#81483,#81484,#81485,#81486,#81487,
#81488,#81489,#81490,#81491,#81492,#81493,#81494,#81495,#81496,#81497,#81498,
#81499,#81500,#81501,#81502,#81503,#81504,#81505,#81506,#81507,#81508,#81509,
#81510,#81511,#81512,#81513,#81514,#81515,#81516,#81517,#81518,#81519,#81520,
#81521,#81522,#81523,#81524,#81525,#81526,#81527,#81528,#81529,#81530,#81531,
#81532,#81533,#81534,#81535,#81536,#81537,#81538,#81539,#81540,#81541,#81542,
#81543,#81544,#81545,#81546,#81547,#81548,#81549,#81550,#81551,#81552,#81553,
#81554),.UNSPECIFIED.,.F.,.F.,(4,3,3,3,3,3,3,3,3,3,3,3,3,3,3,3,3,3,3,3,
3,3,3,3,3,3,3,3,3,3,3,4),(49.3502890643105,49.4441980075936,49.5380454154391,
49.6318625367458,49.7256751244353,49.8195089204159,49.9134469314248,50.0074443620431,
50.1015910816633,50.1428511894672,50.2372865866975,50.3315942311916,50.4258024048822,
50.5199421152025,50.6140468426817,50.7081419983793,50.8022529780978,50.8964615635168,
50.9907242482063,51.0851334542348,51.1357526078699,51.2296137933982,51.3233498604106,
51.4201025481234,51.513678360408,51.6072245547518,51.7007672092646,51.7943323919603,
51.8879995295073,51.9817279801555,52.0755968171824,52.0973713621133),
 .UNSPECIFIED.);
#670=B_SPLINE_CURVE_WITH_KNOTS('',3,(#81560,#81561,#81562,#81563,#81564,
#81565,#81566,#81567,#81568,#81569,#81570,#81571,#81572,#81573,#81574,#81575,
#81576,#81577,#81578,#81579,#81580,#81581,#81582,#81583,#81584,#81585,#81586,
#81587,#81588,#81589,#81590,#81591,#81592,#81593,#81594,#81595,#81596,#81597,
#81598,#81599,#81600,#81601,#81602,#81603,#81604,#81605,#81606,#81607,#81608,
#81609,#81610,#81611,#81612,#81613,#81614,#81615,#81616,#81617,#81618,#81619,
#81620,#81621,#81622,#81623,#81624,#81625,#81626,#81627,#81628,#81629,#81630,
#81631,#81632,#81633,#81634,#81635,#81636,#81637,#81638,#81639,#81640,#81641,
#81642,#81643,#81644,#81645,#81646,#81647,#81648,#81649,#81650,#81651,#81652,
#81653,#81654,#81655,#81656,#81657,#81658,#81659,#81660,#81661,#81662,#81663,
#81664,#81665,#81666,#81667,#81668,#81669,#81670,#81671,#81672,#81673,#81674,
#81675,#81676,#81677,#81678,#81679,#81680,#81681,#81682,#81683,#81684,#81685,
#81686,#81687,#81688,#81689,#81690,#81691,#81692,#81693,#81694,#81695),
 .UNSPECIFIED.,.F.,.F.,(4,3,3,3,3,3,3,3,3,3,3,3,3,3,3,3,3,3,3,3,3,3,3,3,
3,3,3,3,3,3,3,3,3,3,3,3,3,3,3,3,3,3,3,3,3,4),(43.0667308900299,43.1606650120045,
43.2546048907049,43.3489122308268,43.4429918536228,43.5374130524077,43.6318342511926,
43.7260822246237,43.820202860722,43.9142246906894,44.0081798125043,44.102101113331,
44.1960142280177,44.2899447773498,44.3839764664652,44.4780640048411,44.5723024967692,
44.6247356695953,44.7190190673005,44.8131750768461,44.9072321830112,45.0012222929145,
45.0951783904985,45.1891260690686,45.2830909076629,45.3771562627026,45.4712771634273,
45.5655482176145,45.6176370879979,45.7119229052218,45.8060816827838,45.9001418965429,
45.994135600988,46.0880955922864,46.1820474568586,46.2760167671013,46.3700869966516,
46.4642130067074,46.5584894846377,46.6105385064006,46.708795281591,46.8068753700284,
46.9047422712377,47.0024804016383,47.1000720984711,47.1238898038469),
 .UNSPECIFIED.);
#671=B_SPLINE_CURVE_WITH_KNOTS('',3,(#81696,#81697,#81698,#81699,#81700,
#81701),.UNSPECIFIED.,.F.,.F.,(4,1,1,4),(47.1238910227372,47.6034399248032,
48.5963413432059,49.348829680871),.UNSPECIFIED.);
#672=B_SPLINE_CURVE_WITH_KNOTS('',3,(#81703,#81704,#81705,#81706,#81707,
#81708,#81709,#81710,#81711,#81712,#81713,#81714,#81715,#81716,#81717,#81718,
#81719,#81720,#81721,#81722,#81723,#81724,#81725,#81726,#81727,#81728,#81729,
#81730,#81731,#81732,#81733,#81734,#81735,#81736,#81737,#81738,#81739,#81740,
#81741,#81742,#81743,#81744,#81745,#81746,#81747,#81748,#81749,#81750,#81751,
#81752,#81753,#81754,#81755,#81756,#81757,#81758,#81759,#81760,#81761,#81762,
#81763,#81764,#81765,#81766,#81767,#81768,#81769,#81770,#81771,#81772,#81773,
#81774,#81775,#81776,#81777,#81778,#81779,#81780,#81781),.UNSPECIFIED.,
 .F.,.F.,(4,3,3,3,3,3,3,3,3,3,3,3,3,3,3,3,3,3,3,3,3,3,3,3,3,3,4),(47.1238898038469,
47.1641469342593,47.2584303255499,47.3525863287413,47.4466434286191,47.5406335323594,
47.6345896238593,47.728537296431,47.8225021291195,47.9165674784281,48.010688373512,
48.1049594222539,48.1570483526619,48.2513341440243,48.3454928955643,48.439553083177,
48.5335467614017,48.6275067264437,48.721458564756,48.8154278487685,48.9094980522921,
49.0036240363993,49.097900488756,49.1499497710646,49.2441087762897,49.3381296503042,
49.3502890643105),.UNSPECIFIED.);
#673=B_SPLINE_CURVE_WITH_KNOTS('',3,(#81782,#81783,#81784,#81785,#81786,
#81787,#81788,#81789,#81790,#81791,#81792,#81793,#81794,#81795,#81796,#81797,
#81798,#81799,#81800,#81801,#81802,#81803,#81804,#81805,#81806,#81807,#81808,
#81809,#81810,#81811,#81812,#81813,#81814,#81815,#81816,#81817,#81818,#81819,
#81820,#81821,#81822,#81823,#81824,#81825,#81826,#81827,#81828,#81829,#81830,
#81831,#81832,#81833,#81834,#81835,#81836,#81837,#81838,#81839,#81840,#81841,
#81842,#81843,#81844,#81845,#81846,#81847,#81848,#81849,#81850,#81851,#81852,
#81853,#81854,#81855,#81856,#81857,#81858,#81859,#81860,#81861,#81862,#81863,
#81864,#81865,#81866,#81867,#81868,#81869,#81870,#81871,#81872,#81873,#81874,
#81875,#81876,#81877,#81878,#81879,#81880,#81881,#81882,#81883,#81884,#81885,
#81886,#81887,#81888,#81889,#81890,#81891,#81892,#81893,#81894,#81895,#81896,
#81897,#81898,#81899,#81900,#81901,#81902,#81903,#81904,#81905,#81906,#81907,
#81908,#81909,#81910,#81911,#81912,#81913,#81914,#81915,#81916,#81917,#81918,
#81919,#81920),.UNSPECIFIED.,.F.,.F.,(4,3,3,3,3,3,3,3,3,3,3,3,3,3,3,3,3,
3,3,3,3,3,3,3,3,3,3,3,3,3,3,3,3,3,3,3,3,3,3,3,3,3,3,3,3,3,4),(43.0660266561136,
43.1602904721168,43.1925412606487,43.2868033719875,43.3809381709436,43.4749741695202,
43.5689434103037,43.6628787940877,43.7568059386841,43.8507504477941,43.9447959057476,
44.0388971250699,44.1331490266067,44.1854426790513,44.2797089580453,44.3738479140106,
44.4678880535664,44.56186139472,44.6558008522294,44.7497320390745,44.8436805540964,
44.9377299387299,45.0318350456382,45.1260907357409,45.178344097454,45.2726125283646,
45.3667536848057,45.4607960697361,45.5547717131217,45.6487135070695,45.7426470614455,
45.8365979720026,45.9306497797122,46.0247573287788,46.1190154666471,46.1712455158566,
46.2648964418328,46.3584204779971,46.4541041436943,46.5474649448372,46.6407949988889,
46.7341206207388,46.8315629164479,46.9250126715277,47.0185246713068,47.1121726918931,
47.1238898035752),.UNSPECIFIED.);
#674=B_SPLINE_CURVE_WITH_KNOTS('',3,(#81926,#81927,#81928,#81929,#81930,
#81931,#81932,#81933),.UNSPECIFIED.,.F.,.F.,(4,1,1,1,1,4),(36.7839153402381,
37.6744257407767,38.6673271591794,39.660228577582,40.6531299959847,40.8407044966673),
 .UNSPECIFIED.);
#675=B_SPLINE_CURVE_WITH_KNOTS('',3,(#81934,#81935,#81936,#81937,#81938,
#81939,#81940,#81941,#81942,#81943,#81944,#81945,#81946,#81947,#81948,#81949,
#81950,#81951,#81952,#81953,#81954,#81955,#81956,#81957,#81958,#81959,#81960,
#81961,#81962,#81963,#81964,#81965,#81966,#81967,#81968,#81969,#81970,#81971,
#81972,#81973,#81974,#81975,#81976,#81977,#81978,#81979,#81980,#81981,#81982,
#81983,#81984,#81985,#81986,#81987,#81988,#81989,#81990,#81991,#81992,#81993,
#81994,#81995,#81996,#81997,#81998,#81999,#82000,#82001,#82002,#82003,#82004,
#82005,#82006,#82007,#82008,#82009),.UNSPECIFIED.,.F.,.F.,(4,3,3,3,3,3,
3,3,3,3,3,3,3,3,3,3,3,3,3,3,3,3,3,3,3,4),(40.8407044966673,40.9334408037622,
41.0260857529454,41.1186819168029,41.2112563193078,41.3038359570828,41.3965054357324,
41.4892223986014,41.5820893820075,41.6460314143873,41.740297694324,41.8344366512188,
41.9284767916903,42.0224501337347,42.1163895921195,42.2103207798235,42.3042692956868,
42.3983186811306,42.4924237888327,42.5866794796959,42.63893283279,42.7332102678453,
42.8273362992733,42.9213748230855,43.0153462359771,43.0667308900299),
 .UNSPECIFIED.);
#676=B_SPLINE_CURVE_WITH_KNOTS('',3,(#82011,#82012,#82013,#82014,#82015,
#82016,#82017,#82018,#82019,#82020,#82021,#82022,#82023,#82024,#82025,#82026,
#82027,#82028,#82029,#82030,#82031,#82032,#82033,#82034,#82035,#82036,#82037,
#82038,#82039,#82040,#82041,#82042,#82043,#82044,#82045,#82046,#82047,#82048,
#82049,#82050,#82051,#82052,#82053,#82054,#82055,#82056,#82057,#82058,#82059,
#82060,#82061,#82062,#82063,#82064,#82065,#82066,#82067,#82068,#82069,#82070,
#82071,#82072,#82073,#82074,#82075,#82076,#82077,#82078,#82079,#82080,#82081,
#82082,#82083,#82084,#82085,#82086),.UNSPECIFIED.,.F.,.F.,(4,3,3,3,3,3,
3,3,3,3,3,3,3,3,3,3,3,3,3,3,3,3,3,3,3,4),(40.8407044968899,40.9467955512976,
41.0533560472971,41.1605004892804,41.2067384238434,41.3010029055445,41.3951400750534,
41.4891784412107,41.5831500354742,41.6770877631296,41.7710172391702,41.8649640644675,
41.9590118014643,42.0531152821399,42.147369395277,42.199639842246,42.2939131126729,
42.390427305603,42.4844558516208,42.5784225571918,42.6723530736409,42.7707714692591,
42.8647438703345,42.9587494932815,43.0528504831882,43.0660266561136),
 .UNSPECIFIED.);
#677=B_SPLINE_CURVE_WITH_KNOTS('',3,(#82087,#82088,#82089,#82090,#82091,
#82092,#82093,#82094,#82095,#82096,#82097,#82098,#82099,#82100,#82101,#82102,
#82103,#82104,#82105,#82106,#82107,#82108,#82109,#82110,#82111,#82112,#82113,
#82114,#82115,#82116,#82117,#82118,#82119,#82120,#82121,#82122,#82123,#82124,
#82125,#82126,#82127,#82128,#82129,#82130,#82131,#82132,#82133,#82134,#82135,
#82136,#82137,#82138,#82139,#82140,#82141,#82142,#82143,#82144,#82145,#82146,
#82147,#82148,#82149,#82150,#82151,#82152,#82153,#82154,#82155,#82156,#82157,
#82158,#82159,#82160,#82161,#82162,#82163,#82164,#82165,#82166,#82167,#82168,
#82169,#82170,#82171,#82172,#82173,#82174,#82175,#82176,#82177,#82178,#82179,
#82180,#82181,#82182,#82183,#82184,#82185,#82186,#82187,#82188,#82189,#82190,
#82191,#82192,#82193,#82194,#82195,#82196,#82197,#82198,#82199,#82200,#82201,
#82202,#82203,#82204,#82205,#82206,#82207,#82208,#82209,#82210,#82211,#82212,
#82213,#82214,#82215,#82216,#82217,#82218,#82219,#82220,#82221,#82222),
 .UNSPECIFIED.,.F.,.F.,(4,3,3,3,3,3,3,3,3,3,3,3,3,3,3,3,3,3,3,3,3,3,3,3,
3,3,3,3,3,3,3,3,3,3,3,3,3,3,3,3,3,3,3,3,3,4),(36.7832062156987,36.8771462021669,
36.9711835390891,37.0652709139485,37.1595158376815,37.2351327502328,37.3293970166289,
37.4235339728533,37.5175721280006,37.6115435154695,37.7054810390119,37.7994103138541,
37.8933569411026,37.9874044860071,38.0815077776789,38.1757617084725,38.2280341686354,
38.3222984827967,38.4164354864664,38.5104736886812,38.6044451224672,38.6983826918458,
38.7923120119903,38.8862586839539,38.9803062724145,39.0744096070503,39.1686635794652,
39.2209355870381,39.3152000026346,39.4093371086122,39.5033754138575,39.5973469513155,
39.691284624722,39.7852140491199,39.8791608254314,39.9732085177452,40.0673119561054,
40.1615660310226,40.2138370054408,40.3087260615032,40.4034841245682,40.4981360246953,
40.5927004290814,40.6872130147763,40.7817120672609,40.8407044966673),
 .UNSPECIFIED.);
#678=B_SPLINE_CURVE_WITH_KNOTS('',3,(#82228,#82229,#82230,#82231,#82232,
#82233,#82234,#82235,#82236,#82237,#82238,#82239,#82240,#82241,#82242,#82243,
#82244,#82245,#82246,#82247,#82248,#82249,#82250,#82251,#82252,#82253,#82254,
#82255,#82256,#82257,#82258,#82259,#82260,#82261,#82262,#82263,#82264,#82265,
#82266,#82267,#82268,#82269,#82270,#82271,#82272,#82273,#82274,#82275,#82276,
#82277,#82278,#82279,#82280,#82281,#82282,#82283,#82284,#82285,#82286,#82287,
#82288,#82289,#82290,#82291,#82292,#82293,#82294,#82295,#82296,#82297,#82298,
#82299,#82300,#82301,#82302,#82303,#82304,#82305,#82306,#82307,#82308,#82309,
#82310,#82311,#82312,#82313,#82314,#82315,#82316,#82317,#82318,#82319,#82320,
#82321,#82322,#82323,#82324,#82325,#82326,#82327,#82328,#82329,#82330,#82331,
#82332,#82333,#82334,#82335,#82336,#82337,#82338,#82339,#82340,#82341,#82342,
#82343,#82344,#82345,#82346,#82347,#82348,#82349,#82350,#82351,#82352,#82353,
#82354,#82355,#82356,#82357,#82358,#82359,#82360,#82361,#82362,#82363,#82364,
#82365,#82366),.UNSPECIFIED.,.F.,.F.,(4,3,3,3,3,3,3,3,3,3,3,3,3,3,3,3,3,
3,3,3,3,3,3,3,3,3,3,3,3,3,3,3,3,3,3,3,3,3,3,3,3,3,3,3,3,3,4),(30.4995773282354,
30.5936924956574,30.6879537244389,30.7241158119582,30.8183801128151,30.9125171034153,
31.0065552928083,31.1005267141897,31.1944642714255,31.2883935797018,31.3823402400845,
31.4763878174676,31.5704911412944,31.6647451034225,31.7170172303608,31.8112815307233,
31.90541852093,31.9994567100302,32.0934281312696,32.1873656884567,32.2812949967776,
32.3752416572982,32.4692892349602,32.5633925591461,32.6576465217556,32.7099186487635,
32.8041829507817,32.8983199425657,32.9923581331637,33.0863295557777,33.1802671142629,
33.274196423804,33.368143085466,33.462190664143,33.5562939892742,33.6505479527108,
33.7028200671661,33.7957345290918,33.8909576116413,33.9836391003293,34.0762648441589,
34.1688618584558,34.2660261912138,34.3586908797819,34.4513987251761,34.544218471741,
34.5575191894877),.UNSPECIFIED.);
#679=B_SPLINE_CURVE_WITH_KNOTS('',3,(#82367,#82368,#82369,#82370,#82371,
#82372,#82373),.UNSPECIFIED.,.F.,.F.,(4,1,1,1,4),(34.5575191894877,34.6957214855688,
35.6886229039714,36.6815243223741,36.7839153402381),.UNSPECIFIED.);
#680=B_SPLINE_CURVE_WITH_KNOTS('',3,(#82375,#82376,#82377,#82378,#82379,
#82380,#82381,#82382,#82383,#82384,#82385,#82386,#82387,#82388,#82389,#82390,
#82391,#82392,#82393,#82394,#82395,#82396,#82397,#82398,#82399,#82400,#82401,
#82402,#82403,#82404,#82405,#82406,#82407,#82408,#82409,#82410,#82411,#82412,
#82413,#82414,#82415,#82416,#82417,#82418,#82419,#82420,#82421,#82422,#82423,
#82424,#82425,#82426,#82427,#82428,#82429,#82430,#82431,#82432,#82433,#82434,
#82435,#82436,#82437,#82438,#82439,#82440,#82441,#82442,#82443,#82444,#82445,
#82446,#82447,#82448,#82449,#82450),.UNSPECIFIED.,.F.,.F.,(4,3,3,3,3,3,
3,3,3,3,3,3,3,3,3,3,3,3,3,3,3,3,3,3,3,4),(34.5575191894877,34.6509762726285,
34.7444023855589,34.8378236978393,34.9312663680321,35.0248135409537,35.1184210075654,
35.2121773968077,35.2493299134275,35.3435942154491,35.4377312072367,35.5317693978386,
35.6257408204563,35.7196783789453,35.8136076884902,35.9075543501558,36.0016019288369,
36.0957052539719,36.1899592174124,36.2422313318302,36.3364903160518,36.4306275699184,
36.5246573120852,36.618623649412,36.7125643023337,36.7832062156987),
 .UNSPECIFIED.);
#681=B_SPLINE_CURVE_WITH_KNOTS('',3,(#82451,#82452,#82453,#82454,#82455,
#82456,#82457,#82458,#82459,#82460,#82461,#82462,#82463,#82464,#82465,#82466,
#82467,#82468,#82469,#82470,#82471,#82472,#82473,#82474,#82475,#82476,#82477,
#82478,#82479,#82480,#82481,#82482,#82483,#82484,#82485,#82486,#82487,#82488,
#82489,#82490,#82491,#82492,#82493,#82494,#82495,#82496,#82497,#82498,#82499,
#82500,#82501,#82502,#82503,#82504,#82505,#82506,#82507,#82508,#82509,#82510,
#82511,#82512,#82513,#82514,#82515,#82516,#82517,#82518,#82519,#82520,#82521,
#82522,#82523,#82524,#82525,#82526,#82527,#82528,#82529,#82530,#82531,#82532,
#82533,#82534,#82535,#82536,#82537,#82538,#82539,#82540,#82541,#82542,#82543,
#82544,#82545,#82546,#82547,#82548,#82549,#82550,#82551,#82552,#82553,#82554,
#82555,#82556,#82557,#82558,#82559,#82560,#82561,#82562,#82563,#82564,#82565,
#82566,#82567,#82568,#82569,#82570,#82571,#82572,#82573,#82574,#82575,#82576,
#82577,#82578,#82579,#82580,#82581,#82582,#82583,#82584,#82585,#82586),
 .UNSPECIFIED.,.F.,.F.,(4,3,3,3,3,3,3,3,3,3,3,3,3,3,3,3,3,3,3,3,3,3,3,3,
3,3,3,3,3,3,3,3,3,3,3,3,3,3,3,3,3,3,3,3,3,4),(30.5007344054827,30.5978581347745,
30.6918156853378,30.7857477128349,30.8796798255972,30.9736376246596,31.067700776091,
31.161827167571,31.2560956256276,31.2777242398169,31.3719885583348,31.4661255668587,
31.5601637744116,31.6541352142286,31.7480727900637,31.8420021170799,31.9359487963204,
32.0299963926262,32.1240997354399,32.2183537164704,32.2706256582196,32.3648899598909,
32.4590269513998,32.5530651417941,32.6470365643113,32.7409741227658,32.8349034323424,
32.928850094106,33.0228976729848,33.1170009983745,33.2112549621563,33.2635270766222,
33.3577913774809,33.4519283680829,33.5459665574779,33.6399379788614,33.7338755360994,
33.8278048443779,33.9217515047631,34.0157990821487,34.109902405978,34.2041563681087,
34.2564284950248,34.3705294643833,34.48324688611,34.5575191893195),
 .UNSPECIFIED.);
#682=B_SPLINE_CURVE_WITH_KNOTS('',3,(#82592,#82593,#82594,#82595,#82596,
#82597,#82598,#82599,#82600,#82601,#82602,#82603,#82604,#82605,#82606,#82607,
#82608,#82609,#82610,#82611,#82612,#82613,#82614,#82615,#82616,#82617,#82618,
#82619,#82620,#82621,#82622,#82623,#82624,#82625,#82626,#82627,#82628,#82629,
#82630,#82631,#82632,#82633,#82634,#82635,#82636,#82637,#82638,#82639,#82640,
#82641,#82642,#82643,#82644,#82645,#82646,#82647,#82648,#82649,#82650,#82651,
#82652,#82653,#82654,#82655,#82656,#82657,#82658,#82659,#82660,#82661,#82662,
#82663,#82664,#82665,#82666,#82667,#82668,#82669,#82670,#82671,#82672,#82673,
#82674,#82675,#82676,#82677,#82678,#82679,#82680,#82681,#82682,#82683,#82684,
#82685,#82686,#82687,#82688,#82689,#82690,#82691,#82692,#82693,#82694,#82695,
#82696,#82697,#82698,#82699,#82700,#82701,#82702,#82703,#82704,#82705,#82706,
#82707,#82708,#82709,#82710,#82711,#82712,#82713,#82714,#82715,#82716,#82717,
#82718,#82719,#82720,#82721,#82722,#82723,#82724,#82725,#82726,#82727),
 .UNSPECIFIED.,.F.,.F.,(4,3,3,3,3,3,3,3,3,3,3,3,3,3,3,3,3,3,3,3,3,3,3,3,
3,3,3,3,3,3,3,3,3,3,3,3,3,3,3,3,3,3,3,3,3,4),(24.2171289178558,24.3110581457589,
24.4049973630879,24.4990333500489,24.5931184654238,24.687362266644,24.7667073015423,
24.8609713374983,24.9551080590497,25.0491459756451,25.1431171197724,25.2370543971007,
25.3309834231588,25.4249297993533,25.5189770912628,25.6130801284721,25.7073338049799,
25.7596087199449,25.8538731327047,25.9480102364635,26.042048540105,26.1360200768798,
26.2299577501729,26.3238871750263,26.4178339523628,26.511881646561,26.6059850872946,
26.7002391653289,26.7525101383476,26.8467744488966,26.9409114496918,27.0349496497661,
27.1289210825126,27.2228586515332,27.3167879720004,27.4107346449676,27.5047822354614,
27.5988855727163,27.6931395486428,27.7454115567502,27.8431501298669,27.9407221178994,
28.0380986588194,28.135358661508,28.2324911801573,28.2743338823081),
 .UNSPECIFIED.);
#683=B_SPLINE_CURVE_WITH_KNOTS('',3,(#82728,#82729,#82730,#82731,#82732,
#82733,#82734,#82735,#82736,#82737,#82738,#82739,#82740,#82741,#82742,#82743,
#82744,#82745,#82746,#82747,#82748,#82749,#82750,#82751,#82752,#82753,#82754,
#82755,#82756,#82757,#82758,#82759,#82760,#82761,#82762,#82763,#82764,#82765,
#82766,#82767,#82768,#82769,#82770,#82771,#82772,#82773,#82774,#82775,#82776,
#82777,#82778,#82779,#82780,#82781,#82782,#82783,#82784,#82785,#82786,#82787,
#82788,#82789,#82790,#82791,#82792,#82793,#82794,#82795,#82796,#82797,#82798,
#82799,#82800,#82801,#82802,#82803),.UNSPECIFIED.,.F.,.F.,(4,3,3,3,3,3,
3,3,3,3,3,3,3,3,3,3,3,3,3,3,3,3,3,3,3,4),(28.2743338824719,28.3741025969876,
28.4742017662569,28.574472011735,28.6750305518817,28.7383129751529,28.8325772937002,
28.9267143022538,29.0207525098367,29.1147239496841,29.2086615255499,29.3025908525969,
29.3965375318683,29.490585128205,29.5846884710498,29.678942452111,29.7312143935555,
29.8272597603905,29.9213793427822,30.0154088866135,30.1093741101295,30.2069249146559,
30.3008614012555,30.3948068581838,30.4888131781989,30.4995773282354),
 .UNSPECIFIED.);
#684=B_SPLINE_CURVE_WITH_KNOTS('',3,(#82805,#82806,#82807,#82808,#82809,
#82810,#82811,#82812,#82813,#82814,#82815,#82816,#82817,#82818,#82819,#82820,
#82821,#82822,#82823,#82824,#82825,#82826,#82827,#82828,#82829,#82830,#82831,
#82832,#82833,#82834,#82835,#82836,#82837,#82838,#82839,#82840,#82841,#82842,
#82843,#82844,#82845,#82846,#82847,#82848,#82849,#82850,#82851,#82852,#82853,
#82854,#82855,#82856,#82857,#82858,#82859,#82860,#82861,#82862,#82863,#82864,
#82865,#82866,#82867,#82868,#82869,#82870,#82871,#82872,#82873,#82874,#82875,
#82876,#82877,#82878,#82879,#82880,#82881,#82882,#82883),.UNSPECIFIED.,
 .F.,.F.,(4,3,3,3,3,3,3,3,3,3,3,3,3,3,3,3,3,3,3,3,3,3,3,3,3,3,4),(28.2743338823081,
28.299019984609,28.3932843971923,28.4874215007725,28.5814598042337,28.6754313408263,
28.7693690139363,28.8632984386057,28.9572452157574,29.0512929097711,29.14539635032,
29.2396504281712,29.2919214030116,29.3861857135655,29.4803227143652,29.5743609144437,
29.6683323471937,29.7622699162173,29.8561992366871,29.9501459096564,30.044193500152,
30.1382968374083,30.2325508133356,30.2848228214143,30.3790955390654,30.4732292280887,
30.5007344054827),.UNSPECIFIED.);
#685=B_SPLINE_CURVE_WITH_KNOTS('',3,(#82884,#82885,#82886,#82887,#82888,
#82889,#82890,#82891),.UNSPECIFIED.,.F.,.F.,(4,1,1,1,1,4),(24.2163566964775,
24.3274143109984,25.320315729401,26.3132171478037,27.3061185662063,28.2743305207902),
 .UNSPECIFIED.);
#686=B_SPLINE_CURVE_WITH_KNOTS('',3,(#82897,#82898,#82899,#82900,#82901,
#82902,#82903,#82904,#82905,#82906,#82907,#82908,#82909,#82910,#82911,#82912,
#82913,#82914,#82915,#82916,#82917,#82918,#82919,#82920,#82921,#82922,#82923,
#82924,#82925,#82926,#82927,#82928,#82929,#82930,#82931,#82932,#82933,#82934,
#82935,#82936,#82937,#82938,#82939,#82940,#82941,#82942,#82943,#82944,#82945,
#82946,#82947,#82948,#82949,#82950,#82951,#82952,#82953,#82954,#82955,#82956,
#82957,#82958,#82959,#82960,#82961,#82962,#82963,#82964,#82965,#82966,#82967,
#82968,#82969,#82970,#82971,#82972),.UNSPECIFIED.,.F.,.F.,(4,3,3,3,3,3,
3,3,3,3,3,3,3,3,3,3,3,3,3,3,3,3,3,3,3,4),(15.707963267949,15.8009257619914,
15.8938611105031,15.9867959077331,16.0797567414188,16.1728269203555,16.2659622627033,
16.3592466607815,16.3842029637772,16.4785791144072,16.5728278228513,16.66697743437,
16.7610593414545,16.8551067542938,16.9491451414462,17.043199956675,17.1373535976475,
17.2315619508221,17.3259182756567,17.3771043821798,17.4715160967997,17.565809265615,
17.6600001838905,17.7541298992212,17.8482412804839,17.933562797591),
 .UNSPECIFIED.);
#687=B_SPLINE_CURVE_WITH_KNOTS('',3,(#82974,#82975,#82976,#82977,#82978),
 .UNSPECIFIED.,.F.,.F.,(4,1,4),(14.3984001269719,15.3913015453745,15.7079549083771),
 .UNSPECIFIED.);
#688=B_SPLINE_CURVE_WITH_KNOTS('',3,(#82982,#82983,#82984,#82985,#82986,
#82987,#82988,#82989,#82990,#82991,#82992,#82993,#82994,#82995,#82996,#82997,
#82998,#82999,#83000,#83001,#83002,#83003,#83004,#83005,#83006,#83007,#83008,
#83009,#83010,#83011,#83012,#83013,#83014,#83015,#83016,#83017,#83018,#83019,
#83020,#83021,#83022,#83023,#83024,#83025,#83026,#83027,#83028,#83029,#83030,
#83031,#83032,#83033,#83034,#83035,#83036,#83037,#83038,#83039,#83040,#83041,
#83042,#83043,#83044,#83045),.UNSPECIFIED.,.F.,.F.,(4,3,3,3,3,3,3,3,3,3,
3,3,3,3,3,3,3,3,3,3,3,4),(13.8759339770166,13.969800853008,14.063541445323,
14.1603104043471,14.2538878301271,14.3474345658592,14.4409766902909,14.534540271142,
14.6282042675365,14.7219286532259,14.8157921941949,14.8376931175158,14.9307866091952,
15.0279336915394,15.1207996554847,15.2136126275113,15.3063994726962,15.3991870244372,
15.4920485203054,15.5849537240745,15.677980834301,15.707963267949),
 .UNSPECIFIED.);
#689=B_SPLINE_CURVE_WITH_KNOTS('',3,(#83046,#83047,#83048,#83049,#83050,
#83051,#83052),.UNSPECIFIED.,.F.,.F.,(4,1,1,1,4),(15.707963267949,15.8305945359184,
16.8234959543211,17.8163973727237,17.934417062947),.UNSPECIFIED.);
#690=B_SPLINE_CURVE_WITH_KNOTS('',3,(#83058,#83059,#83060,#83061,#83062,
#83063,#83064,#83065,#83066,#83067),.UNSPECIFIED.,.F.,.F.,(4,2,2,2,4),(-0.0891794197387037,
-0.0404384534220769,-0.012183279177373,-0.0054070073603356,0.),
 .UNSPECIFIED.);
#691=B_SPLINE_CURVE_WITH_KNOTS('',3,(#83070,#83071,#83072,#83073,#83074,
#83075,#83076,#83077,#83078,#83079,#83080,#83081,#83082,#83083,#83084,#83085,
#83086,#83087,#83088,#83089,#83090,#83091,#83092,#83093,#83094,#83095,#83096,
#83097,#83098,#83099,#83100,#83101,#83102,#83103,#83104,#83105,#83106,#83107,
#83108,#83109,#83110,#83111,#83112,#83113,#83114,#83115,#83116,#83117,#83118,
#83119,#83120,#83121,#83122,#83123,#83124,#83125),.UNSPECIFIED.,.F.,.F.,
(4,2,2,2,2,2,2,2,2,2,2,2,2,2,2,2,2,2,2,2,2,2,2,2,2,2,2,4),(-2.19718104682751,
-2.19645858152794,-2.18932165309502,-2.15032845111742,-2.11832204261695,
-2.09604578914239,-2.08390596653947,-2.07287258854925,-2.05759738399719,
-2.01446578143502,-1.98527138501252,-1.96806044418142,-1.96043522719183,
-1.95409249138337,-1.94439702344743,-1.89993652966697,-1.86954642289234,
-1.8480399631896,-1.83610215377107,-1.82515811572939,-1.80990179286441,
-1.75224698036085,-1.73058071279881,-1.71614874303442,-1.70904218146749,
-1.70280042621923,-1.69271885646605,-1.67608637462986),.UNSPECIFIED.);
#692=B_SPLINE_CURVE_WITH_KNOTS('',3,(#83131,#83132,#83133,#83134,#83135,
#83136,#83137,#83138,#83139,#83140,#83141,#83142,#83143,#83144,#83145,#83146,
#83147,#83148,#83149,#83150,#83151,#83152,#83153,#83154,#83155,#83156,#83157,
#83158,#83159,#83160,#83161,#83162,#83163,#83164,#83165,#83166,#83167,#83168,
#83169,#83170,#83171,#83172,#83173,#83174,#83175,#83176,#83177,#83178,#83179,
#83180,#83181,#83182,#83183,#83184,#83185,#83186,#83187,#83188,#83189,#83190,
#83191,#83192,#83193,#83194,#83195,#83196,#83197,#83198,#83199,#83200,#83201,
#83202,#83203,#83204,#83205,#83206,#83207,#83208,#83209,#83210,#83211,#83212,
#83213,#83214,#83215,#83216,#83217,#83218,#83219,#83220,#83221,#83222,#83223,
#83224,#83225,#83226,#83227,#83228,#83229,#83230,#83231,#83232,#83233,#83234,
#83235,#83236,#83237,#83238,#83239,#83240,#83241,#83242,#83243,#83244,#83245,
#83246,#83247,#83248,#83249,#83250,#83251,#83252,#83253,#83254,#83255,#83256,
#83257,#83258,#83259,#83260,#83261,#83262,#83263,#83264,#83265,#83266,#83267,
#83268,#83269,#83270,#83271,#83272,#83273,#83274,#83275,#83276,#83277,#83278,
#83279,#83280,#83281,#83282,#83283,#83284,#83285,#83286,#83287,#83288,#83289,
#83290,#83291,#83292,#83293,#83294,#83295,#83296,#83297,#83298,#83299,#83300,
#83301,#83302,#83303,#83304,#83305,#83306,#83307,#83308,#83309,#83310,#83311),
 .UNSPECIFIED.,.F.,.F.,(4,3,3,3,3,3,3,3,3,3,3,3,3,3,3,3,3,3,3,3,3,3,3,3,
3,3,3,3,3,3,3,3,3,3,3,3,3,3,3,3,3,3,3,3,3,3,3,3,3,3,3,3,3,3,3,3,3,3,3,3,
4),(33.079934870469,33.1787177894596,33.2774733872199,33.3762313802265,
33.4750880185667,33.5739937416401,33.6730724278617,33.7586482256901,33.8577570182368,
33.9567262428988,34.0560791680481,34.1548734814301,34.253635757772,34.3523957095728,
34.4521841932028,34.5510854562345,34.6513175501636,34.7515496440927,34.8505116619609,
34.9493335207729,35.0487232134882,35.1473697968322,35.2459845308404,35.3445973248064,
35.4445607592287,35.5433172973594,35.6438841799274,35.7444510624954,35.8437171136992,
35.9428428037689,36.0421565134101,36.1411042244635,36.2400184017015,36.3389285537144,
36.4385345355103,36.5375803171594,36.6374663990287,36.737352480898,36.83654561436,
36.9356010198157,37.0349326297513,37.1338168838387,37.2326702948661,37.3315224367231,
37.4312053023675,37.5302003418486,37.6302271205746,37.7302538993007,37.8283438241589,
37.9262933983847,38.0259011382996,38.1236806968838,38.2214320150539,38.3191859967539,
38.4201783269913,38.518095715075,38.6206255163892,38.7231553177033,38.8550550269612,
38.9837128251521,39.0086643481542),.UNSPECIFIED.);
#693=B_SPLINE_CURVE_WITH_KNOTS('',3,(#83312,#83313,#83314,#83315,#83316,
#83317,#83318,#83319,#83320,#83321,#83322,#83323,#83324,#83325),
 .UNSPECIFIED.,.F.,.F.,(4,2,2,2,2,2,4),(-0.178828740417439,-0.148696555674604,
-0.131054670705411,-0.117602908728372,-0.105711018511371,-0.0894577948770551,
-0.0891794197387037),.UNSPECIFIED.);
#694=B_SPLINE_CURVE_WITH_KNOTS('',3,(#83326,#83327,#83328,#83329,#83330,
#83331,#83332,#83333,#83334,#83335,#83336,#83337,#83338,#83339,#83340,#83341,
#83342,#83343,#83344,#83345,#83346,#83347,#83348,#83349,#83350,#83351,#83352,
#83353,#83354,#83355,#83356,#83357,#83358,#83359,#83360,#83361,#83362,#83363,
#83364,#83365,#83366,#83367,#83368,#83369,#83370,#83371,#83372,#83373,#83374,
#83375,#83376,#83377,#83378,#83379,#83380,#83381,#83382,#83383,#83384,#83385,
#83386,#83387,#83388,#83389,#83390,#83391,#83392,#83393,#83394,#83395,#83396,
#83397,#83398,#83399,#83400,#83401,#83402,#83403,#83404,#83405,#83406,#83407,
#83408,#83409,#83410,#83411,#83412,#83413,#83414,#83415,#83416,#83417,#83418,
#83419,#83420,#83421,#83422,#83423,#83424,#83425,#83426,#83427,#83428,#83429,
#83430,#83431,#83432,#83433,#83434,#83435,#83436,#83437,#83438,#83439,#83440,
#83441,#83442,#83443,#83444,#83445,#83446,#83447,#83448,#83449,#83450,#83451,
#83452,#83453,#83454,#83455,#83456,#83457,#83458,#83459,#83460,#83461,#83462,
#83463,#83464,#83465,#83466,#83467,#83468,#83469,#83470,#83471,#83472,#83473,
#83474,#83475,#83476,#83477),.UNSPECIFIED.,.F.,.F.,(4,2,2,2,2,2,2,2,2,2,
2,2,2,2,2,2,2,2,2,2,2,2,2,2,2,2,2,2,2,2,2,2,2,2,2,2,2,2,2,2,2,2,2,2,2,2,
2,2,2,2,2,2,2,2,2,2,2,2,2,2,2,2,2,2,2,2,2,2,2,2,2,2,2,2,2,4),(-1.67608637462986,
-1.65687732929873,-1.62150669571193,-1.59809880019172,-1.58595568834587,
-1.57523193825967,-1.56120312823587,-1.50340369105419,-1.4804032775575,
-1.46544522879122,-1.45828994231978,-1.45207772281957,-1.44223763959186,
-1.39973102571514,-1.36815220530213,-1.3461400200849,-1.33414089633424,
-1.32325608559398,-1.30827425353094,-1.27361347699094,-1.24298186377057,
-1.22589234207498,-1.21355300420792,-1.20681156948572,-1.20020487396986,
-1.18853404833856,-1.13693688228772,-1.10104754529816,-1.08748866548457,
-1.07675204196991,-1.06397420315739,-1.03626793101884,-0.985730691755481,
-0.96646465694695,-0.9585409114734,-0.95239260804874,-0.943735945622945,
-0.914830519314583,-0.852511535606085,-0.839536044514228,-0.828619201443956,
-0.816856476100891,-0.796170252696613,-0.767688481950534,-0.718690361686391,
-0.70950920017578,-0.703315870755706,-0.695744660943167,-0.678234129685828,
-0.648195237002004,-0.604153246978942,-0.588788611265734,-0.577871755610879,
-0.566061605072287,-0.545134452920513,-0.516104985097223,-0.468429542707585,
-0.459108393407661,-0.45289439172849,-0.445391289165089,-0.428359750747527,
-0.399772116764656,-0.353548048375749,-0.338224087500789,-0.32731626767606,
-0.315499073747651,-0.294510667550791,-0.265342259784795,-0.217920436646892,
-0.208570811893949,-0.202356109969582,-0.194876006641539,-0.177994331427986,
-0.149845137636229,-0.102902361229971,-0.0902464959671978),
 .UNSPECIFIED.);
#695=B_SPLINE_CURVE_WITH_KNOTS('',3,(#83483,#83484,#83485,#83486,#83487,
#83488,#83489,#83490,#83491,#83492,#83493,#83494,#83495,#83496,#83497,#83498,
#83499,#83500,#83501,#83502,#83503,#83504,#83505,#83506,#83507,#83508,#83509,
#83510,#83511,#83512,#83513,#83514,#83515,#83516,#83517,#83518,#83519,#83520,
#83521,#83522,#83523,#83524,#83525,#83526,#83527,#83528,#83529,#83530,#83531,
#83532,#83533,#83534,#83535,#83536,#83537,#83538,#83539,#83540,#83541,#83542,
#83543,#83544,#83545,#83546,#83547,#83548,#83549,#83550,#83551,#83552,#83553,
#83554,#83555,#83556,#83557,#83558,#83559,#83560,#83561,#83562,#83563,#83564,
#83565,#83566,#83567,#83568,#83569,#83570,#83571,#83572,#83573,#83574,#83575,
#83576,#83577,#83578,#83579,#83580,#83581,#83582,#83583,#83584,#83585,#83586,
#83587,#83588,#83589,#83590,#83591,#83592,#83593,#83594,#83595,#83596,#83597,
#83598,#83599,#83600,#83601,#83602,#83603,#83604,#83605,#83606,#83607,#83608,
#83609,#83610,#83611,#83612,#83613,#83614,#83615,#83616,#83617,#83618,#83619,
#83620,#83621,#83622,#83623,#83624,#83625,#83626,#83627,#83628,#83629,#83630,
#83631,#83632,#83633,#83634,#83635,#83636,#83637,#83638,#83639,#83640,#83641,
#83642,#83643,#83644,#83645,#83646,#83647,#83648,#83649,#83650,#83651,#83652,
#83653,#83654,#83655,#83656,#83657,#83658,#83659,#83660,#83661,#83662,#83663,
#83664,#83665,#83666),.UNSPECIFIED.,.F.,.F.,(4,3,3,3,3,3,3,3,3,3,3,3,3,
3,3,3,3,3,3,3,3,3,3,3,3,3,3,3,3,3,3,3,3,3,3,3,3,3,3,3,3,3,3,3,3,3,3,3,3,
3,3,3,3,3,3,3,3,3,3,3,3,4),(26.7961971418499,26.8083382968715,26.9074246897037,
27.0063712146189,27.1057297772008,27.2045008356489,27.3032397020132,27.4019761219099,
27.501792020251,27.6006696972515,27.7009547062628,27.8012397152742,27.9003266636363,
27.9992737513498,28.0986321741407,28.1974038087594,28.296143254997,28.3948802576534,
28.4946954766592,28.5935737374497,28.6938574355633,28.7941411336768,28.8932250348956,
28.9921690680764,29.0915282535767,29.1902968380783,29.2890332426283,29.3877672161178,
29.4875860501082,29.5864613431686,29.6867519476241,29.7870425520795,29.8861308341416,
29.9850792362496,30.0844373280286,30.1832102211334,30.2819509022162,30.3806891145515,
30.4805028285342,30.5793822255267,30.6796630980044,30.7799439704821,30.8790345145378,
30.977985232193,31.0773427517795,31.1761180722291,31.2748612169249,31.3736019255314,
31.4734127913698,31.5722947382858,31.6725700635853,31.7728453888848,31.8712868407757,
31.9695889139027,32.0677797276253,32.1659104762213,32.2640117568114,32.3621141291314,
32.4603109955813,32.558557434612,32.6569676584442,32.7254896765486),
 .UNSPECIFIED.);
#696=B_SPLINE_CURVE_WITH_KNOTS('',3,(#83667,#83668,#83669,#83670,#83671,
#83672,#83673,#83674,#83675,#83676,#83677,#83678,#83679,#83680,#83681,#83682),
 .UNSPECIFIED.,.F.,.F.,(4,3,3,3,3,4),(32.725489676875,32.7657468072874,
32.8648376513885,32.9638055933405,33.0626616366559,33.079934870469),
 .UNSPECIFIED.);
#697=B_SPLINE_CURVE_WITH_KNOTS('',3,(#83684,#83685,#83686,#83687,#83688,
#83689,#83690,#83691,#83692,#83693,#83694,#83695),.UNSPECIFIED.,.F.,.F.,
(4,2,2,2,2,4),(-0.0902464959671978,-0.0876094181756293,-0.0767074401332747,
-0.0648824535281501,-0.0438358835002987,-0.000729091238856221),
 .UNSPECIFIED.);
#698=B_SPLINE_CURVE_WITH_KNOTS('',3,(#83696,#83697,#83698,#83699,#83700,
#83701,#83702,#83703,#83704,#83705,#83706,#83707,#83708,#83709,#83710,#83711,
#83712,#83713,#83714,#83715,#83716,#83717,#83718,#83719,#83720,#83721,#83722,
#83723,#83724,#83725,#83726,#83727,#83728,#83729,#83730,#83731,#83732,#83733,
#83734,#83735,#83736,#83737,#83738,#83739,#83740,#83741,#83742,#83743,#83744,
#83745,#83746,#83747,#83748,#83749,#83750,#83751,#83752,#83753,#83754,#83755,
#83756,#83757,#83758,#83759,#83760,#83761,#83762,#83763,#83764,#83765,#83766,
#83767,#83768,#83769,#83770,#83771,#83772,#83773,#83774,#83775,#83776,#83777,
#83778,#83779,#83780,#83781,#83782,#83783,#83784,#83785,#83786,#83787,#83788,
#83789,#83790,#83791,#83792,#83793,#83794,#83795,#83796,#83797,#83798,#83799,
#83800,#83801,#83802,#83803,#83804,#83805,#83806,#83807,#83808,#83809,#83810,
#83811,#83812,#83813,#83814,#83815,#83816,#83817,#83818,#83819,#83820,#83821,
#83822,#83823,#83824,#83825,#83826,#83827,#83828,#83829,#83830,#83831,#83832,
#83833,#83834,#83835,#83836,#83837,#83838,#83839,#83840,#83841,#83842,#83843),
 .UNSPECIFIED.,.F.,.F.,(4,2,2,2,2,2,2,2,2,2,2,2,2,2,2,2,2,2,2,2,2,2,2,2,
2,2,2,2,2,2,2,2,2,2,2,2,2,2,2,2,2,2,2,2,2,2,2,2,2,2,2,2,2,2,2,2,2,2,2,2,
2,2,2,2,2,2,2,2,2,2,2,2,2,4),(-3.17275100264301,-3.14186154461218,-3.13391409134658,
-3.12678168783638,-3.12052738437692,-3.11046928271894,-3.0731019603304,
-3.03864936246736,-3.01554524537885,-3.00339627109982,-2.99258199427153,
-2.97803186410277,-2.92311059284616,-2.89904747261095,-2.88365703590017,
-2.87640159181438,-2.87019111156838,-2.86042990399181,-2.81692426495564,
-2.78589648558406,-2.76412306997584,-2.75217855489811,-2.74131031810344,
-2.72630553692097,-2.69124774359334,-2.65418066394503,-2.63464265155557,
-2.62680585721525,-2.62064554179685,-2.61185961982967,-2.58205337124216,
-2.54078613948644,-2.51542872926686,-2.50295632111094,-2.49219628449891,
-2.47845711696807,-2.41843773622056,-2.39648021659992,-2.38193940820278,
-2.37482226251611,-2.3685595639494,-2.35845362519604,-2.32212341401948,
-2.28705579500856,-2.26372576792335,-2.25154177326307,-2.24073318534329,
-2.22624767424738,-2.17077305608563,-2.14694101379957,-2.13163998576844,
-2.12439815366644,-2.11818188436821,-2.10838569704584,-2.06526937981979,
-2.01895781217817,-2.00479172184713,-1.99401417590832,-1.98165464286044,
-1.95711580672057,-1.94344505849879,-1.90317670897896,-1.88285251345712,
-1.8749212517719,-1.86876804610265,-1.86010430858303,-1.83300238482102,
-1.7958737414637,-1.7653517346366,-1.75225782536403,-1.74153208370379,-1.72833682184749,
-1.69978587912751,-1.67614713822004),.UNSPECIFIED.);
#699=B_SPLINE_CURVE_WITH_KNOTS('',3,(#83849,#83850,#83851,#83852,#83853,
#83854,#83855,#83856,#83857,#83858),.UNSPECIFIED.,.F.,.F.,(4,1,1,1,1,1,
1,4),(20.5123630354388,20.8509297864556,21.8438312048583,22.8367326232609,
23.8296340416636,24.8225354600662,25.8154368784689,26.4423043696954),
 .UNSPECIFIED.);
#700=B_SPLINE_CURVE_WITH_KNOTS('',3,(#83859,#83860,#83861,#83862,#83863,
#83864,#83865,#83866,#83867,#83868,#83869,#83870,#83871),.UNSPECIFIED.,
 .F.,.F.,(4,3,3,3,4),(26.4423043696954,26.5538023218569,26.665819695498,
26.778442329872,26.7961971418499),.UNSPECIFIED.);
#701=B_SPLINE_CURVE_WITH_KNOTS('',3,(#83872,#83873,#83874,#83875,#83876,
#83877,#83878,#83879,#83880,#83881,#83882,#83883,#83884,#83885,#83886,#83887,
#83888,#83889,#83890,#83891,#83892,#83893,#83894,#83895,#83896,#83897,#83898,
#83899,#83900,#83901,#83902,#83903,#83904,#83905,#83906,#83907,#83908,#83909,
#83910,#83911,#83912,#83913,#83914,#83915,#83916,#83917,#83918,#83919,#83920,
#83921,#83922,#83923,#83924,#83925,#83926,#83927,#83928,#83929,#83930,#83931,
#83932,#83933,#83934,#83935,#83936,#83937,#83938,#83939,#83940,#83941,#83942,
#83943,#83944,#83945,#83946,#83947,#83948,#83949,#83950,#83951,#83952,#83953,
#83954,#83955,#83956,#83957,#83958,#83959,#83960,#83961,#83962,#83963,#83964,
#83965,#83966,#83967,#83968,#83969,#83970,#83971,#83972,#83973,#83974,#83975,
#83976,#83977,#83978,#83979,#83980,#83981,#83982,#83983,#83984,#83985,#83986,
#83987,#83988,#83989,#83990,#83991,#83992,#83993,#83994,#83995,#83996,#83997,
#83998,#83999,#84000,#84001,#84002,#84003,#84004,#84005,#84006,#84007,#84008,
#84009,#84010,#84011,#84012,#84013,#84014,#84015,#84016,#84017,#84018,#84019,
#84020,#84021,#84022,#84023,#84024,#84025,#84026,#84027,#84028,#84029,#84030,
#84031),.UNSPECIFIED.,.F.,.F.,(4,2,2,2,2,2,2,2,2,2,2,2,2,2,2,2,2,2,2,2,
2,2,2,2,2,2,2,2,2,2,2,2,2,2,2,2,2,2,2,2,2,2,2,2,2,2,2,2,2,2,2,2,2,2,2,2,
2,2,2,2,2,2,2,2,2,2,2,2,2,2,2,2,2,2,2,2,2,2,2,4),(-1.67614713822004,-1.65401491148783,
-1.63251175695329,-1.62444928224132,-1.61830360713468,-1.60979944321575,
-1.58696249204113,-1.52960393139486,-1.50957186701517,-1.49790654268451,
-1.48692695737201,-1.47112058969116,-1.45223197297707,-1.40489495726156,
-1.38255085293624,-1.37499654555521,-1.36881635347511,-1.3611306407341,
-1.34278704356159,-1.31005547939534,-1.26959246473498,-1.25432849237837,
-1.24342545598734,-1.23157987920752,-1.2104338861163,-1.18090569021946,
-1.1342505763082,-1.1248144059171,-1.11858647777933,-1.1111452773009,-1.09454553617311,
-1.0672186360059,-1.01882421882921,-1.00360804187264,-0.99271197540947,
-0.980849747096349,-0.959596069961657,-0.929814359854932,-0.883722915131605,
-0.874227544364716,-0.867992282891039,-0.860581824198139,-0.844186378574769,
-0.817434397532054,-0.767999114531816,-0.752862232035203,-0.741977246487827,
-0.730085985061274,-0.708646138072557,-0.678422330470221,-0.633297614617569,
-0.623701010386046,-0.617452516392324,-0.61009212944287,-0.594025323639252,
-0.568177210783094,-0.517003661116067,-0.502025530146775,-0.491161609799766,
-0.479208204462634,-0.45737031425613,-0.426182182130144,-0.38306916999317,
-0.373281596103964,-0.367068071226507,-0.359826373340644,-0.344516644135123,
-0.32065728539347,-0.265219811356024,-0.250729590978973,-0.239923545802512,
-0.227748504194372,-0.204456692528434,-0.169482548134206,-0.133092781942825,
-0.122991718627395,-0.116731300983826,-0.109616022657332,-0.0950772289438299,
-0.0900798583104094),.UNSPECIFIED.);
#702=B_SPLINE_CURVE_WITH_KNOTS('',3,(#84037,#84038,#84039,#84040,#84041,
#84042,#84043,#84044,#84045,#84046,#84047,#84048,#84049,#84050,#84051,#84052,
#84053,#84054,#84055,#84056,#84057,#84058,#84059,#84060,#84061,#84062,#84063,
#84064,#84065,#84066,#84067,#84068,#84069,#84070,#84071,#84072,#84073,#84074,
#84075,#84076,#84077,#84078,#84079,#84080,#84081,#84082,#84083,#84084,#84085,
#84086,#84087,#84088,#84089,#84090,#84091,#84092,#84093,#84094,#84095,#84096,
#84097,#84098,#84099,#84100,#84101,#84102,#84103,#84104,#84105,#84106,#84107,
#84108,#84109,#84110,#84111,#84112,#84113,#84114,#84115,#84116,#84117,#84118,
#84119,#84120,#84121,#84122,#84123,#84124,#84125,#84126,#84127,#84128,#84129,
#84130,#84131,#84132,#84133,#84134,#84135,#84136,#84137,#84138,#84139,#84140,
#84141,#84142,#84143,#84144,#84145,#84146,#84147,#84148,#84149,#84150,#84151,
#84152,#84153,#84154,#84155,#84156,#84157,#84158,#84159,#84160,#84161,#84162,
#84163,#84164,#84165,#84166,#84167,#84168,#84169,#84170,#84171,#84172,#84173,
#84174,#84175,#84176,#84177,#84178,#84179,#84180,#84181,#84182,#84183,#84184,
#84185,#84186,#84187,#84188,#84189,#84190,#84191,#84192,#84193,#84194,#84195,
#84196,#84197,#84198,#84199,#84200,#84201,#84202,#84203,#84204,#84205,#84206,
#84207,#84208,#84209,#84210,#84211,#84212,#84213,#84214,#84215,#84216,#84217),
 .UNSPECIFIED.,.F.,.F.,(4,3,3,3,3,3,3,3,3,3,3,3,3,3,3,3,3,3,3,3,3,3,3,3,
3,3,3,3,3,3,3,3,3,3,3,3,3,3,3,3,3,3,3,3,3,3,3,3,3,3,3,3,3,3,3,3,3,3,3,3,
4),(14.2303478778739,14.329105063061,14.4278397994346,14.5265818258258,
14.6254258105938,14.7243233111684,14.8233894932032,14.8935212760397,14.9926074889702,
15.091553836683,15.1909124439029,15.2896833329404,15.3884220331809,15.487158290449,
15.5869743914473,15.6858519159895,15.7861373052159,15.8864226944424,15.9855088639308,
16.0844551671027,16.1838137853205,16.2825846274612,16.3813232800216,16.4800594888892,
16.5798756448781,16.6787531197307,16.7790386162878,16.879324112845,16.9784103341468,
17.0773566899656,17.1767152951259,17.2754861915545,17.3742248988989,17.4729611629723,
17.5727772550412,17.6716547855774,17.7719401584125,17.8722255312477,17.9713117348412,
18.0702580727662,18.1696166823767,18.2683875605948,18.3671262496506,18.4658624953827,
18.5656786089496,18.6645561212032,18.7648415354267,18.8651269496503,18.9642131523896,
19.0631594893563,19.1625180991934,19.2612889762052,19.3600276639639,19.4587639083096,
19.5585800232454,19.6574575339053,19.7577429509792,19.858028368053,19.9779659444179,
20.0964128676089,20.1591190625158),.UNSPECIFIED.);
#703=B_SPLINE_CURVE_WITH_KNOTS('',3,(#84218,#84219,#84220,#84221),
 .UNSPECIFIED.,.F.,.F.,(4,4),(20.1591190625158,20.5123630354388),
 .UNSPECIFIED.);
#704=B_SPLINE_CURVE_WITH_KNOTS('',3,(#84223,#84224,#84225,#84226,#84227,
#84228,#84229,#84230,#84231,#84232),.UNSPECIFIED.,.F.,.F.,(4,2,2,2,4),(-0.0900798583104094,
-0.0731194009899147,-0.0178332553777174,-0.0079637246705691,-0.000765186884287919),
 .UNSPECIFIED.);
#705=B_SPLINE_CURVE_WITH_KNOTS('',3,(#84233,#84234,#84235,#84236,#84237,
#84238,#84239,#84240,#84241,#84242),.UNSPECIFIED.,.F.,.F.,(4,1,1,1,1,1,
1,4),(-16.4153450200003,-15.8864226944424,-14.8935212760397,-13.9006198576371,
-12.9077184392344,-11.9148170208318,-10.9219156024291,-10.4858135521078),
 .UNSPECIFIED.);
#706=B_SPLINE_CURVE_WITH_KNOTS('',3,(#84248,#84249,#84250,#84251,#84252,
#84253,#84254,#84255,#84256,#84257,#84258,#84259,#84260),.UNSPECIFIED.,
 .F.,.F.,(4,3,3,3,4),(-4.20357440982612,-4.10477081863081,-4.00580716021436,
-3.9716056736106,-3.84897440564112),.UNSPECIFIED.);
#707=B_SPLINE_CURVE_WITH_KNOTS('',3,(#84262,#84263,#84264,#84265,#84266,
#84267,#84268,#84269,#84270,#84271,#84272,#84273,#84274,#84275,#84276,#84277,
#84278,#84279,#84280,#84281,#84282,#84283,#84284,#84285,#84286,#84287,#84288,
#84289,#84290,#84291,#84292,#84293,#84294,#84295,#84296,#84297,#84298,#84299,
#84300,#84301,#84302,#84303,#84304,#84305,#84306,#84307,#84308,#84309,#84310,
#84311,#84312,#84313,#84314,#84315,#84316,#84317,#84318,#84319,#84320,#84321,
#84322,#84323,#84324,#84325,#84326,#84327,#84328,#84329,#84330,#84331,#84332,
#84333,#84334,#84335,#84336,#84337,#84338,#84339,#84340,#84341,#84342,#84343,
#84344,#84345,#84346,#84347,#84348,#84349,#84350,#84351,#84352,#84353,#84354,
#84355,#84356,#84357,#84358,#84359,#84360,#84361,#84362,#84363,#84364,#84365,
#84366,#84367,#84368,#84369,#84370,#84371,#84372,#84373,#84374,#84375,#84376,
#84377,#84378,#84379),.UNSPECIFIED.,.F.,.F.,(4,3,3,3,3,3,3,3,3,3,3,3,3,
3,3,3,3,3,3,3,3,3,3,3,3,3,3,3,3,3,3,3,3,3,3,3,3,3,3,4),(-3.84897440539012,
-3.75118261568908,-3.65352307956186,-3.55593660581752,-3.45839196281045,
-3.36085797170509,-3.26323988314662,-3.16558158777684,-3.06775694336586,
-2.97870425520795,-2.87951096573215,-2.78045540351959,-2.6811238326803,
-2.58223942123546,-2.48338585298897,-2.38453355427412,-2.28485087490691,
-2.18585568108901,-2.08582925894716,-1.9858028368053,-1.88771322941384,
-1.78976397356157,-1.6901561541667,-1.59237691450442,-1.49462591498151,
-1.39687225137187,-1.29587954312957,-1.19796246900829,-1.09543194370547,
-0.992901418402649,-0.89112328419197,-0.789504516915043,-0.688044984898128,
-0.586679197074179,-0.485382845519511,-0.384131701056394,-0.282872156371267,
-0.181614269833575,-0.0802834070124286,0.),.UNSPECIFIED.);
#708=B_SPLINE_CURVE_WITH_KNOTS('',3,(#84383,#84384,#84385,#84386,#84387,
#84388,#84389,#84390,#84391,#84392,#84393,#84394,#84395,#84396,#84397,#84398,
#84399,#84400,#84401,#84402,#84403,#84404,#84405,#84406,#84407,#84408,#84409,
#84410,#84411,#84412,#84413,#84414,#84415,#84416,#84417,#84418,#84419,#84420,
#84421,#84422,#84423,#84424,#84425,#84426,#84427,#84428,#84429,#84430,#84431,
#84432,#84433,#84434,#84435,#84436,#84437,#84438,#84439,#84440,#84441,#84442,
#84443,#84444,#84445,#84446,#84447,#84448,#84449,#84450,#84451,#84452,#84453,
#84454,#84455,#84456,#84457,#84458,#84459,#84460,#84461,#84462,#84463,#84464,
#84465,#84466,#84467,#84468,#84469,#84470,#84471,#84472,#84473,#84474,#84475,
#84476,#84477,#84478,#84479,#84480,#84481,#84482,#84483,#84484,#84485,#84486,
#84487,#84488,#84489,#84490,#84491,#84492,#84493,#84494,#84495,#84496,#84497,
#84498,#84499,#84500,#84501,#84502,#84503,#84504,#84505,#84506,#84507,#84508,
#84509,#84510,#84511,#84512,#84513,#84514,#84515,#84516,#84517,#84518,#84519,
#84520,#84521,#84522,#84523,#84524,#84525,#84526,#84527,#84528,#84529,#84530,
#84531,#84532,#84533,#84534,#84535,#84536,#84537,#84538,#84539,#84540,#84541,
#84542,#84543,#84544,#84545,#84546,#84547,#84548,#84549,#84550,#84551,#84552,
#84553,#84554),.UNSPECIFIED.,.F.,.F.,(4,3,3,3,3,3,3,3,3,3,3,3,3,3,3,3,3,
3,3,3,3,3,3,3,3,3,3,3,3,3,3,3,3,3,3,3,3,3,3,3,3,3,3,3,3,3,3,3,3,3,3,3,3,
3,3,3,3,4),(2.01695736539979,2.11562565186726,2.21415522447183,2.3125739720312,
2.41093268850728,2.50926169686093,2.60759128292761,2.70601567817816,2.80448866800834,
2.90312821026225,2.97870425520795,3.07795262354351,3.1770644355191,3.27638209028053,
3.3753252578773,3.47423841070976,3.57315105478647,3.6727647094925,3.77182156828368,
3.87171362094714,3.9716056736106,4.07057405953448,4.16940092002274,4.26878919152156,
4.36743741751875,4.46605253078176,4.56466444154242,4.66462510416012,4.76337766491379,
4.86394237846352,4.96450709201325,5.06361683813577,5.1625868114871,5.2619395238532,
5.36073408273825,5.45949641510771,5.55825623360058,5.65804430280441,5.75694496937577,
5.85717673989584,5.9574085104159,6.05651255527721,6.15547712567804,6.25483122607061,
6.35362115696554,6.45237916506658,6.55113497045899,6.65092871004888,6.74982617701673,
6.85006805291764,6.95030992881855,7.04969433302994,7.14893807815273,7.24807060895532,
7.34712014750351,7.44612108226041,7.5451208045432,7.59274844815667),
 .UNSPECIFIED.);
#709=B_SPLINE_CURVE_WITH_KNOTS('',3,(#84555,#84556,#84557,#84558,#84559,
#84560,#84561,#84562,#84563,#84564,#84565,#84566,#84567),.UNSPECIFIED.,
 .F.,.F.,(4,3,3,3,4),(7.59274844852443,7.70563146856783,7.82442140789452,
7.9432113472212,7.94673289122112),.UNSPECIFIED.);
#710=B_SPLINE_CURVE_WITH_KNOTS('',3,(#84573,#84574,#84575,#84576,#84577,
#84578,#84579,#84580,#84581,#84582),.UNSPECIFIED.,.F.,.F.,(4,2,2,2,4),(-0.0892373222902252,
-0.0215572701752487,-0.00841522927678683,-0.00391774174210212,0.),
 .UNSPECIFIED.);
#711=B_SPLINE_CURVE_WITH_KNOTS('',3,(#84585,#84586,#84587,#84588,#84589,
#84590,#84591,#84592,#84593,#84594,#84595,#84596,#84597,#84598,#84599,#84600,
#84601,#84602,#84603,#84604,#84605,#84606,#84607,#84608,#84609,#84610,#84611,
#84612,#84613,#84614,#84615,#84616,#84617,#84618,#84619,#84620,#84621,#84622,
#84623,#84624,#84625,#84626,#84627,#84628,#84629,#84630,#84631,#84632,#84633,
#84634,#84635,#84636,#84637,#84638,#84639,#84640),.UNSPECIFIED.,.F.,.F.,
(4,2,2,2,2,2,2,2,2,2,2,2,2,2,2,2,2,2,2,2,2,2,2,2,2,2,2,4),(-2.19717915922714,
-2.19645659009491,-2.18931965603961,-2.15050379135875,-2.11839010273414,
-2.09607100903603,-2.08392470023533,-2.07289364098603,-2.05763555569738,
-2.01581763729026,-1.98568438600816,-1.96817169548238,-1.96050423950668,
-1.95417132940057,-1.94455971106179,-1.89929675230279,-1.86927758549977,
-1.84792623098591,-1.83601276060896,-1.82505977551714,-1.80973768729716,
-1.76181010825729,-1.73403052891512,-1.71725415524436,-1.70977854721702,
-1.70358054739824,-1.69426186068016,-1.67609529766553),.UNSPECIFIED.);
#712=B_SPLINE_CURVE_WITH_KNOTS('',3,(#84646,#84647,#84648,#84649,#84650,
#84651,#84652,#84653,#84654,#84655,#84656,#84657,#84658,#84659,#84660,#84661,
#84662,#84663,#84664,#84665,#84666,#84667,#84668,#84669,#84670,#84671,#84672,
#84673,#84674,#84675,#84676,#84677,#84678,#84679,#84680,#84681,#84682,#84683,
#84684,#84685,#84686,#84687,#84688,#84689,#84690,#84691,#84692,#84693,#84694,
#84695,#84696,#84697,#84698,#84699,#84700,#84701,#84702,#84703,#84704,#84705,
#84706,#84707,#84708,#84709,#84710,#84711,#84712,#84713,#84714,#84715,#84716,
#84717,#84718,#84719,#84720,#84721,#84722,#84723,#84724,#84725,#84726,#84727,
#84728,#84729,#84730,#84731,#84732,#84733,#84734,#84735,#84736,#84737,#84738,
#84739,#84740,#84741,#84742,#84743,#84744,#84745,#84746,#84747,#84748,#84749,
#84750,#84751,#84752,#84753,#84754,#84755,#84756,#84757,#84758,#84759,#84760,
#84761,#84762,#84763,#84764,#84765,#84766,#84767,#84768,#84769,#84770,#84771,
#84772,#84773,#84774,#84775,#84776,#84777,#84778,#84779,#84780,#84781,#84782,
#84783,#84784,#84785,#84786,#84787,#84788,#84789,#84790,#84791,#84792,#84793,
#84794,#84795,#84796,#84797,#84798,#84799,#84800,#84801,#84802,#84803,#84804,
#84805,#84806,#84807,#84808,#84809,#84810,#84811,#84812,#84813,#84814,#84815,
#84816,#84817,#84818,#84819,#84820,#84821,#84822,#84823,#84824,#84825,#84826),
 .UNSPECIFIED.,.F.,.F.,(4,3,3,3,3,3,3,3,3,3,3,3,3,3,3,3,3,3,3,3,3,3,3,3,
3,3,3,3,3,3,3,3,3,3,3,3,3,3,3,3,3,3,3,3,3,3,3,3,3,3,3,3,3,3,3,3,3,3,3,3,
4),(33.0799350929859,33.1787180525024,33.27747369025,33.3762317226554,33.4750883991966,
33.5739941598867,33.6730728822677,33.7586482256901,33.857757189267,33.9567265860696,
34.0560794683225,34.1548739552646,34.2536364053097,34.3523965307192,34.4521848090626,
34.5510862436967,34.6513179438947,34.7515496440927,34.8505112553917,34.9493327069361,
35.048722501381,35.1473686785809,35.2459830077185,35.3445953985981,35.4445593145724,
35.5433154579641,35.6438832602297,35.7444510624954,35.8437172783021,35.942843131204,
36.0421567999157,36.141104668409,36.2400190007244,36.3389293052607,36.43853509917,
36.537581025639,36.6374667532685,36.737352480898,36.8365465941635,36.9356029841046,
37.0349343485041,37.1338195908865,37.2326739893535,37.3315271163957,37.431208812122,
37.5302048209883,37.6302293601445,37.7302538993007,37.8283418314163,37.9262894071898,
38.025897646004,38.1236752026466,38.2214245205825,38.3191765055242,38.420171208569,
38.5180866257596,38.6206209717314,38.7231553177033,38.8550671088507,38.9837349211043,
39.0086643637188),.UNSPECIFIED.);
#713=B_SPLINE_CURVE_WITH_KNOTS('',3,(#84827,#84828,#84829,#84830,#84831,
#84832,#84833,#84834,#84835,#84836,#84837,#84838,#84839,#84840),
 .UNSPECIFIED.,.F.,.F.,(4,2,2,2,2,2,4),(-0.178881538265878,-0.14875089528117,
-0.131111218924469,-0.117656600924242,-0.105764816929103,-0.0895156630152576,
-0.0892373222902252),.UNSPECIFIED.);
#714=B_SPLINE_CURVE_WITH_KNOTS('',3,(#84841,#84842,#84843,#84844,#84845,
#84846,#84847,#84848,#84849,#84850,#84851,#84852,#84853,#84854,#84855,#84856,
#84857,#84858,#84859,#84860,#84861,#84862,#84863,#84864,#84865,#84866,#84867,
#84868,#84869,#84870,#84871,#84872,#84873,#84874,#84875,#84876,#84877,#84878,
#84879,#84880,#84881,#84882,#84883,#84884,#84885,#84886,#84887,#84888,#84889,
#84890,#84891,#84892,#84893,#84894,#84895,#84896,#84897,#84898,#84899,#84900,
#84901,#84902,#84903,#84904,#84905,#84906,#84907,#84908,#84909,#84910,#84911,
#84912,#84913,#84914,#84915,#84916,#84917,#84918,#84919,#84920,#84921,#84922,
#84923,#84924,#84925,#84926,#84927,#84928,#84929,#84930,#84931,#84932,#84933,
#84934,#84935,#84936,#84937,#84938,#84939,#84940,#84941,#84942,#84943,#84944,
#84945,#84946,#84947,#84948,#84949,#84950,#84951,#84952,#84953,#84954,#84955,
#84956,#84957,#84958,#84959,#84960,#84961,#84962,#84963,#84964,#84965,#84966,
#84967,#84968,#84969,#84970,#84971,#84972,#84973,#84974,#84975,#84976,#84977,
#84978,#84979,#84980,#84981,#84982,#84983,#84984,#84985,#84986,#84987,#84988,
#84989,#84990,#84991,#84992),.UNSPECIFIED.,.F.,.F.,(4,2,2,2,2,2,2,2,2,2,
2,2,2,2,2,2,2,2,2,2,2,2,2,2,2,2,2,2,2,2,2,2,2,2,2,2,2,2,2,2,2,2,2,2,2,2,
2,2,2,2,2,2,2,2,2,2,2,2,2,2,2,2,2,2,2,2,2,2,2,2,2,2,2,2,2,4),(-1.67609529766553,
-1.64671553914685,-1.61757900798281,-1.59663124306229,-1.58486995679092,
-1.57404350494896,-1.55890499236992,-1.50110180973233,-1.4795265849896,
-1.46515816266859,-1.45810063060918,-1.45184906365944,-1.44175954178262,
-1.41020899241748,-1.3719498655606,-1.35462917073466,-1.33973807254146,
-1.32886447655595,-1.31682811125898,-1.29455574748249,-1.24300901245012,
-1.22590455158308,-1.21355791334137,-1.20681516593851,-1.20020972960133,
-1.18854564067458,-1.13693985211147,-1.10104765354146,-1.08748853903,-1.07675187350426,
-1.0639741421333,-1.03626889690998,-0.985736232314045,-0.966465563951661,
-0.958541460300993,-0.952393138793696,-0.943736788111427,-0.914837267675602,
-0.852507151479367,-0.839533244827146,-0.828616662260341,-0.816853068039929,
-0.796161751914324,-0.767668513762618,-0.718696450045662,-0.709512462908799,
-0.703318801253057,-0.69574917775228,-0.678250055048964,-0.648246585598915,
-0.604153726816397,-0.588788941402707,-0.577872060287989,-0.566061952678386,
-0.545135101238413,-0.516106350454803,-0.468429108519963,-0.459108136308134,
-0.452894153556565,-0.445390943741233,-0.428358716657414,-0.39976905988297,
-0.353548207875082,-0.338224108628993,-0.327316247095225,-0.315499053855471,
-0.294510774400837,-0.265342670852866,-0.217920285619976,-0.20857071567736,
-0.202356004370044,-0.194875823355679,-0.177993703842297,-0.149843235549889,
-0.10290260483124,-0.0902465477143886),.UNSPECIFIED.);
#715=B_SPLINE_CURVE_WITH_KNOTS('',3,(#84998,#84999,#85000,#85001,#85002,
#85003,#85004,#85005,#85006,#85007,#85008,#85009,#85010,#85011,#85012,#85013,
#85014,#85015,#85016,#85017,#85018,#85019,#85020,#85021,#85022,#85023,#85024,
#85025,#85026,#85027,#85028,#85029,#85030,#85031,#85032,#85033,#85034,#85035,
#85036,#85037,#85038,#85039,#85040,#85041,#85042,#85043,#85044,#85045,#85046,
#85047,#85048,#85049,#85050,#85051,#85052,#85053,#85054,#85055,#85056,#85057,
#85058,#85059,#85060,#85061,#85062,#85063,#85064,#85065,#85066,#85067,#85068,
#85069,#85070,#85071,#85072,#85073,#85074,#85075,#85076,#85077,#85078,#85079,
#85080,#85081,#85082,#85083,#85084,#85085,#85086,#85087,#85088,#85089,#85090,
#85091,#85092,#85093,#85094,#85095,#85096,#85097,#85098,#85099,#85100,#85101,
#85102,#85103,#85104,#85105,#85106,#85107,#85108,#85109,#85110,#85111,#85112,
#85113,#85114,#85115,#85116,#85117,#85118,#85119,#85120,#85121,#85122,#85123,
#85124,#85125,#85126,#85127,#85128,#85129,#85130,#85131,#85132,#85133,#85134,
#85135,#85136,#85137,#85138,#85139,#85140,#85141,#85142,#85143,#85144,#85145,
#85146,#85147,#85148,#85149,#85150,#85151,#85152,#85153,#85154,#85155,#85156,
#85157,#85158,#85159,#85160,#85161,#85162,#85163,#85164,#85165,#85166,#85167,
#85168,#85169,#85170,#85171,#85172,#85173,#85174,#85175,#85176,#85177,#85178,
#85179,#85180,#85181),.UNSPECIFIED.,.F.,.F.,(4,3,3,3,3,3,3,3,3,3,3,3,3,
3,3,3,3,3,3,3,3,3,3,3,3,3,3,3,3,3,3,3,3,3,3,3,3,3,3,3,3,3,3,3,3,3,3,3,3,
3,3,3,3,3,3,3,3,3,3,3,3,4),(26.7961973726131,26.8083382968715,26.907424690282,
27.0063712157574,27.105729778197,27.2045008371582,27.3032397040171,27.4019761243891,
27.5017920221104,27.6006696995348,27.7009547074045,27.8012397152742,27.9003266702602,
27.9992737646337,28.0986321857641,28.1974038270813,28.296143280017,28.3948802893619,
28.4946955004406,28.5935737678283,28.6938574507526,28.7941411336768,28.8932250203573,
28.9921690389877,29.0915282281242,29.190296798151,29.2890331882864,29.3877671474404,
29.4875859986002,29.5864612776629,29.6867519148712,29.7870425520795,29.8861308403733,
29.9850792486213,30.0844373388539,30.1832102378347,30.2819509246824,30.3806891426645,
30.4805028496189,30.5793822519147,30.6796631111984,30.7799439704821,30.8790345488744,
30.9779853010793,31.077342812055,31.1761181673173,31.2748613468469,31.3736020902608,
31.4734129149168,31.5722948962214,31.6725701425531,31.7728453888848,31.8712867592265,
31.9695887507089,32.0677794829529,32.1659101501907,32.2640113496284,32.3621136410874,
32.4603104275931,32.5585567870616,32.6569669327387,32.7254896765487),
 .UNSPECIFIED.);
#716=B_SPLINE_CURVE_WITH_KNOTS('',3,(#85182,#85183,#85184,#85185,#85186,
#85187,#85188,#85189,#85190,#85191,#85192,#85193,#85194,#85195,#85196,#85197),
 .UNSPECIFIED.,.F.,.F.,(4,3,3,3,3,4),(32.725489676875,32.7657468072874,
32.8648376936571,32.9638056775635,33.062661762309,33.0799350929859),
 .UNSPECIFIED.);
#717=B_SPLINE_CURVE_WITH_KNOTS('',3,(#85199,#85200,#85201,#85202,#85203,
#85204,#85205,#85206,#85207,#85208,#85209,#85210),.UNSPECIFIED.,.F.,.F.,
(4,2,2,2,2,4),(-0.0902465477143886,-0.0876095400998589,-0.0767075193960174,
-0.0648825206908752,-0.0438360192347396,-0.000729083341957605),
 .UNSPECIFIED.);
#718=B_SPLINE_CURVE_WITH_KNOTS('',3,(#85211,#85212,#85213,#85214,#85215,
#85216,#85217,#85218,#85219,#85220,#85221,#85222,#85223,#85224,#85225,#85226,
#85227,#85228,#85229,#85230,#85231,#85232,#85233,#85234,#85235,#85236,#85237,
#85238,#85239,#85240,#85241,#85242,#85243,#85244,#85245,#85246,#85247,#85248,
#85249,#85250,#85251,#85252,#85253,#85254,#85255,#85256,#85257,#85258,#85259,
#85260,#85261,#85262,#85263,#85264,#85265,#85266,#85267,#85268,#85269,#85270,
#85271,#85272,#85273,#85274,#85275,#85276,#85277,#85278,#85279,#85280,#85281,
#85282,#85283,#85284,#85285,#85286,#85287,#85288,#85289,#85290,#85291,#85292,
#85293,#85294,#85295,#85296,#85297,#85298,#85299,#85300,#85301,#85302,#85303,
#85304,#85305,#85306,#85307,#85308,#85309,#85310,#85311,#85312,#85313,#85314,
#85315,#85316,#85317,#85318,#85319,#85320,#85321,#85322,#85323,#85324,#85325,
#85326,#85327,#85328,#85329,#85330,#85331,#85332,#85333,#85334,#85335,#85336,
#85337,#85338,#85339,#85340,#85341,#85342,#85343,#85344,#85345,#85346,#85347,
#85348,#85349,#85350,#85351,#85352,#85353,#85354,#85355,#85356,#85357,#85358,
#85359,#85360),.UNSPECIFIED.,.F.,.F.,(4,2,2,2,2,2,2,2,2,2,2,2,2,2,2,2,2,
2,2,2,2,2,2,2,2,2,2,2,2,2,2,2,2,2,2,2,2,2,2,2,2,2,2,2,2,2,2,2,2,2,2,2,2,
2,2,2,2,2,2,2,2,2,2,2,2,2,2,2,2,2,2,2,2,2,4),(-3.17269239421731,-3.1418080264104,
-3.13385954589945,-3.12672655156742,-3.12047280516759,-3.1104172371218,
-3.07299620890547,-3.03857721203288,-3.01548585115055,-3.00333909904038,
-2.99252480308098,-2.9779715427723,-2.92308193523701,-2.89900662609222,
-2.88361165360702,-2.87635565952824,-2.87014566122291,-2.86038664063358,
-2.81686173958364,-2.7858454430596,-2.76407706049396,-2.75213363579342,
-2.74126556810184,-2.72625965209991,-2.69116856650147,-2.65413166490487,
-2.63460179508923,-2.62676618807796,-2.6206059931027,-2.61181910365338,
-2.58193611504223,-2.54072680564311,-2.51538698177176,-2.50291729143309,
-2.49215734816347,-2.47841522688553,-2.41842410715263,-2.39645719873271,
-2.3819126630231,-2.37479506001559,-2.36853287548749,-2.35842916883865,
-2.32452674348858,-2.2878831010503,-2.26399844770101,-2.25173309026112,
-2.24094080149394,-2.22686244955933,-2.16941165174081,-2.14641839599599,
-2.13145176960661,-2.12426403664912,-2.11802875825167,-2.10810294433784,
-2.06796256488764,-2.03507111840387,-2.01894162719182,-2.00478194164045,
-1.99400494516425,-1.98164158191672,-1.95707581947592,-1.94344851811339,
-1.90317769083255,-1.88285290838813,-1.87492156667475,-1.86876834808487,
-1.86010465337482,-1.83300344367185,-1.7958742160871,-1.76535200430175,
-1.75225805290813,-1.74153228251082,-1.72833698796303,-1.69978753189247,
-1.67614738790005),.UNSPECIFIED.);
#719=B_SPLINE_CURVE_WITH_KNOTS('',3,(#85366,#85367,#85368,#85369,#85370,
#85371,#85372,#85373,#85374,#85375),.UNSPECIFIED.,.F.,.F.,(4,1,1,1,1,1,
1,4),(20.5123632666524,20.8509297864556,21.8438312048583,22.8367326232609,
23.8296340416636,24.8225354600662,25.8154368784689,26.4423043696954),
 .UNSPECIFIED.);
#720=B_SPLINE_CURVE_WITH_KNOTS('',3,(#85376,#85377,#85378,#85379,#85380,
#85381,#85382,#85383,#85384,#85385,#85386,#85387,#85388),.UNSPECIFIED.,
 .F.,.F.,(4,3,3,3,4),(26.4423043696954,26.5538023203891,26.6658196926276,
26.778442326011,26.7961973726131),.UNSPECIFIED.);
#721=B_SPLINE_CURVE_WITH_KNOTS('',3,(#85389,#85390,#85391,#85392,#85393,
#85394,#85395,#85396,#85397,#85398,#85399,#85400,#85401,#85402,#85403,#85404,
#85405,#85406,#85407,#85408,#85409,#85410,#85411,#85412,#85413,#85414,#85415,
#85416,#85417,#85418,#85419,#85420,#85421,#85422,#85423,#85424,#85425,#85426,
#85427,#85428,#85429,#85430,#85431,#85432,#85433,#85434,#85435,#85436,#85437,
#85438,#85439,#85440,#85441,#85442,#85443,#85444,#85445,#85446,#85447,#85448,
#85449,#85450,#85451,#85452,#85453,#85454,#85455,#85456,#85457,#85458,#85459,
#85460,#85461,#85462,#85463,#85464,#85465,#85466,#85467,#85468,#85469,#85470,
#85471,#85472,#85473,#85474,#85475,#85476,#85477,#85478,#85479,#85480,#85481,
#85482,#85483,#85484,#85485,#85486,#85487,#85488,#85489,#85490,#85491,#85492,
#85493,#85494,#85495,#85496,#85497,#85498,#85499,#85500,#85501,#85502,#85503,
#85504,#85505,#85506,#85507,#85508,#85509,#85510,#85511,#85512,#85513,#85514,
#85515,#85516,#85517,#85518,#85519,#85520,#85521,#85522,#85523,#85524,#85525,
#85526,#85527,#85528,#85529,#85530,#85531,#85532,#85533,#85534,#85535,#85536,
#85537,#85538,#85539,#85540,#85541,#85542,#85543,#85544,#85545,#85546,#85547,
#85548),.UNSPECIFIED.,.F.,.F.,(4,2,2,2,2,2,2,2,2,2,2,2,2,2,2,2,2,2,2,2,
2,2,2,2,2,2,2,2,2,2,2,2,2,2,2,2,2,2,2,2,2,2,2,2,2,2,2,2,2,2,2,2,2,2,2,2,
2,2,2,2,2,2,2,2,2,2,2,2,2,2,2,2,2,2,2,2,2,2,2,4),(-1.67614738790005,-1.65401539803214,
-1.63251200410341,-1.6244494917157,-1.61830380027013,-1.60979962397045,
-1.58696266804934,-1.52960415803192,-1.50957204956521,-1.49790669752566,
-1.48692708081092,-1.47112065152718,-1.45223194399327,-1.40489440322899,
-1.38255080966505,-1.37499656378177,-1.36881636593124,-1.36113055468062,
-1.34278630121307,-1.31005254648512,-1.26959232320727,-1.25432845224904,
-1.24342540625013,-1.23157974231834,-1.21043333302154,-1.1809041913237,
-1.13425114923896,-1.12481474505895,-1.11858677379479,-1.11114565468571,
-1.0945465402581,-1.06722144679975,-1.0188238102491,-1.00360783327805,-0.992711770276206,
-0.980849417064562,-0.959595084991448,-0.929811860271617,-0.883723717419915,
-0.874227982324294,-0.867992659951299,-0.860582344874721,-0.844187932972367,
-0.817438862528606,-0.767998151644771,-0.752861690727202,-0.741976737251043,
-0.730085262520449,-0.70864419881481,-0.678417516809986,-0.633298972396409,
-0.623701712095381,-0.617453115407401,-0.610093002657982,-0.594028063783899,
-0.568185038995766,-0.517001317180073,-0.502024174319338,-0.491160355365596,
-0.479206491575932,-0.457365804191386,-0.426170830491055,-0.383071357672949,
-0.373282689208771,-0.367068994072127,-0.359827730726221,-0.344520787293964,
-0.320668537576263,-0.265214737806784,-0.250726549549183,-0.239920698609147,
-0.227744574156621,-0.204445619843977,-0.169451754272856,-0.133092188794971,
-0.122991416082315,-0.116731032841127,-0.109615614144809,-0.0950760407469734,
-0.0900799055529525),.UNSPECIFIED.);
#722=B_SPLINE_CURVE_WITH_KNOTS('',3,(#85554,#85555,#85556,#85557,#85558,
#85559,#85560,#85561,#85562,#85563,#85564,#85565,#85566,#85567,#85568,#85569,
#85570,#85571,#85572,#85573,#85574,#85575,#85576,#85577,#85578,#85579,#85580,
#85581,#85582,#85583,#85584,#85585,#85586,#85587,#85588,#85589,#85590,#85591,
#85592,#85593,#85594,#85595,#85596,#85597,#85598,#85599,#85600,#85601,#85602,
#85603,#85604,#85605,#85606,#85607,#85608,#85609,#85610,#85611,#85612,#85613,
#85614,#85615,#85616,#85617,#85618,#85619,#85620,#85621,#85622,#85623,#85624,
#85625,#85626,#85627,#85628,#85629,#85630,#85631,#85632,#85633,#85634,#85635,
#85636,#85637,#85638,#85639,#85640,#85641,#85642,#85643,#85644,#85645,#85646,
#85647,#85648,#85649,#85650,#85651,#85652,#85653,#85654,#85655,#85656,#85657,
#85658,#85659,#85660,#85661,#85662,#85663,#85664,#85665,#85666,#85667,#85668,
#85669,#85670,#85671,#85672,#85673,#85674,#85675,#85676,#85677,#85678,#85679,
#85680,#85681,#85682,#85683,#85684,#85685,#85686,#85687,#85688,#85689,#85690,
#85691,#85692,#85693,#85694,#85695,#85696,#85697,#85698,#85699,#85700,#85701,
#85702,#85703,#85704,#85705,#85706,#85707,#85708,#85709,#85710,#85711,#85712,
#85713,#85714,#85715,#85716,#85717,#85718,#85719,#85720,#85721,#85722,#85723,
#85724,#85725,#85726,#85727,#85728,#85729,#85730,#85731,#85732,#85733,#85734),
 .UNSPECIFIED.,.F.,.F.,(4,3,3,3,3,3,3,3,3,3,3,3,3,3,3,3,3,3,3,3,3,3,3,3,
3,3,3,3,3,3,3,3,3,3,3,3,3,3,3,3,3,3,3,3,3,3,3,3,3,3,3,3,3,3,3,3,3,3,3,3,
4),(14.2303481072454,14.3291052935583,14.4278400311323,14.5265820587969,
14.6254260448789,14.7243235468301,14.8233897301623,14.8935212760397,14.992607488937,
15.0915538366193,15.1909124438472,15.2896833328613,15.3884220330811,15.4871582903312,
15.586974391359,15.6858519158902,15.7861373051663,15.8864226944424,15.9855088636077,
16.0844551664509,16.1838137847501,16.2825846265504,16.3813232787667,16.4800594872869,
16.5798756436764,16.6787531181774,16.7790386155112,16.879324112845,16.9784103343415,
17.0773566903575,17.1767152954688,17.2754861920995,17.3742248996474,17.4729611639253,
17.5727772557559,17.6716547864972,17.7719401588725,17.8722255312477,17.9713117348143,
18.0702580727126,18.1696166823298,18.2683875605216,18.3671262495515,18.465862495258,
18.565678608856,18.6645561210849,18.7648415353676,18.8651269496503,18.964213152378,
19.0631594893323,19.1625180991724,19.2612889761701,19.360027663914,19.4587639082443,
19.5585800231964,19.6574575338396,19.7577429509463,19.858028368053,19.9779659443332,
20.0964128674536,20.1591190625159),.UNSPECIFIED.);
#723=B_SPLINE_CURVE_WITH_KNOTS('',3,(#85735,#85736,#85737,#85738),
 .UNSPECIFIED.,.F.,.F.,(4,4),(20.1591190625159,20.5123632666524),
 .UNSPECIFIED.);
#724=B_SPLINE_CURVE_WITH_KNOTS('',3,(#85740,#85741,#85742,#85743,#85744,
#85745,#85746,#85747,#85748,#85749),.UNSPECIFIED.,.F.,.F.,(4,2,2,2,4),(-0.0900799055529525,
-0.0731163611940172,-0.0178336702430842,-0.00796388538298541,-0.00076518352726976),
 .UNSPECIFIED.);
#725=B_SPLINE_CURVE_WITH_KNOTS('',3,(#85750,#85751,#85752,#85753,#85754,
#85755,#85756,#85757,#85758,#85759),.UNSPECIFIED.,.F.,.F.,(4,1,1,1,1,1,
1,4),(-16.4153450200003,-15.8864226944424,-14.8935212760397,-13.9006198576371,
-12.9077184392344,-11.9148170208318,-10.9219156024291,-10.4858137779553),
 .UNSPECIFIED.);
#726=B_SPLINE_CURVE_WITH_KNOTS('',3,(#85765,#85766,#85767,#85768,#85769,
#85770,#85771,#85772,#85773,#85774,#85775,#85776,#85777),.UNSPECIFIED.,
 .F.,.F.,(4,3,3,3,4),(-4.20357446602247,-4.10477053931125,-4.00580655102466,
-3.9716056736106,-3.84897440564113),.UNSPECIFIED.);
#727=B_SPLINE_CURVE_WITH_KNOTS('',3,(#85779,#85780,#85781,#85782,#85783,
#85784,#85785,#85786,#85787,#85788,#85789,#85790,#85791,#85792,#85793,#85794,
#85795,#85796,#85797,#85798,#85799,#85800,#85801,#85802,#85803,#85804,#85805,
#85806,#85807,#85808,#85809,#85810,#85811,#85812,#85813,#85814,#85815,#85816,
#85817,#85818,#85819,#85820,#85821,#85822,#85823,#85824,#85825,#85826,#85827,
#85828,#85829,#85830,#85831,#85832,#85833,#85834,#85835,#85836,#85837,#85838,
#85839,#85840,#85841,#85842,#85843,#85844,#85845,#85846,#85847,#85848,#85849,
#85850,#85851,#85852,#85853,#85854,#85855,#85856,#85857,#85858,#85859,#85860,
#85861,#85862,#85863,#85864,#85865,#85866,#85867,#85868,#85869,#85870,#85871,
#85872,#85873,#85874,#85875,#85876,#85877,#85878,#85879,#85880,#85881,#85882,
#85883,#85884,#85885,#85886,#85887,#85888,#85889,#85890,#85891,#85892,#85893,
#85894,#85895,#85896),.UNSPECIFIED.,.F.,.F.,(4,3,3,3,3,3,3,3,3,3,3,3,3,
3,3,3,3,3,3,3,3,3,3,3,3,3,3,3,3,3,3,3,3,3,3,3,3,3,3,4),(-3.8489744053901,
-3.75118264277131,-3.65352312873579,-3.55593667405005,-3.45839204708363,
-3.36085806901283,-3.26323998878766,-3.16558169918367,-3.06775705625276,
-2.97870425520795,-2.87951180797405,-2.78045709200363,-2.68112531010384,
-2.58224174811673,-2.48338902857077,-2.38453757659689,-2.284853891649,-2.18585953093757,
-2.08583118387143,-1.9858028368053,-1.88771151482969,-1.78976053950896,
-1.69015314937067,-1.59237218731071,-1.49461946688772,-1.39686408539742,
-1.29587341864873,-1.19795464897449,-1.09542803368857,-0.992901418402651,
-0.891124553118223,-0.789507061012913,-0.68804880427994,-0.58668428904758,
-0.485389203973641,-0.384139316452674,-0.282881003294853,-0.181624333840912,
-0.0802946514713979,0.),.UNSPECIFIED.);
#728=B_SPLINE_CURVE_WITH_KNOTS('',3,(#85900,#85901,#85902,#85903,#85904,
#85905,#85906,#85907,#85908,#85909,#85910,#85911,#85912,#85913,#85914,#85915,
#85916,#85917,#85918,#85919,#85920,#85921,#85922,#85923,#85924,#85925,#85926,
#85927,#85928,#85929,#85930,#85931,#85932,#85933,#85934,#85935,#85936,#85937,
#85938,#85939,#85940,#85941,#85942,#85943,#85944,#85945,#85946,#85947,#85948,
#85949,#85950,#85951,#85952,#85953,#85954,#85955,#85956,#85957,#85958,#85959,
#85960,#85961,#85962,#85963,#85964,#85965,#85966,#85967,#85968,#85969,#85970,
#85971,#85972,#85973,#85974,#85975,#85976,#85977,#85978,#85979,#85980,#85981,
#85982,#85983,#85984,#85985,#85986,#85987,#85988,#85989,#85990,#85991,#85992,
#85993,#85994,#85995,#85996,#85997,#85998,#85999,#86000,#86001,#86002,#86003,
#86004,#86005,#86006,#86007,#86008,#86009,#86010,#86011,#86012,#86013,#86014,
#86015,#86016,#86017,#86018,#86019,#86020,#86021,#86022,#86023,#86024,#86025,
#86026,#86027,#86028,#86029,#86030,#86031,#86032,#86033,#86034,#86035,#86036,
#86037,#86038,#86039,#86040,#86041,#86042,#86043,#86044,#86045,#86046,#86047,
#86048,#86049,#86050,#86051,#86052,#86053,#86054,#86055,#86056,#86057,#86058,
#86059,#86060,#86061,#86062,#86063,#86064,#86065,#86066,#86067,#86068,#86069,
#86070,#86071),.UNSPECIFIED.,.F.,.F.,(4,3,3,3,3,3,3,3,3,3,3,3,3,3,3,3,3,
3,3,3,3,3,3,3,3,3,3,3,3,3,3,3,3,3,3,3,3,3,3,3,3,3,3,3,3,3,3,3,3,3,3,3,3,
3,3,3,3,4),(2.01695735912304,2.11562654140827,2.21415701847924,2.31257667970888,
2.41093631520768,2.50926624683899,2.60759675934576,2.70602208019458,2.80449599663101,
2.90313645744952,2.97870425520795,3.07795276095063,3.17706471441973,3.27638233431859,
3.37532565237687,3.47423895872607,3.57315175917927,3.6727652377871,3.77182225845132,
3.87171396603096,3.9716056736106,4.07057367524206,4.16940014596475,4.26878851422081,
4.36743633982893,4.46605104956199,4.56466255416582,4.66462368862768,4.76337584074457,
4.86394146637891,4.96450709201324,5.06361700642839,5.16258714977056,5.26193981985123,
5.36073455159112,5.45949705750217,5.55825704998521,5.65804491509288,5.75694575497821,
5.85717713269705,5.95740851041589,6.05651259099809,6.15547719813649,6.25483128947175,
6.35362125932815,6.45237930714439,6.55113515295565,6.65092884692138,6.749826355645,
6.85006814223177,6.95030992881854,7.04969426096498,7.14893793290924,7.24807038953629,
7.34711985275463,7.44612071151953,7.5451203572188,7.59274844815668),
 .UNSPECIFIED.);
#729=B_SPLINE_CURVE_WITH_KNOTS('',3,(#86072,#86073,#86074,#86075,#86076,
#86077,#86078,#86079,#86080,#86081,#86082,#86083,#86084),.UNSPECIFIED.,
 .F.,.F.,(4,3,3,3,4),(7.59274844852451,7.70563133194379,7.82442133958249,
7.94321134722119,7.94673310592174),.UNSPECIFIED.);
#730=B_SPLINE_CURVE_WITH_KNOTS('',3,(#86087,#86088,#86089,#86090,#86091,
#86092,#86093,#86094,#86095,#86096,#86097,#86098,#86099,#86100,#86101,#86102,
#86103,#86104,#86105,#86106,#86107,#86108,#86109,#86110,#86111,#86112,#86113,
#86114,#86115,#86116,#86117,#86118,#86119,#86120,#86121,#86122,#86123,#86124,
#86125,#86126,#86127,#86128,#86129,#86130,#86131,#86132,#86133,#86134,#86135,
#86136,#86137,#86138,#86139,#86140,#86141,#86142,#86143,#86144,#86145,#86146,
#86147,#86148,#86149,#86150,#86151,#86152,#86153,#86154,#86155,#86156,#86157,
#86158,#86159,#86160,#86161,#86162,#86163,#86164,#86165,#86166,#86167,#86168,
#86169,#86170,#86171,#86172,#86173,#86174,#86175,#86176,#86177,#86178,#86179,
#86180,#86181,#86182,#86183,#86184,#86185,#86186,#86187,#86188,#86189,#86190,
#86191,#86192,#86193,#86194,#86195,#86196,#86197,#86198,#86199,#86200,#86201,
#86202,#86203,#86204,#86205,#86206,#86207,#86208,#86209,#86210,#86211,#86212,
#86213,#86214,#86215,#86216,#86217,#86218,#86219,#86220,#86221,#86222,#86223,
#86224,#86225,#86226,#86227,#86228,#86229,#86230,#86231,#86232,#86233,#86234,
#86235,#86236,#86237,#86238,#86239,#86240,#86241,#86242,#86243,#86244,#86245,
#86246,#86247,#86248,#86249,#86250,#86251,#86252,#86253,#86254,#86255,#86256,
#86257,#86258,#86259,#86260,#86261,#86262,#86263,#86264,#86265,#86266,#86267),
 .UNSPECIFIED.,.F.,.F.,(4,3,3,3,3,3,3,3,3,3,3,3,3,3,3,3,3,3,3,3,3,3,3,3,
3,3,3,3,3,3,3,3,3,3,3,3,3,3,3,3,3,3,3,3,3,3,3,3,3,3,3,3,3,3,3,3,3,3,3,3,
4),(7.94673310592174,8.04581817646567,8.14476459328382,8.24368311482633,
8.34245702765183,8.44119968485212,8.53994082527461,8.63898381036192,8.73786714282491,
8.83698995422438,8.93611276562384,9.03520077646614,9.1341489668641,9.2335071190094,
9.33227994653866,9.43102061705201,9.52975887377632,9.62957270133887,9.728452277143,
9.82873323058475,9.92901418402649,10.0280982190887,10.127042354227,10.2264015102523,
10.3251701184937,10.4239065173681,10.5226404558074,10.6224592424628,10.7213344287368,
10.8216250155829,10.9219156024291,11.0210025472156,11.1199496335807,11.2193080569871,
11.3180796956776,11.4168191480129,11.515556158782,11.6153713742944,11.7142496480606,
11.8145333344462,11.9148170208318,12.0139033809216,12.112849880234,12.2122084501091,
12.310979500489,12.4097183653858,12.5084547904101,12.6082707026162,12.7071484008778,
12.8074334200561,12.9077184392344,13.006397200346,13.1049363913014,13.2033637313469,
13.3017302940464,13.4000663981463,13.498402324608,13.5968336628894,13.6953128615516,
13.7939621905588,13.8759337551205),.UNSPECIFIED.);
#731=B_SPLINE_CURVE_WITH_KNOTS('',3,(#86268,#86269,#86270,#86271,#86272,
#86273,#86274,#86275,#86276,#86277,#86278,#86279,#86280,#86281,#86282,#86283),
 .UNSPECIFIED.,.F.,.F.,(4,3,3,3,3,4),(13.8759337553363,13.9006198576371,
13.9996876770314,14.0986328228261,14.1974668341838,14.2303481072454),
 .UNSPECIFIED.);
#732=B_SPLINE_CURVE_WITH_KNOTS('',3,(#86285,#86286,#86287,#86288),
 .UNSPECIFIED.,.F.,.F.,(4,4),(-10.4858137779553,-10.132162382237),
 .UNSPECIFIED.);
#733=B_SPLINE_CURVE_WITH_KNOTS('',3,(#86289,#86290,#86291,#86292,#86293,
#86294,#86295,#86296,#86297,#86298,#86299,#86300,#86301,#86302,#86303,#86304,
#86305,#86306,#86307,#86308,#86309,#86310,#86311,#86312,#86313,#86314,#86315,
#86316,#86317,#86318,#86319,#86320,#86321,#86322,#86323,#86324,#86325,#86326,
#86327,#86328,#86329,#86330,#86331,#86332,#86333,#86334,#86335,#86336,#86337,
#86338,#86339,#86340,#86341,#86342,#86343,#86344,#86345,#86346,#86347,#86348,
#86349,#86350,#86351,#86352,#86353,#86354,#86355,#86356,#86357,#86358,#86359,
#86360,#86361,#86362,#86363,#86364,#86365,#86366,#86367,#86368,#86369,#86370,
#86371,#86372,#86373,#86374,#86375,#86376,#86377,#86378,#86379,#86380,#86381,
#86382,#86383,#86384,#86385,#86386,#86387,#86388,#86389,#86390,#86391,#86392,
#86393,#86394,#86395,#86396,#86397,#86398,#86399,#86400,#86401,#86402,#86403,
#86404,#86405,#86406,#86407,#86408,#86409,#86410,#86411,#86412,#86413,#86414,
#86415,#86416,#86417,#86418,#86419,#86420,#86421,#86422,#86423,#86424,#86425,
#86426,#86427,#86428,#86429,#86430,#86431,#86432,#86433,#86434,#86435,#86436,
#86437,#86438,#86439,#86440,#86441,#86442,#86443,#86444,#86445,#86446,#86447,
#86448,#86449,#86450,#86451,#86452,#86453,#86454,#86455,#86456,#86457,#86458,
#86459,#86460,#86461,#86462,#86463,#86464,#86465,#86466,#86467,#86468,#86469),
 .UNSPECIFIED.,.F.,.F.,(4,3,3,3,3,3,3,3,3,3,3,3,3,3,3,3,3,3,3,3,3,3,3,3,
3,3,3,3,3,3,3,3,3,3,3,3,3,3,3,3,3,3,3,3,3,3,3,3,3,3,3,3,3,3,3,3,3,3,3,3,
4),(-10.1321597128207,-9.99259860333552,-9.9290141840265,-9.82992590631703,
-9.73097750849788,-9.63161941563862,-9.53284652663874,-9.43410584958342,
-9.3353676411932,-9.23555392230086,-9.13667452901384,-9.03639364731884,
-8.93611276562384,-8.83702224548506,-8.73807155189518,-8.63871402631093,
-8.53993873010981,-8.4411956096771,-8.34245492531528,-8.24264403079176,
-8.14376210782866,-8.04348672752493,-7.9432113472212,-7.84414223683077,
-7.74521302140415,-7.64585013483095,-7.54709632547949,-7.44837464743071,
-7.34965533209489,-7.2498189812758,-7.15095803039816,-7.05063397960835,
-6.95030992881855,-6.85120368873458,-6.75223740083337,-6.65288378953119,
-6.55409331422877,-6.45533520337683,-6.35657973652944,-6.25678693000106,
-6.15789088086669,-6.05764969564129,-5.95740851041589,-5.85829983722156,
-5.75933073268631,-5.65997777760218,-5.56118358533646,-5.46242143021034,
-5.36366159955868,-5.26387297267232,-5.16497182938891,-5.06473946070108,
-4.96450709201325,-4.86557200000987,-4.76676516593899,-4.66805645652568,
-4.56941584216026,-4.47078819908846,-4.37217137319955,-4.2734867160408,
-4.20357446602247),.UNSPECIFIED.);
#734=B_SPLINE_CURVE_WITH_KNOTS('',3,(#86472,#86473,#86474,#86475,#86476,
#86477,#86478,#86479,#86480,#86481,#86482,#86483,#86484,#86485,#86486,#86487,
#86488,#86489,#86490,#86491,#86492,#86493,#86494,#86495,#86496,#86497,#86498,
#86499,#86500,#86501,#86502,#86503,#86504,#86505,#86506,#86507,#86508,#86509,
#86510,#86511,#86512,#86513,#86514,#86515,#86516,#86517,#86518,#86519,#86520,
#86521,#86522,#86523,#86524,#86525,#86526,#86527,#86528,#86529,#86530,#86531,
#86532,#86533,#86534,#86535,#86536,#86537,#86538,#86539,#86540,#86541,#86542,
#86543,#86544,#86545,#86546,#86547,#86548,#86549,#86550,#86551,#86552,#86553,
#86554,#86555,#86556,#86557,#86558,#86559,#86560,#86561,#86562,#86563,#86564,
#86565,#86566,#86567,#86568,#86569,#86570,#86571,#86572,#86573,#86574,#86575,
#86576,#86577,#86578,#86579,#86580,#86581,#86582,#86583,#86584,#86585,#86586,
#86587,#86588,#86589,#86590,#86591,#86592,#86593,#86594,#86595,#86596,#86597,
#86598,#86599,#86600,#86601,#86602,#86603,#86604,#86605,#86606,#86607,#86608,
#86609,#86610,#86611,#86612,#86613,#86614,#86615,#86616,#86617,#86618,#86619,
#86620,#86621,#86622,#86623,#86624,#86625,#86626,#86627,#86628,#86629,#86630,
#86631,#86632,#86633,#86634,#86635,#86636,#86637,#86638,#86639,#86640,#86641,
#86642,#86643,#86644,#86645,#86646,#86647,#86648,#86649,#86650,#86651,#86652),
 .UNSPECIFIED.,.F.,.F.,(4,3,3,3,3,3,3,3,3,3,3,3,3,3,3,3,3,3,3,3,3,3,3,3,
3,3,3,3,3,3,3,3,3,3,3,3,3,3,3,3,3,3,3,3,3,3,3,3,3,3,3,3,3,3,3,3,3,3,3,3,
4),(7.94673289122112,8.04581792837314,8.14476431138301,8.24368286816311,
8.34245674641829,8.44119936884877,8.53994047434931,8.63898354716794,8.73786684476973,
8.83698980519679,8.93611276562385,9.03520077148316,9.13414895672167,9.23350711013477,
9.33227993210958,9.43102059693156,9.52975884783475,9.62957268188268,9.72845225160275,
9.82873321781462,9.92901418402649,10.0280982326817,10.1270423816281,10.2264015342282,
10.325170156701,10.4239065699343,10.5226405228411,10.6224592927381,10.7213344936009,
10.821625048015,10.9219156024291,11.0210025407565,11.1199496205909,11.219308045621,
11.3180796776554,11.4168191233022,11.5155561273596,11.6153713507277,11.7142496177934,
11.8145333193126,11.9148170208318,12.0139033805419,12.1128498794499,12.212208449423,
12.3109794993409,12.4097183637549,12.5084547882763,12.6082707010158,12.7071483987294,
12.8074334189819,12.9077184392344,13.0063972024842,13.1049363956126,13.2033637378739,
13.301730302815,13.4000664091795,13.4984023379264,13.5968336785102,13.6953128794884,
13.7939622108089,13.8759337551205),.UNSPECIFIED.);
#735=B_SPLINE_CURVE_WITH_KNOTS('',3,(#86653,#86654,#86655,#86656,#86657,
#86658,#86659,#86660,#86661,#86662,#86663,#86664,#86665,#86666,#86667,#86668),
 .UNSPECIFIED.,.F.,.F.,(4,3,3,3,3,4),(13.8759337553363,13.9006198576371,
13.9996876759034,14.0986328205549,14.1974668307429,14.2303478778739),
 .UNSPECIFIED.);
#736=B_SPLINE_CURVE_WITH_KNOTS('',3,(#86670,#86671,#86672,#86673),
 .UNSPECIFIED.,.F.,.F.,(4,4),(-10.4858135521078,-10.1321623805438),
 .UNSPECIFIED.);
#737=B_SPLINE_CURVE_WITH_KNOTS('',3,(#86674,#86675,#86676,#86677,#86678,
#86679,#86680,#86681,#86682,#86683,#86684,#86685,#86686,#86687,#86688,#86689,
#86690,#86691,#86692,#86693,#86694,#86695,#86696,#86697,#86698,#86699,#86700,
#86701,#86702,#86703,#86704,#86705,#86706,#86707,#86708,#86709,#86710,#86711,
#86712,#86713,#86714,#86715,#86716,#86717,#86718,#86719,#86720,#86721,#86722,
#86723,#86724,#86725,#86726,#86727,#86728,#86729,#86730,#86731,#86732,#86733,
#86734,#86735,#86736,#86737,#86738,#86739,#86740,#86741,#86742,#86743,#86744,
#86745,#86746,#86747,#86748,#86749,#86750,#86751,#86752,#86753,#86754,#86755,
#86756,#86757,#86758,#86759,#86760,#86761,#86762,#86763,#86764,#86765,#86766,
#86767,#86768,#86769,#86770,#86771,#86772,#86773,#86774,#86775,#86776,#86777,
#86778,#86779,#86780,#86781,#86782,#86783,#86784,#86785,#86786,#86787,#86788,
#86789,#86790,#86791,#86792,#86793,#86794,#86795,#86796,#86797,#86798,#86799,
#86800,#86801,#86802,#86803,#86804,#86805,#86806,#86807,#86808,#86809,#86810,
#86811,#86812,#86813,#86814,#86815,#86816,#86817,#86818,#86819,#86820,#86821,
#86822,#86823,#86824,#86825,#86826,#86827,#86828,#86829,#86830,#86831,#86832,
#86833,#86834,#86835,#86836,#86837,#86838,#86839,#86840,#86841,#86842,#86843,
#86844,#86845,#86846,#86847,#86848,#86849,#86850,#86851,#86852,#86853,#86854),
 .UNSPECIFIED.,.F.,.F.,(4,3,3,3,3,3,3,3,3,3,3,3,3,3,3,3,3,3,3,3,3,3,3,3,
3,3,3,3,3,3,3,3,3,3,3,3,3,3,3,3,3,3,3,3,3,3,3,3,3,3,3,3,3,3,3,3,3,3,3,3,
4),(-10.1321597128207,-9.99259863041052,-9.9290141840265,-9.82992590097336,
-9.73097749788903,-9.63161940635588,-9.53284651231657,-9.43410583031699,
-9.33536761708367,-9.23555390421872,-9.13667450638263,-9.03639363600324,
-8.93611276562384,-8.83702221611555,-8.73807149297398,-8.63871397475489,
-8.53993864877712,-8.44119549854981,-8.34245478441589,-8.24264392511722,
-8.14376197274035,-8.04348665998078,-7.9432113472212,-7.84414230710637,
-7.74521316205596,-7.64585025790128,-7.54709651866685,-7.44837491048508,
-7.3496556646746,-7.24981923071059,-7.15095834782461,-7.05063413832158,
-6.95030992881855,-6.8512036523718,-6.75223732846605,-6.65288372620978,
-6.55409321601646,-6.45533507076485,-6.35657957005115,-6.25678680514234,
-6.15789072377564,-6.05764961709577,-5.9574085104159,-5.8582996906847,-5.75933043866179,
-5.65997752033072,-5.5611831793623,-5.46242087541135,-5.36366089601644,
-5.26387244501564,-5.16497115470896,-5.0647391233611,-4.96450709201325,
-4.86557234860677,-4.76676586361448,-4.66805750331981,-4.56941723767383,
-4.47078994099785,-4.37217346045678,-4.27348914445664,-4.20357440982612),
 .UNSPECIFIED.);
#738=B_SPLINE_CURVE_WITH_KNOTS('',3,(#86857,#86858,#86859,#86860,#86861,
#86862,#86863,#86864),.UNSPECIFIED.,.F.,.F.,(4,1,1,1,1,4),(17.934417062947,
18.8092987911264,19.802200209529,20.7951016279317,21.7880030463343,21.9911485751285),
 .UNSPECIFIED.);
#739=B_SPLINE_CURVE_WITH_KNOTS('',3,(#86865,#86866,#86867,#86868,#86869,
#86870,#86871,#86872,#86873,#86874,#86875,#86876,#86877,#86878,#86879,#86880,
#86881,#86882,#86883,#86884,#86885,#86886,#86887,#86888,#86889,#86890,#86891,
#86892,#86893,#86894,#86895,#86896,#86897,#86898,#86899,#86900,#86901,#86902,
#86903,#86904,#86905,#86906,#86907,#86908,#86909,#86910,#86911,#86912,#86913,
#86914,#86915,#86916,#86917,#86918,#86919,#86920,#86921,#86922,#86923,#86924,
#86925,#86926,#86927,#86928,#86929,#86930,#86931,#86932,#86933,#86934,#86935,
#86936,#86937,#86938,#86939,#86940),.UNSPECIFIED.,.F.,.F.,(4,3,3,3,3,3,
3,3,3,3,3,3,3,3,3,3,3,3,3,3,3,3,3,3,3,4),(21.9911485751285,22.0839073590714,
22.1765824116993,22.2692136891438,22.3618281746274,22.4544528291803,22.5471704847007,
22.6399399937748,22.7328552617387,22.780904464737,22.8751694663624,22.9693071643559,
23.0633460667357,23.1573182064377,23.2512564850146,23.3451865167536,23.4391339018238,
23.5331822013363,23.6272862468957,23.7215409230576,23.7738058831396,23.8680772171186,
23.9621978437796,24.0562310887038,24.1502000668644,24.2171289178558),
 .UNSPECIFIED.);
#740=B_SPLINE_CURVE_WITH_KNOTS('',3,(#86942,#86943,#86944,#86945,#86946,
#86947),.UNSPECIFIED.,.F.,.F.,(4,1,1,4),(21.9911557963905,22.3416114741931,
23.3345128925957,24.2163566964775),.UNSPECIFIED.);
#741=B_SPLINE_CURVE_WITH_KNOTS('',3,(#86948,#86949,#86950,#86951,#86952,
#86953,#86954,#86955,#86956,#86957,#86958,#86959,#86960,#86961,#86962,#86963,
#86964,#86965,#86966,#86967,#86968,#86969,#86970,#86971,#86972,#86973,#86974,
#86975,#86976,#86977,#86978,#86979,#86980,#86981,#86982,#86983,#86984,#86985,
#86986,#86987,#86988,#86989,#86990,#86991,#86992,#86993,#86994,#86995,#86996,
#86997,#86998,#86999,#87000,#87001,#87002,#87003,#87004,#87005,#87006,#87007,
#87008,#87009,#87010,#87011,#87012,#87013,#87014,#87015,#87016,#87017,#87018,
#87019,#87020,#87021,#87022,#87023,#87024,#87025,#87026,#87027,#87028,#87029,
#87030,#87031,#87032,#87033,#87034,#87035,#87036,#87037,#87038,#87039,#87040,
#87041,#87042,#87043,#87044,#87045,#87046,#87047,#87048,#87049,#87050,#87051,
#87052,#87053,#87054,#87055,#87056,#87057,#87058,#87059,#87060,#87061,#87062,
#87063,#87064,#87065,#87066,#87067,#87068,#87069,#87070,#87071,#87072,#87073,
#87074,#87075,#87076,#87077,#87078,#87079,#87080,#87081,#87082,#87083),
 .UNSPECIFIED.,.F.,.F.,(4,3,3,3,3,3,3,3,3,3,3,3,3,3,3,3,3,3,3,3,3,3,3,3,
3,3,3,3,3,3,3,3,3,3,3,3,3,3,3,3,3,3,3,3,3,4),(17.933562797591,18.027675652425,
18.1218896239166,18.2161582961348,18.3105802127554,18.3700058005825,18.4641580180287,
18.5581814190289,18.6521046770886,18.7459596395798,18.8397798343671,18.9335910183375,
19.0274189336518,19.121347534599,19.2153315750444,19.309466936441,19.3629072189851,
19.4571939175188,19.5513533907898,19.6454141155,19.7394080541651,19.8333681083284,
19.9273198645896,20.0212888953817,20.1153585868841,20.2094839117571,20.3037594805915,
20.3558086373878,20.4500899121047,20.5442442313676,20.6383000780776,20.73228957412,
20.8262454576189,20.9201933215444,21.0141587449332,21.1082252887648,21.2023477218278,
21.2966208318784,21.3487100557904,21.4432580465324,21.5376780899157,21.6319955406164,
21.7262338036894,21.8204240372999,21.914613503733,21.9911485751285),
 .UNSPECIFIED.);
#742=B_SPLINE_CURVE_WITH_KNOTS('',3,(#87086,#87087,#87088,#87089,#87090,
#87091,#87092,#87093),.UNSPECIFIED.,.F.,.F.,(4,1,1,1,1,4),(17.9344169320433,
18.8092987911264,19.802200209529,20.7951016279317,21.7880030463343,21.9911485751285),
 .UNSPECIFIED.);
#743=B_SPLINE_CURVE_WITH_KNOTS('',3,(#87094,#87095,#87096,#87097,#87098,
#87099,#87100,#87101,#87102,#87103,#87104,#87105,#87106,#87107,#87108,#87109,
#87110,#87111,#87112,#87113,#87114,#87115,#87116,#87117,#87118,#87119,#87120,
#87121,#87122,#87123,#87124,#87125,#87126,#87127,#87128,#87129,#87130,#87131,
#87132,#87133,#87134,#87135,#87136,#87137,#87138,#87139,#87140,#87141,#87142,
#87143,#87144,#87145,#87146,#87147,#87148,#87149,#87150,#87151,#87152,#87153,
#87154,#87155,#87156,#87157,#87158,#87159,#87160,#87161,#87162,#87163,#87164,
#87165,#87166,#87167,#87168,#87169),.UNSPECIFIED.,.F.,.F.,(4,3,3,3,3,3,
3,3,3,3,3,3,3,3,3,3,3,3,3,3,3,3,3,3,3,4),(21.9911485751285,22.0839073709794,
22.1765824356426,22.2692137252015,22.3618282228698,22.4544528896688,22.5471705574739,
22.6399400788727,22.7328553591282,22.780904464737,22.8751694611138,22.9693071538032,
23.0633460508314,23.157318185133,23.2512564582814,23.3451864845702,23.4391338641752,
23.5331821582336,23.6272861983369,23.7215408690931,23.7738058831396,23.8680772168287,
23.9621978431654,24.056231087749,24.1502000655167,24.2171287697742),
 .UNSPECIFIED.);
#744=B_SPLINE_CURVE_WITH_KNOTS('',3,(#87171,#87172,#87173,#87174,#87175,
#87176),.UNSPECIFIED.,.F.,.F.,(4,1,1,4),(21.9911557978734,22.3416114741931,
23.3345128925957,24.2163565526082),.UNSPECIFIED.);
#745=B_SPLINE_CURVE_WITH_KNOTS('',3,(#87177,#87178,#87179,#87180,#87181,
#87182,#87183,#87184,#87185,#87186,#87187,#87188,#87189,#87190,#87191,#87192,
#87193,#87194,#87195,#87196,#87197,#87198,#87199,#87200,#87201,#87202,#87203,
#87204,#87205,#87206,#87207,#87208,#87209,#87210,#87211,#87212,#87213,#87214,
#87215,#87216,#87217,#87218,#87219,#87220,#87221,#87222,#87223,#87224,#87225,
#87226,#87227,#87228,#87229,#87230,#87231,#87232,#87233,#87234,#87235,#87236,
#87237,#87238,#87239,#87240,#87241,#87242,#87243,#87244,#87245,#87246,#87247,
#87248,#87249,#87250,#87251,#87252,#87253,#87254,#87255,#87256,#87257,#87258,
#87259,#87260,#87261,#87262,#87263,#87264,#87265,#87266,#87267,#87268,#87269,
#87270,#87271,#87272,#87273,#87274,#87275,#87276,#87277,#87278,#87279,#87280,
#87281,#87282,#87283,#87284,#87285,#87286,#87287,#87288,#87289,#87290,#87291,
#87292,#87293,#87294,#87295,#87296,#87297,#87298,#87299,#87300,#87301,#87302,
#87303,#87304,#87305,#87306,#87307,#87308,#87309,#87310,#87311,#87312),
 .UNSPECIFIED.,.F.,.F.,(4,3,3,3,3,3,3,3,3,3,3,3,3,3,3,3,3,3,3,3,3,3,3,3,
3,3,3,3,3,3,3,3,3,3,3,3,3,3,3,3,3,3,3,3,3,4),(17.9335626655157,18.0276756704584,
18.1218897949067,18.2161586217505,18.310580694799,18.3700058005825,18.4641576524374,
18.5581806828801,18.6521035659322,18.7459581482699,18.8397779598427,18.9335887579803,
19.0274162852848,19.1213444971949,19.2153281474366,19.3094631205816,19.3629072189851,
19.4571940776216,19.551353712538,19.6454146002015,19.7394087030847,19.8333689221839,
19.9273208438937,20.0212900404422,20.1153598971617,20.2094853871854,20.3037611194529,
20.3558086373878,20.4500899460874,20.5442443002541,20.6383001827375,20.7322897157095,
20.8262456368411,20.9201935390591,21.0141590013572,21.1082255848112,21.2023480579584,
21.2966212084346,21.3487100557904,21.4432579779742,21.537677951789,21.6319953320113,
21.7262335235201,21.8204236849522,21.9146130786406,21.9911485751285),
 .UNSPECIFIED.);
#746=B_SPLINE_CURVE_WITH_KNOTS('',3,(#87486,#87487,#87488,#87489,#87490,
#87491,#87492,#87493,#87494,#87495,#87496,#87497,#87498,#87499,#87500,#87501,
#87502,#87503,#87504,#87505,#87506,#87507,#87508,#87509,#87510,#87511,#87512,
#87513,#87514,#87515,#87516,#87517,#87518,#87519,#87520,#87521,#87522,#87523,
#87524,#87525,#87526,#87527,#87528,#87529,#87530,#87531,#87532,#87533,#87534,
#87535,#87536,#87537,#87538,#87539,#87540,#87541,#87542,#87543,#87544,#87545,
#87546,#87547,#87548,#87549,#87550,#87551,#87552,#87553,#87554,#87555,#87556,
#87557,#87558,#87559,#87560,#87561,#87562,#87563,#87564,#87565,#87566,#87567,
#87568,#87569,#87570,#87571,#87572,#87573,#87574,#87575,#87576),
 .UNSPECIFIED.,.F.,.F.,(4,3,3,3,3,3,3,3,3,3,3,3,3,3,3,3,3,3,3,3,3,3,3,3,
3,3,3,3,3,3,4),(0.,0.0300159935056151,0.0604743500360521,0.0909579961729321,
0.11495774109072,0.120628826798375,0.150390662795823,0.179990444032073,
0.208918759997128,0.22052111292651,0.229057706928878,0.233702755111811,
0.26200301285018,0.290174366185419,0.294101824832485,0.323060492781776,
0.339554831971467,0.343320212454064,0.371322118638722,0.399422729592019,
0.427289788372197,0.437570748201759,0.44383438261869,0.448938125741618,
0.476009686934302,0.498103681939219,0.50628921912477,0.511794812399658,
0.537727274345166,0.561316539907562,0.569248610399424),.UNSPECIFIED.);
#747=B_SPLINE_CURVE_WITH_KNOTS('',3,(#87577,#87578,#87579,#87580,#87581,
#87582,#87583,#87584,#87585,#87586,#87587,#87588,#87589,#87590,#87591,#87592,
#87593,#87594,#87595,#87596,#87597,#87598,#87599,#87600,#87601,#87602,#87603,
#87604,#87605,#87606,#87607,#87608,#87609,#87610,#87611,#87612,#87613,#87614,
#87615,#87616,#87617,#87618,#87619,#87620,#87621,#87622,#87623,#87624,#87625,
#87626,#87627,#87628,#87629,#87630,#87631,#87632,#87633,#87634,#87635,#87636,
#87637,#87638,#87639,#87640,#87641,#87642,#87643,#87644,#87645,#87646,#87647,
#87648,#87649,#87650,#87651,#87652,#87653,#87654,#87655,#87656,#87657,#87658,
#87659,#87660,#87661,#87662,#87663,#87664),.UNSPECIFIED.,.F.,.F.,(4,3,3,
3,3,3,3,3,3,3,3,3,3,3,3,3,3,3,3,3,3,3,3,3,3,3,3,3,3,4),(0.,0.0255422152389494,
0.0516177884235197,0.0783410487135325,0.0899179575897014,0.096618619084006,
0.102681367695304,0.130058793828978,0.157808810247486,0.185592138961451,
0.195924569149338,0.202922297119531,0.206879012885186,0.236200442199667,
0.265521871514148,0.293412035650182,0.309408739020944,0.314635271121598,
0.343053617094055,0.372027540249262,0.401483685393919,0.421616489784836,
0.426693998849235,0.456850944397209,0.481878239127351,0.490063670760061,
0.498374798665562,0.528883352060159,0.557282026181539,0.566784192699823),
 .UNSPECIFIED.);
#748=B_SPLINE_CURVE_WITH_KNOTS('',3,(#87665,#87666,#87667,#87668),
 .UNSPECIFIED.,.F.,.F.,(4,4),(-0.0155024185535969,0.),.UNSPECIFIED.);
#749=B_SPLINE_CURVE_WITH_KNOTS('',3,(#87841,#87842,#87843,#87844,#87845,
#87846,#87847,#87848,#87849,#87850,#87851,#87852,#87853,#87854,#87855,#87856,
#87857,#87858,#87859,#87860,#87861,#87862,#87863,#87864,#87865,#87866,#87867,
#87868,#87869,#87870,#87871,#87872,#87873,#87874,#87875,#87876,#87877,#87878,
#87879,#87880,#87881,#87882,#87883,#87884,#87885,#87886,#87887,#87888,#87889,
#87890,#87891,#87892,#87893,#87894,#87895,#87896,#87897,#87898,#87899,#87900,
#87901,#87902,#87903,#87904,#87905,#87906,#87907,#87908,#87909,#87910,#87911,
#87912,#87913,#87914,#87915,#87916,#87917,#87918,#87919,#87920,#87921,#87922,
#87923,#87924,#87925,#87926,#87927,#87928),.UNSPECIFIED.,.F.,.F.,(4,3,3,
3,3,3,3,3,3,3,3,3,3,3,3,3,3,3,3,3,3,3,3,3,3,3,3,3,3,4),(1.04239282054807E-14,
0.0254572747588063,0.0518172438748224,0.0781772129908385,0.0966186262417464,
0.103162062894422,0.130547954004623,0.158302436395126,0.186083150718936,
0.195924591412827,0.202922307188184,0.206879036916929,0.236200454215543,
0.265521871514156,0.293411964117121,0.302822187650876,0.3094079319206,0.314634984029602,
0.343053229098208,0.372027084515964,0.401483217598252,0.421615452936291,
0.426694040216341,0.456850977316032,0.481878254523113,0.49006368288519,
0.499045747647966,0.529549458312069,0.557282026181566,0.566816216565832),
 .UNSPECIFIED.);
#750=B_SPLINE_CURVE_WITH_KNOTS('',3,(#87929,#87930,#87931,#87932,#87933,
#87934,#87935,#87936,#87937,#87938,#87939,#87940,#87941,#87942,#87943,#87944,
#87945,#87946,#87947,#87948,#87949,#87950,#87951,#87952,#87953,#87954,#87955,
#87956,#87957,#87958,#87959,#87960,#87961,#87962,#87963,#87964,#87965,#87966,
#87967,#87968,#87969,#87970,#87971,#87972,#87973,#87974,#87975,#87976,#87977,
#87978,#87979,#87980,#87981,#87982,#87983,#87984,#87985,#87986,#87987,#87988,
#87989,#87990,#87991,#87992,#87993,#87994,#87995,#87996,#87997,#87998,#87999,
#88000,#88001,#88002,#88003,#88004,#88005,#88006,#88007,#88008,#88009,#88010,
#88011,#88012,#88013,#88014,#88015,#88016,#88017,#88018,#88019),
 .UNSPECIFIED.,.F.,.F.,(4,3,3,3,3,3,3,3,3,3,3,3,3,3,3,3,3,3,3,3,3,3,3,3,
3,3,3,3,3,3,4),(0.,0.0300160900779859,0.0604744914019228,0.0909581108839495,
0.114957874464915,0.120628837064466,0.150390666664299,0.179990414269659,
0.20891869318285,0.220521069668172,0.229057577762524,0.233702774585337,
0.262002994102814,0.290174314790119,0.294101824832485,0.323060497067606,
0.339554809732512,0.343320179866502,0.371322084504482,0.399422690124115,
0.427289724843109,0.437570609423,0.443833557401397,0.448938172443596,0.476009696567213,
0.498103708209085,0.506289235973561,0.511794807845771,0.537727197803124,
0.561316539907572,0.569248610399431),.UNSPECIFIED.);
#751=B_SPLINE_CURVE_WITH_KNOTS('',3,(#88029,#88030,#88031,#88032,#88033,
#88034,#88035,#88036,#88037,#88038,#88039,#88040,#88041,#88042,#88043,#88044,
#88045,#88046,#88047,#88048,#88049,#88050,#88051,#88052,#88053,#88054,#88055,
#88056,#88057,#88058,#88059,#88060,#88061,#88062,#88063,#88064,#88065,#88066,
#88067,#88068,#88069,#88070,#88071,#88072,#88073,#88074,#88075,#88076,#88077,
#88078,#88079,#88080,#88081,#88082,#88083,#88084,#88085,#88086,#88087,#88088,
#88089,#88090,#88091,#88092,#88093,#88094,#88095,#88096,#88097,#88098,#88099,
#88100,#88101,#88102,#88103,#88104,#88105,#88106,#88107,#88108,#88109,#88110,
#88111,#88112,#88113,#88114,#88115,#88116,#88117,#88118,#88119),
 .UNSPECIFIED.,.F.,.F.,(4,3,3,3,3,3,3,3,3,3,3,3,3,3,3,3,3,3,3,3,3,3,3,3,
3,3,3,3,3,3,4),(0.,0.025457205048592,0.0518171512135332,0.0781770973784744,
0.0899179847267486,0.0966186227065892,0.102681367591522,0.129991616367842,
0.157832389105944,0.184687665901973,0.195924580418245,0.202922302220591,
0.206879025059384,0.236200448286765,0.265521871514145,0.29342151830769,
0.302822262870922,0.309408330719355,0.314635125840642,0.343053420777207,
0.372027309636075,0.40148344864646,0.421615965153544,0.426694019602539,
0.456850960866328,0.481878246781235,0.491733467196207,0.498374793580113,
0.528883346995961,0.557282026181531,0.566784188998617),.UNSPECIFIED.);
#752=B_SPLINE_CURVE_WITH_KNOTS('',3,(#88120,#88121,#88122,#88123,#88124,
#88125,#88126,#88127,#88128,#88129,#88130,#88131,#88132,#88133,#88134,#88135,
#88136,#88137,#88138,#88139,#88140,#88141,#88142,#88143,#88144,#88145,#88146,
#88147,#88148,#88149,#88150,#88151,#88152,#88153,#88154,#88155,#88156,#88157,
#88158,#88159,#88160,#88161,#88162,#88163,#88164,#88165,#88166,#88167,#88168,
#88169,#88170,#88171,#88172,#88173,#88174,#88175,#88176,#88177,#88178,#88179,
#88180,#88181,#88182,#88183,#88184,#88185,#88186,#88187,#88188,#88189,#88190,
#88191,#88192,#88193,#88194,#88195,#88196,#88197,#88198,#88199,#88200,#88201,
#88202,#88203,#88204,#88205,#88206,#88207,#88208,#88209,#88210),
 .UNSPECIFIED.,.F.,.F.,(4,3,3,3,3,3,3,3,3,3,3,3,3,3,3,3,3,3,3,3,3,3,3,3,
3,3,3,3,3,3,4),(0.,0.0300160333477477,0.0604744083323999,0.0909580434563729,
0.114957796091441,0.120628831026791,0.150388839258673,0.179796669056497,
0.208512063304176,0.220521095101031,0.229057653709693,0.23370276314254,
0.262003005144642,0.290174345004673,0.294101824832486,0.323048758434001,
0.339554822814053,0.343320199032514,0.371322104568047,0.399422713338306,
0.42728976222237,0.437570691067827,0.443834042831826,0.448938144811474,
0.476009690744306,0.498103692666017,0.506289225879212,0.511794810465465,
0.537727242743261,0.561316539907572,0.569248610399431),.UNSPECIFIED.);
#753=B_SPLINE_CURVE_WITH_KNOTS('',3,(#88386,#88387,#88388,#88389,#88390,
#88391,#88392,#88393,#88394,#88395,#88396,#88397,#88398,#88399,#88400,#88401,
#88402,#88403,#88404,#88405,#88406,#88407,#88408,#88409,#88410,#88411,#88412,
#88413,#88414,#88415,#88416,#88417,#88418,#88419,#88420,#88421,#88422,#88423,
#88424,#88425,#88426,#88427,#88428,#88429,#88430,#88431,#88432,#88433,#88434,
#88435,#88436,#88437,#88438,#88439,#88440,#88441,#88442,#88443,#88444,#88445,
#88446,#88447,#88448,#88449,#88450,#88451,#88452,#88453,#88454,#88455,#88456,
#88457,#88458,#88459,#88460,#88461,#88462,#88463,#88464,#88465,#88466,#88467,
#88468,#88469,#88470,#88471,#88472,#88473,#88474,#88475,#88476),
 .UNSPECIFIED.,.F.,.F.,(4,3,3,3,3,3,3,3,3,3,3,3,3,3,3,3,3,3,3,3,3,3,3,3,
3,3,3,3,3,3,4),(0.,0.030016042371606,0.0604744215895692,0.0909580542444513,
0.114957808579322,0.120628831988276,0.150388840111643,0.17979666618708,
0.2085120615786,0.220521091051168,0.229057641618228,0.233702764936734,0.262003003352699,
0.290174340161946,0.294101824832484,0.32306049493075,0.339554820728239,
0.343320195973592,0.371362527908372,0.399540213697088,0.427306356009437,
0.437570678055961,0.443833965453209,0.448938149214107,0.47703274688747,
0.498103695142492,0.506289227485511,0.512902840722385,0.538820003579557,
0.561316539907558,0.56924861039942),.UNSPECIFIED.);
#754=B_SPLINE_CURVE_WITH_KNOTS('',3,(#88477,#88478,#88479,#88480),
 .UNSPECIFIED.,.F.,.F.,(4,4),(-0.0155031780625747,0.),.UNSPECIFIED.);
#755=B_SPLINE_CURVE_WITH_KNOTS('',3,(#88653,#88654,#88655,#88656,#88657,
#88658,#88659,#88660,#88661,#88662,#88663,#88664,#88665,#88666,#88667,#88668,
#88669,#88670,#88671,#88672,#88673,#88674,#88675,#88676,#88677,#88678,#88679,
#88680,#88681,#88682,#88683,#88684,#88685,#88686,#88687,#88688,#88689,#88690,
#88691,#88692,#88693,#88694,#88695,#88696,#88697,#88698,#88699,#88700,#88701,
#88702,#88703,#88704,#88705,#88706,#88707,#88708,#88709,#88710,#88711,#88712,
#88713,#88714,#88715,#88716,#88717,#88718,#88719,#88720,#88721,#88722,#88723,
#88724,#88725,#88726,#88727,#88728,#88729,#88730,#88731,#88732,#88733,#88734,
#88735,#88736,#88737,#88738,#88739,#88740,#88741,#88742,#88743),
 .UNSPECIFIED.,.F.,.F.,(4,3,3,3,3,3,3,3,3,3,3,3,3,3,3,3,3,3,3,3,3,3,3,3,
3,3,3,3,3,3,4),(0.,0.0254571918318206,0.0518171336468171,0.0781770754618136,
0.089917979704679,0.0966186220362691,0.102681367599265,0.129991607231578,
0.157832378191868,0.184687655883825,0.195924578330426,0.202922301283516,
0.206879022820041,0.236200447167097,0.265521871514153,0.293412006162953,
0.302822277125942,0.309408406301434,0.31463515273045,0.343053457095624,
0.372027352294228,0.401483492527513,0.421616062260858,0.426694015683236,
0.456850957722602,0.481878245307923,0.490063675457469,0.498374794492553,
0.528883347928461,0.557282026181522,0.566816364269905),.UNSPECIFIED.);
#756=B_SPLINE_CURVE_WITH_KNOTS('',3,(#88858,#88859,#88860,#88861,#88862,
#88863,#88864,#88865,#88866,#88867,#88868,#88869,#88870,#88871,#88872,#88873,
#88874,#88875,#88876,#88877,#88878,#88879,#88880,#88881,#88882,#88883,#88884,
#88885,#88886,#88887,#88888,#88889,#88890,#88891,#88892,#88893,#88894,#88895,
#88896,#88897,#88898,#88899,#88900,#88901,#88902,#88903,#88904,#88905,#88906,
#88907,#88908,#88909,#88910,#88911,#88912,#88913,#88914,#88915,#88916,#88917,
#88918,#88919,#88920,#88921,#88922,#88923,#88924,#88925,#88926,#88927,#88928,
#88929,#88930,#88931,#88932,#88933,#88934,#88935,#88936,#88937,#88938,#88939,
#88940,#88941,#88942,#88943,#88944,#88945,#88946,#88947,#88948,#88949,#88950,
#88951,#88952,#88953,#88954,#88955,#88956,#88957,#88958,#88959,#88960,#88961,
#88962,#88963,#88964,#88965,#88966,#88967,#88968,#88969,#88970,#88971,#88972,
#88973,#88974,#88975,#88976,#88977,#88978,#88979,#88980,#88981,#88982,#88983,
#88984,#88985,#88986,#88987,#88988,#88989,#88990,#88991,#88992,#88993,#88994,
#88995,#88996,#88997,#88998,#88999,#89000,#89001,#89002,#89003,#89004,#89005,
#89006,#89007,#89008,#89009,#89010,#89011,#89012,#89013,#89014,#89015,#89016,
#89017,#89018,#89019,#89020,#89021,#89022,#89023,#89024,#89025,#89026,#89027),
 .UNSPECIFIED.,.F.,.F.,(4,2,2,2,2,2,2,2,2,2,2,2,2,2,2,2,2,2,2,2,2,2,2,2,
2,2,2,2,2,2,2,2,2,2,2,2,2,2,2,2,2,2,2,2,2,2,2,2,2,2,2,2,2,2,2,2,2,2,2,2,
2,2,2,2,2,2,2,2,2,2,2,2,2,2,2,2,2,2,2,2,2,2,2,2,4),(-1.2515673108366,-1.22435849913044,
-1.18111626973005,-1.17544558238588,-1.17313343276111,-1.17155791431562,
-1.16991884844908,-1.16738471241629,-1.15964630200229,-1.0993075393073,
-1.06370295787804,-1.05814004411266,-1.05464036190055,-1.05188693155765,
-1.0488117399633,-1.04367588385316,-1.02350567064026,-0.970063196322433,
-0.940627890269205,-0.936844402153188,-0.934908337774157,-0.933366910608549,
-0.931531482081231,-0.928126216997923,-0.90836141146552,-0.83602400114745,
-0.823461389161282,-0.818945364448262,-0.816296041589489,-0.813522380477069,
-0.809899489959606,-0.80211442928955,-0.771129890465391,-0.72688847713087,
-0.719255203577689,-0.702631820792681,-0.699554102394289,-0.697612420993421,
-0.696079488323228,-0.694276095606343,-0.690953296379212,-0.672420985195493,
-0.614755594276794,-0.602710917804209,-0.586308628129192,-0.581345526424109,
-0.578323752560248,-0.575586243211812,-0.572062671692218,-0.564690986793914,
-0.536582468568329,-0.5053700714835,-0.468380511459306,-0.46263404600946,
-0.460316384288055,-0.458886752268476,-0.457282481549026,-0.454916849166946,
-0.448470523637336,-0.409582319930846,-0.354306700297234,-0.345780899997678,
-0.342301711255695,-0.339718401676499,-0.336893078941839,-0.332987395763267,
-0.323623129832107,-0.310488980261098,-0.232900434545352,-0.225381943817547,
-0.222820600626815,-0.221171766935522,-0.219579718940233,-0.217955660179146,
-0.213743814124771,-0.177840686383126,-0.119019789569982,-0.110969718024,
-0.107306702527921,-0.104485004599358,-0.101440861244329,-0.0965944039422034,
-0.0802244065616758,-0.0518476034352533,-0.00381635513711168),
 .UNSPECIFIED.);
#757=B_SPLINE_CURVE_WITH_KNOTS('',3,(#89030,#89031,#89032,#89033,#89034,
#89035,#89036,#89037,#89038,#89039,#89040,#89041,#89042,#89043,#89044,#89045,
#89046,#89047,#89048,#89049,#89050,#89051,#89052,#89053,#89054,#89055,#89056,
#89057,#89058,#89059,#89060,#89061,#89062,#89063,#89064,#89065,#89066,#89067,
#89068,#89069,#89070,#89071,#89072,#89073,#89074,#89075,#89076,#89077,#89078,
#89079,#89080,#89081,#89082,#89083,#89084,#89085,#89086,#89087,#89088,#89089,
#89090,#89091,#89092,#89093,#89094,#89095,#89096,#89097,#89098,#89099,#89100,
#89101,#89102,#89103,#89104,#89105,#89106,#89107,#89108,#89109,#89110,#89111,
#89112,#89113,#89114,#89115,#89116,#89117,#89118,#89119,#89120,#89121,#89122,
#89123,#89124,#89125,#89126,#89127,#89128,#89129,#89130,#89131,#89132,#89133,
#89134,#89135,#89136,#89137,#89138,#89139,#89140,#89141,#89142,#89143,#89144,
#89145,#89146,#89147,#89148,#89149,#89150,#89151,#89152,#89153),
 .UNSPECIFIED.,.F.,.F.,(4,3,3,3,3,3,3,3,3,3,3,3,3,3,3,3,3,3,3,3,3,3,3,3,
3,3,3,3,3,3,3,3,3,3,3,3,3,3,3,3,3,4),(11.6150328478184,11.7178927810683,
11.8206900629369,11.9234772178892,12.0262624995802,12.129071156527,12.2319284566529,
12.3349398758623,12.4380321171329,12.5413259654438,12.61338032228,12.7128604993709,
12.8121804206787,12.9121238426866,13.0112337068811,13.1103017019409,13.2093602993827,
13.3099521737224,13.4091491768461,13.5104384867939,13.6117277967416,13.7123825153464,
13.8128920177283,13.913284058111,14.0136117411332,14.1139061000047,14.2141981264595,
14.3145876671349,14.4150241421376,14.5156398886915,14.6100752712031,14.7107559040164,
14.8112948220338,14.9117214609962,15.0120868840636,15.1124220794924,15.2127579970338,
15.3131959775761,15.4136834531212,15.5143539969786,15.6084227456647,15.635150476959),
 .UNSPECIFIED.);
#758=B_SPLINE_CURVE_WITH_KNOTS('',3,(#89158,#89159,#89160,#89161,#89162,
#89163,#89164,#89165,#89166,#89167,#89168,#89169,#89170,#89171,#89172,#89173,
#89174,#89175,#89176,#89177,#89178,#89179,#89180,#89181,#89182,#89183,#89184,
#89185,#89186,#89187,#89188,#89189,#89190,#89191,#89192,#89193,#89194,#89195,
#89196,#89197,#89198,#89199,#89200,#89201,#89202,#89203,#89204,#89205,#89206,
#89207,#89208,#89209,#89210,#89211,#89212,#89213,#89214,#89215,#89216,#89217,
#89218,#89219,#89220,#89221,#89222,#89223,#89224,#89225,#89226,#89227,#89228,
#89229,#89230,#89231,#89232,#89233,#89234,#89235,#89236,#89237,#89238,#89239,
#89240,#89241,#89242,#89243,#89244,#89245,#89246,#89247,#89248,#89249,#89250,
#89251,#89252,#89253,#89254,#89255,#89256,#89257,#89258,#89259,#89260,#89261,
#89262,#89263,#89264,#89265,#89266,#89267,#89268,#89269,#89270,#89271,#89272,
#89273,#89274,#89275,#89276,#89277,#89278,#89279,#89280,#89281,#89282,#89283,
#89284,#89285,#89286,#89287,#89288,#89289,#89290,#89291,#89292,#89293,#89294,
#89295,#89296,#89297,#89298,#89299,#89300,#89301,#89302,#89303,#89304,#89305,
#89306,#89307,#89308,#89309,#89310,#89311,#89312,#89313,#89314,#89315,#89316,
#89317,#89318,#89319,#89320,#89321,#89322,#89323,#89324,#89325,#89326,#89327,
#89328,#89329,#89330,#89331,#89332,#89333,#89334,#89335,#89336,#89337,#89338,
#89339,#89340,#89341,#89342,#89343,#89344,#89345,#89346,#89347,#89348,#89349,
#89350,#89351,#89352,#89353,#89354,#89355,#89356,#89357,#89358,#89359,#89360,
#89361,#89362,#89363,#89364,#89365,#89366,#89367,#89368,#89369,#89370,#89371,
#89372,#89373,#89374,#89375,#89376,#89377,#89378,#89379,#89380,#89381,#89382,
#89383,#89384,#89385,#89386,#89387,#89388,#89389,#89390,#89391,#89392,#89393,
#89394,#89395,#89396,#89397,#89398,#89399,#89400,#89401,#89402,#89403,#89404,
#89405,#89406,#89407,#89408,#89409),.UNSPECIFIED.,.F.,.F.,(4,2,2,2,2,2,
2,2,2,2,2,2,2,2,2,2,2,2,2,2,2,2,2,2,2,2,2,2,2,2,2,2,2,2,2,2,2,2,2,2,2,2,
2,2,2,2,2,2,2,2,2,2,2,2,2,2,2,2,2,2,2,2,2,2,2,2,2,2,2,2,2,2,2,2,2,2,2,2,
2,2,2,2,2,2,2,2,2,2,2,2,2,2,2,2,2,2,2,2,2,2,2,2,2,2,2,2,2,2,2,2,2,2,2,2,
2,2,2,2,2,2,2,2,2,2,2,4),(-2.74596130104751,-2.72684582105165,-2.72242131286312,
-2.71937229190755,-2.71679617626614,-2.71404945553218,-2.71060476704055,
-2.70522045400994,-2.67511637823372,-2.64750863656549,-2.62210270826699,
-2.60295764488784,-2.59955536128111,-2.59772558506206,-2.59618889512473,
-2.59425996079627,-2.59050191505979,-2.56264900107927,-2.49649139540665,
-2.48897828315974,-2.48299772668024,-2.47975463171809,-2.479725069868,-2.47969492845286,
-2.47966419244804,-2.47963284637204,-2.47960087428214,-2.47956825975468,
-2.47954544089104,-2.4795204642658,-2.47949312009591,-2.47946317725337,
-2.47943038095463,-2.47939445019257,-2.47935507489099,-2.47931191274788,
-2.47926458574908,-2.47921267633288,-2.47915572252463,-2.47909321448,-2.47633865405684,
-2.47281699864536,-2.4671774715544,-2.42019285991096,-2.38617755577876,
-2.36543234783292,-2.36199867938643,-2.36016225741302,-2.35862590846863,
-2.35670484273269,-2.35369425858519,-2.33829393891924,-2.32902161585575,
-2.26453017465292,-2.24896957980145,-2.2442582480386,-2.2412774355981,-2.2385001973981,
-2.23487548393799,-2.22683531039053,-2.16507749804811,-2.12899344642868,
-2.12484631392815,-2.12286498111636,-2.12133864671178,-2.11955425845572,
-2.11644591677456,-2.10375665387797,-2.03159606023987,-2.0120582258132,
-2.00697622583128,-2.003914474815,-2.00116117124945,-1.9976452849142,-1.99202345799012,
-1.94394477625816,-1.90581032736851,-1.88986575871525,-1.88665372202272,
-1.88486518882826,-1.88332503771993,-1.88134241604678,-1.87812717286299,
-1.85863339131255,-1.80809854872818,-1.77872668034899,-1.77116201148413,
-1.76758630099531,-1.76482521486805,-1.76179418482937,-1.75685342154035,
-1.74084672824851,-1.6721503775032,-1.65260031526199,-1.64921360143595,
-1.6473869560256,-1.6458493141535,-1.64391472338356,-1.64013375207598,-1.6106872258172,
-1.56008317041423,-1.5374741737023,-1.53215832280398,-1.52904379965535,
-1.52629694106275,-1.5228613199515,-1.51750907180911,-1.48825471392759,
-1.43322821497606,-1.41500050277623,-1.4116717250324,-1.40985749183632,
-1.40832052744295,-1.40637394901052,-1.4032756794298,-1.3861955666591,-1.38221198054699,
-1.34860598513101,-1.30151785999778,-1.29588783635578,-1.29237067383878,
-1.28961880804336,-1.28656118902796,-1.28149206889162,-1.26208531559498,
-1.2515673108366),.UNSPECIFIED.);
#759=B_SPLINE_CURVE_WITH_KNOTS('',3,(#89411,#89412,#89413,#89414),
 .UNSPECIFIED.,.F.,.F.,(4,4),(15.635150476959,15.707963267949),
 .UNSPECIFIED.);
#760=B_SPLINE_CURVE_WITH_KNOTS('',3,(#89415,#89416,#89417,#89418,#89419,
#89420,#89421,#89422,#89423,#89424,#89425,#89426,#89427,#89428,#89429,#89430,
#89431,#89432,#89433,#89434,#89435,#89436,#89437,#89438,#89439,#89440,#89441,
#89442,#89443,#89444,#89445,#89446,#89447,#89448,#89449,#89450,#89451,#89452,
#89453,#89454,#89455,#89456,#89457,#89458,#89459,#89460,#89461,#89462,#89463,
#89464,#89465,#89466,#89467,#89468,#89469,#89470,#89471,#89472,#89473,#89474,
#89475,#89476,#89477,#89478,#89479,#89480,#89481,#89482,#89483,#89484,#89485,
#89486,#89487,#89488,#89489,#89490,#89491,#89492,#89493,#89494,#89495,#89496,
#89497,#89498,#89499,#89500,#89501,#89502,#89503,#89504,#89505,#89506,#89507,
#89508,#89509,#89510,#89511,#89512,#89513,#89514,#89515,#89516,#89517,#89518,
#89519,#89520,#89521,#89522,#89523,#89524,#89525,#89526,#89527,#89528,#89529,
#89530,#89531,#89532,#89533,#89534,#89535,#89536,#89537,#89538,#89539,#89540,
#89541,#89542,#89543,#89544,#89545,#89546,#89547,#89548,#89549,#89550,#89551,
#89552,#89553,#89554,#89555,#89556,#89557,#89558,#89559,#89560,#89561,#89562,
#89563,#89564,#89565,#89566,#89567,#89568,#89569,#89570,#89571,#89572,#89573,
#89574,#89575,#89576,#89577,#89578,#89579,#89580,#89581,#89582,#89583,#89584,
#89585,#89586,#89587,#89588,#89589,#89590,#89591,#89592,#89593,#89594,#89595,
#89596,#89597,#89598,#89599,#89600,#89601,#89602,#89603,#89604,#89605,#89606,
#89607,#89608,#89609,#89610,#89611,#89612,#89613,#89614,#89615,#89616,#89617,
#89618),.UNSPECIFIED.,.F.,.F.,(4,2,2,2,2,2,2,2,2,2,2,2,2,2,2,2,2,2,2,2,
2,2,2,2,2,2,2,2,2,2,2,2,2,2,2,2,2,2,2,2,2,2,2,2,2,2,2,2,2,2,2,2,2,2,2,2,
2,2,2,2,2,2,2,2,2,2,2,2,2,2,2,2,2,2,2,2,2,2,2,2,2,2,2,2,2,2,2,2,2,2,2,2,
2,2,2,2,2,2,2,2,2,4),(-2.98957413435225,-2.92293074458371,-2.91013837221342,
-2.90095504915141,-2.89707614956163,-2.89425265569043,-2.8916588311148,
-2.88814692245246,-2.87941471369762,-2.82976411010901,-2.79796495390714,
-2.78670708167694,-2.78189848099851,-2.77925522439628,-2.77701460649494,
-2.77542935524957,-2.77397499015983,-2.77162826755696,-2.76587200822799,
-2.7250895086881,-2.68624164526005,-2.66590661028265,-2.66070453546092,
-2.657583278642,-2.65478404542381,-2.65121928814907,-2.64553714632705,-2.59911345921582,
-2.5656538196434,-2.54449388765869,-2.54100065660931,-2.539131123257,-2.53756832620688,
-2.53561287325283,-2.53181148645191,-2.50392182591024,-2.44655015813056,
-2.43470205020368,-2.42603259226309,-2.42222399796675,-2.41939553826342,
-2.41675696755446,-2.41312142376263,-2.40377442571152,-2.32699092878548,
-2.30690690240132,-2.30346565953354,-2.30161228261404,-2.30005438234876,
-2.29809519710445,-2.29500235210593,-2.27856838278559,-2.21653120644009,
-2.19198790275312,-2.18650101799731,-2.18332441100193,-2.18054514951452,
-2.17709774462248,-2.1717810293574,-2.1444143946996,-2.08175518424723,-2.07307842973623,
-2.06720084214376,-2.06490329017409,-2.06329879931526,-2.06182057908956,
-2.05975637643455,-2.05435462513705,-2.00506292444482,-1.95671257219573,
-1.94993615653964,-1.9464843251575,-1.9437008729984,-1.94051874492825,-1.93515983628363,
-1.91478867859304,-1.85745606031538,-1.84038620661764,-1.83398912462634,
-1.82933062865304,-1.82723546660552,-1.82566279584796,-1.82389601835563,
-1.82085558314271,-1.80964880205187,-1.73662019724725,-1.71652005577685,
-1.71134541138908,-1.70823523339447,-1.70544263040521,-1.70188190643201,
-1.69619781331851,-1.6493656260355,-1.61543123898372,-1.59466481383716,
-1.59119672964362,-1.58933758323233,-1.5877793337795,-1.58582545399308,
-1.58202341996452,-1.55346356205055,-1.51266683266716),.UNSPECIFIED.);
#761=B_SPLINE_CURVE_WITH_KNOTS('',3,(#89624,#89625,#89626,#89627,#89628,
#89629,#89630,#89631,#89632,#89633,#89634,#89635,#89636,#89637,#89638,#89639,
#89640,#89641,#89642,#89643,#89644,#89645,#89646,#89647,#89648,#89649,#89650,
#89651,#89652,#89653,#89654,#89655,#89656,#89657,#89658,#89659,#89660,#89661,
#89662,#89663,#89664,#89665,#89666,#89667,#89668,#89669,#89670,#89671,#89672,
#89673,#89674,#89675,#89676,#89677,#89678,#89679,#89680,#89681,#89682,#89683,
#89684,#89685,#89686,#89687,#89688,#89689,#89690,#89691,#89692,#89693,#89694,
#89695,#89696,#89697,#89698,#89699,#89700,#89701,#89702,#89703,#89704,#89705,
#89706,#89707,#89708,#89709,#89710,#89711,#89712,#89713,#89714,#89715,#89716,
#89717,#89718,#89719,#89720,#89721,#89722,#89723,#89724,#89725,#89726,#89727,
#89728,#89729,#89730,#89731,#89732,#89733,#89734,#89735,#89736,#89737,#89738,
#89739,#89740,#89741,#89742,#89743,#89744,#89745,#89746,#89747,#89748,#89749,
#89750,#89751,#89752,#89753,#89754,#89755,#89756,#89757,#89758,#89759,#89760,
#89761,#89762,#89763,#89764,#89765,#89766,#89767,#89768,#89769,#89770,#89771,
#89772,#89773,#89774,#89775,#89776,#89777,#89778,#89779,#89780,#89781,#89782,
#89783,#89784,#89785,#89786,#89787,#89788,#89789,#89790,#89791,#89792,#89793,
#89794,#89795,#89796,#89797,#89798,#89799,#89800,#89801,#89802,#89803,#89804,
#89805,#89806,#89807,#89808,#89809,#89810,#89811,#89812,#89813,#89814,#89815,
#89816,#89817,#89818,#89819,#89820,#89821),.UNSPECIFIED.,.F.,.F.,(4,2,2,
2,2,2,2,2,2,2,2,2,2,2,2,2,2,2,2,2,2,2,2,2,2,2,2,2,2,2,2,2,2,2,2,2,2,2,2,
2,2,2,2,2,2,2,2,2,2,2,2,2,2,2,2,2,2,2,2,2,2,2,2,2,2,2,2,2,2,2,2,2,2,2,2,
2,2,2,2,2,2,2,2,2,2,2,2,2,2,2,2,2,2,2,2,2,2,2,4),(-1.47789197491073,-1.41686972830544,
-1.3890785606746,-1.38378577682514,-1.38036862332489,-1.37762379445051,
-1.37449782019632,-1.36912803422488,-1.34571223404409,-1.29089043456906,
-1.26629215690005,-1.26258628142778,-1.26066824487321,-1.25913165025539,
-1.25729173874776,-1.25384320608642,-1.23271761582457,-1.19916887222781,
-1.15212999409321,-1.14649506710233,-1.14297416629817,-1.14021891174287,
-1.13715701829772,-1.13207953181691,-1.11262116564429,-1.07473851007211,
-1.0317097224467,-1.02602801879475,-1.02371246889212,-1.02213506388296,
-1.02049538514544,-1.01796062384299,-1.01022251912543,-0.949804493250946,
-0.914359309644795,-0.908802674216476,-0.905305390382556,-0.902552869647405,
-0.899477686147479,-0.894339483334249,-0.874130340155093,-0.824871239310694,
-0.791242054640749,-0.787436667388664,-0.785497327356098,-0.783959692472395,
-0.782137437032186,-0.778771768757833,-0.759722066915378,-0.697055384001429,
-0.675501602837159,-0.670097521078887,-0.666932728682255,-0.664465854178,
-0.661221898959827,-0.655306160101179,-0.620637967545861,-0.58343565599599,
-0.553605864413414,-0.549820438836707,-0.547885438263039,-0.54634815550498,
-0.544522670398463,-0.54114151121831,-0.521723963848347,-0.454754481856921,
-0.437210952171618,-0.432105725369859,-0.429038065690201,-0.426284563046816,
-0.422775450884152,-0.415560139825568,-0.365728839964459,-0.318575502838319,
-0.313080744137428,-0.311022519459302,-0.309558813370945,-0.307980585177986,
-0.305742110323364,-0.30013164023708,-0.291947760209732,-0.235751835887413,
-0.201450426413078,-0.195927412534167,-0.192440436493334,-0.18968923253603,
-0.187116094721187,-0.182798655480253,-0.169480225012182,-0.148209782927271,
-0.123966271616637,-0.0812834788924502,-0.0755919121589384,-0.0732749204249909,
-0.0716973995340425,-0.0700584881459055,-0.0675263830913471,-0.0598077889728894,
-0.000705296177145865),.UNSPECIFIED.);
#762=B_SPLINE_CURVE_WITH_KNOTS('',3,(#89822,#89823,#89824,#89825),
 .UNSPECIFIED.,.F.,.F.,(4,4),(-2.76352601725825,-2.74596130104751),
 .UNSPECIFIED.);
#763=B_SPLINE_CURVE_WITH_KNOTS('',3,(#89826,#89827,#89828,#89829,#89830,
#89831,#89832,#89833,#89834,#89835,#89836,#89837,#89838,#89839,#89840,#89841,
#89842,#89843,#89844,#89845,#89846,#89847,#89848,#89849,#89850,#89851,#89852,
#89853,#89854,#89855,#89856,#89857,#89858,#89859,#89860,#89861,#89862,#89863,
#89864,#89865,#89866,#89867,#89868,#89869,#89870,#89871,#89872,#89873,#89874,
#89875,#89876,#89877,#89878,#89879,#89880,#89881,#89882,#89883,#89884,#89885,
#89886,#89887,#89888,#89889,#89890,#89891,#89892,#89893,#89894,#89895,#89896,
#89897,#89898,#89899,#89900,#89901,#89902,#89903,#89904,#89905,#89906,#89907,
#89908,#89909,#89910,#89911,#89912,#89913,#89914,#89915,#89916,#89917,#89918,
#89919,#89920,#89921,#89922,#89923,#89924,#89925,#89926,#89927,#89928,#89929,
#89930,#89931,#89932,#89933,#89934,#89935,#89936,#89937,#89938,#89939,#89940,
#89941,#89942,#89943,#89944,#89945,#89946,#89947,#89948,#89949,#89950,#89951,
#89952,#89953,#89954,#89955,#89956,#89957,#89958,#89959,#89960,#89961,#89962,
#89963,#89964,#89965,#89966,#89967,#89968,#89969,#89970,#89971,#89972,#89973,
#89974,#89975,#89976,#89977,#89978,#89979,#89980,#89981,#89982,#89983,#89984,
#89985,#89986,#89987,#89988,#89989,#89990,#89991,#89992,#89993,#89994,#89995,
#89996,#89997,#89998,#89999,#90000,#90001,#90002,#90003,#90004,#90005,#90006,
#90007,#90008,#90009,#90010,#90011,#90012,#90013,#90014,#90015,#90016,#90017,
#90018,#90019,#90020,#90021,#90022,#90023,#90024,#90025,#90026,#90027,#90028,
#90029,#90030,#90031,#90032,#90033,#90034,#90035,#90036,#90037,#90038,#90039,
#90040,#90041),.UNSPECIFIED.,.F.,.F.,(4,2,2,2,2,2,2,2,2,2,2,2,2,2,2,2,2,
2,2,2,2,2,2,2,2,2,2,2,2,2,2,2,2,2,2,2,2,2,2,2,2,2,2,2,2,2,2,2,2,2,2,2,2,
2,2,2,2,2,2,2,2,2,2,2,2,2,2,2,2,2,2,2,2,2,2,2,2,2,2,2,2,2,2,2,2,2,2,2,2,
2,2,2,2,2,2,2,2,2,2,2,2,2,2,2,2,2,2,4),(-1.51266683266716,-1.49541993273005,
-1.47887900394735,-1.47383826195344,-1.47075792578449,-1.46795935128176,
-1.46434509020257,-1.45673382755789,-1.42732277547221,-1.37690379305642,
-1.35751191070546,-1.35427161457043,-1.35226722718299,-1.35070554134252,
-1.34888488141247,-1.34559673011018,-1.32882556253793,-1.28405894756381,
-1.24384138925538,-1.23814886308824,-1.23458554046803,-1.2317925740647,
-1.228683715852,-1.22351533459441,-1.20349466661584,-1.12479924966047,-1.11802999873483,
-1.11552204707489,-1.11403689096902,-1.11243596725831,-1.11016404529081,
-1.10446111773446,-1.07477621055012,-1.02636085301469,-1.00492336632276,
-0.999485136427048,-0.99628533626524,-0.993504442951504,-0.990078946256255,
-0.983429261080415,-0.93891371504645,-0.890248308468409,-0.881226647652229,
-0.878419126883371,-0.876704042247504,-0.875114867005384,-0.872908733303356,
-0.867610372549159,-0.842068436779016,-0.812474093608546,-0.769012227987209,
-0.763282595597802,-0.759707673875687,-0.756912777297084,-0.753809131882331,
-0.748666699039238,-0.728974028496135,-0.655267307637103,-0.644151324860056,
-0.641119220353837,-0.639354072386046,-0.637781175775374,-0.635683096670152,
-0.631006628918759,-0.593452676122721,-0.534578265305192,-0.526205644581475,
-0.522490001770164,-0.519665745794587,-0.516655958811039,-0.511943113518986,
-0.496762656941134,-0.471309941288985,-0.432312051694832,-0.421904247692991,
-0.40720777399811,-0.403922486841818,-0.402081965744691,-0.400521370479417,
-0.398541633628378,-0.394488972601381,-0.354679141705833,-0.297311951236022,
-0.289653552701159,-0.285532505422394,-0.282935446670138,-0.280073975073642,
-0.2761582401841,-0.266759380907634,-0.253502913961651,-0.213650866315259,
-0.173598485104228,-0.167826212493436,-0.165476509135714,-0.163876444538086,
-0.162212569742731,-0.159637534021854,-0.151749844139344,-0.0973616687214255,
-0.0778315392007462,-0.05520166125016,-0.0496731901416544,-0.0464523816290895,
-0.0436725378849232,-0.0410081735768323,-0.0376833416531648,-0.0326321706283457,
-0.0182824356155657),.UNSPECIFIED.);
#764=B_SPLINE_CURVE_WITH_KNOTS('',3,(#90046,#90047,#90048,#90049,#90050,
#90051,#90052,#90053,#90054,#90055,#90056,#90057,#90058,#90059,#90060,#90061,
#90062,#90063,#90064,#90065,#90066,#90067,#90068,#90069,#90070,#90071,#90072,
#90073,#90074,#90075,#90076,#90077,#90078,#90079,#90080,#90081,#90082,#90083,
#90084,#90085,#90086,#90087,#90088,#90089,#90090,#90091,#90092,#90093,#90094,
#90095,#90096,#90097,#90098,#90099,#90100,#90101,#90102,#90103,#90104,#90105,
#90106,#90107,#90108,#90109,#90110,#90111,#90112,#90113,#90114,#90115,#90116,
#90117,#90118,#90119,#90120,#90121,#90122,#90123,#90124,#90125,#90126,#90127,
#90128,#90129,#90130,#90131,#90132,#90133,#90134,#90135,#90136,#90137,#90138,
#90139,#90140,#90141,#90142,#90143,#90144,#90145,#90146,#90147,#90148,#90149,
#90150,#90151,#90152,#90153,#90154,#90155,#90156,#90157,#90158,#90159,#90160,
#90161,#90162,#90163,#90164,#90165,#90166,#90167,#90168,#90169,#90170,#90171,
#90172,#90173,#90174,#90175,#90176,#90177,#90178,#90179,#90180,#90181,#90182,
#90183,#90184,#90185,#90186,#90187,#90188,#90189,#90190,#90191,#90192,#90193,
#90194,#90195,#90196,#90197,#90198,#90199,#90200,#90201,#90202,#90203,#90204,
#90205,#90206,#90207,#90208,#90209,#90210,#90211,#90212,#90213,#90214,#90215,
#90216,#90217,#90218,#90219,#90220,#90221,#90222,#90223,#90224,#90225,#90226,
#90227,#90228,#90229,#90230,#90231,#90232,#90233,#90234,#90235,#90236,#90237,
#90238,#90239,#90240,#90241,#90242,#90243,#90244,#90245,#90246,#90247,#90248,
#90249,#90250,#90251,#90252,#90253,#90254,#90255,#90256,#90257,#90258,#90259,
#90260,#90261,#90262,#90263,#90264,#90265,#90266,#90267,#90268,#90269),
 .UNSPECIFIED.,.F.,.F.,(4,2,2,2,2,2,2,2,2,2,2,2,2,2,2,2,2,2,2,2,2,2,2,2,
2,2,2,2,2,2,2,2,2,2,2,2,2,2,2,2,2,2,2,2,2,2,2,2,2,2,2,2,2,2,2,2,2,2,2,2,
2,2,2,2,2,2,2,2,2,2,2,2,2,2,2,2,2,2,2,2,2,2,2,2,2,2,2,2,2,2,2,2,2,2,2,2,
2,2,2,2,2,2,2,2,2,2,2,2,2,2,2,4),(-2.97226061936036,-2.93571120009826,-2.9300133755847,
-2.92704069725888,-2.92450288252192,-2.92286304481359,-2.92128703398166,
-2.9189759449437,-2.91331717463684,-2.86978906514473,-2.84307833706508,
-2.81552463117315,-2.80917975508044,-2.80643072780928,-2.80363842954954,
-2.8010458400292,-2.79680191654852,-2.78599163095739,-2.73184172967793,
-2.69535892119586,-2.68918232910714,-2.68681249178123,-2.68520862080502,
-2.68377241594414,-2.68144652420498,-2.67569947722107,-2.63623164624101,
-2.59629359284983,-2.58269653659399,-2.57308582484009,-2.56915218791923,
-2.5663329067649,-2.5637730027392,-2.55970911135672,-2.55215496060649,-2.49369645592223,
-2.48635524258116,-2.45701243143504,-2.45137229878483,-2.44912944327533,
-2.44755067793458,-2.44608849875275,-2.44403521648086,-2.43857489856752,
-2.39058551447352,-2.34002729766112,-2.33379274488407,-2.33048206261321,
-2.32801070830146,-2.32490170506544,-2.31960651102622,-2.30023583327052,
-2.23526414462728,-2.22232643234466,-2.21446577695024,-2.2119165922906,
-2.21027406109759,-2.20869943688505,-2.20639651476276,-2.20078833151477,
-2.15574923301884,-2.11933978898649,-2.10677830203486,-2.0977326277979,
-2.09389184345349,-2.09108912431445,-2.08850963880315,-2.08501004938938,
-2.07630400456507,-2.02814016906202,-1.99294461293695,-1.98302729027546,
-1.97654929981374,-1.97418076725253,-1.97257700401845,-1.97114030670519,
-1.9688125247289,-1.96305534839698,-1.92606296108136,-1.89479507525905,
-1.86679742631814,-1.85941746979412,-1.85587660337223,-1.8531194768352,
-1.85006953463277,-1.84504447942937,-1.82826905093786,-1.76040994782724,
-1.74091882792873,-1.73753445580317,-1.7357082804195,-1.73417103188239,
-1.73223686204881,-1.72845536740707,-1.69892547868359,-1.66601412138072,
-1.63993181671569,-1.62453786004526,-1.6198433588336,-1.61686567692248,
-1.61408614175634,-1.61045093561083,-1.60235576604179,-1.5410249302819,
-1.50523850797559,-1.50064234217139,-1.49857626128058,-1.49702595603265,
-1.49528610268978,-1.49229901967879,-1.47984598605197,-1.47789197491073),
 .UNSPECIFIED.);
#765=B_SPLINE_CURVE_WITH_KNOTS('',3,(#90271,#90272,#90273,#90274),
 .UNSPECIFIED.,.F.,.F.,(4,4),(-0.0182824356155657,-0.000703321212415426),
 .UNSPECIFIED.);
#766=B_SPLINE_CURVE_WITH_KNOTS('',3,(#90275,#90276,#90277,#90278,#90279,
#90280,#90281,#90282,#90283,#90284),.UNSPECIFIED.,.F.,.F.,(4,1,1,1,1,1,
1,4),(28.2743402550742,28.5869399136653,29.5852873881269,30.5836348625885,
31.5819823370501,32.5803298115117,33.5786772859733,34.4839353288417),
 .UNSPECIFIED.);
#767=B_SPLINE_CURVE_WITH_KNOTS('',3,(#90290,#90291,#90292,#90293,#90294,
#90295,#90296,#90297,#90298,#90299),.UNSPECIFIED.,.F.,.F.,(4,1,1,1,1,1,
1,4),(34.5575191894877,35.2752317647851,36.2740374763549,37.2728431879247,
38.2716488994945,39.2704546110642,40.269260322634,40.7676704970196),
 .UNSPECIFIED.);
#768=B_SPLINE_CURVE_WITH_KNOTS('',3,(#90300,#90301,#90302,#90303),
 .UNSPECIFIED.,.F.,.F.,(4,4),(-2.98942133639523,-2.97226061936036),
 .UNSPECIFIED.);
#769=B_SPLINE_CURVE_WITH_KNOTS('',3,(#90305,#90306,#90307,#90308),
 .UNSPECIFIED.,.F.,.F.,(4,4),(34.4839353288417,34.5575163999847),
 .UNSPECIFIED.);
#770=B_SPLINE_CURVE_WITH_KNOTS('',3,(#90309,#90310,#90311,#90312,#90313,
#90314,#90315,#90316,#90317,#90318,#90319,#90320,#90321,#90322,#90323,#90324,
#90325,#90326,#90327,#90328,#90329,#90330,#90331,#90332,#90333,#90334,#90335,
#90336,#90337,#90338,#90339,#90340,#90341,#90342,#90343,#90344,#90345,#90346,
#90347,#90348,#90349,#90350,#90351,#90352,#90353,#90354,#90355,#90356,#90357,
#90358,#90359,#90360,#90361,#90362,#90363,#90364,#90365,#90366,#90367,#90368,
#90369,#90370,#90371,#90372,#90373,#90374,#90375,#90376,#90377,#90378,#90379,
#90380,#90381,#90382,#90383,#90384,#90385,#90386,#90387,#90388,#90389,#90390,
#90391,#90392,#90393,#90394,#90395,#90396,#90397,#90398,#90399,#90400,#90401,
#90402,#90403,#90404,#90405,#90406,#90407,#90408,#90409,#90410,#90411,#90412,
#90413,#90414,#90415,#90416,#90417,#90418,#90419,#90420,#90421,#90422,#90423,
#90424,#90425,#90426,#90427,#90428,#90429,#90430,#90431,#90432,#90433,#90434,
#90435,#90436,#90437,#90438,#90439,#90440,#90441,#90442,#90443,#90444,#90445,
#90446,#90447,#90448,#90449,#90450,#90451,#90452,#90453,#90454,#90455,#90456,
#90457,#90458,#90459,#90460,#90461,#90462,#90463,#90464,#90465,#90466,#90467,
#90468,#90469,#90470,#90471,#90472,#90473,#90474,#90475,#90476,#90477,#90478,
#90479,#90480,#90481,#90482,#90483,#90484,#90485,#90486,#90487,#90488,#90489,
#90490,#90491,#90492,#90493,#90494,#90495,#90496,#90497,#90498,#90499,#90500,
#90501,#90502,#90503,#90504,#90505,#90506,#90507,#90508,#90509,#90510,#90511,
#90512,#90513,#90514,#90515,#90516,#90517,#90518,#90519,#90520,#90521,#90522,
#90523,#90524),.UNSPECIFIED.,.F.,.F.,(4,2,2,2,2,2,2,2,2,2,2,2,2,2,2,2,2,
2,2,2,2,2,2,2,2,2,2,2,2,2,2,2,2,2,2,2,2,2,2,2,2,2,2,2,2,2,2,2,2,2,2,2,2,
2,2,2,2,2,2,2,2,2,2,2,2,2,2,2,2,2,2,2,2,2,2,2,2,2,2,2,2,2,2,2,2,2,2,2,2,
2,2,2,2,2,2,2,2,2,2,2,2,2,2,2,2,2,2,4),(-2.98932851488204,-2.98778835877455,
-2.98589440660087,-2.98439686001854,-2.98288940256014,-2.98026659780242,
-2.97269261178509,-2.92782104182352,-2.89563002419035,-2.87525617600293,
-2.87005949080672,-2.86694440682519,-2.86415265864336,-2.86060023505363,
-2.85494392054553,-2.80673551748508,-2.78518678448732,-2.75509075281792,
-2.75192043656174,-2.74992348108331,-2.74808722290459,-2.74655885834968,
-2.74463977046219,-2.74107596409357,-2.72071738393961,-2.67605240524974,
-2.64274404418098,-2.63463169078566,-2.63092348463791,-2.62811141703,-2.62507404972935,
-2.62023106865622,-2.60541488658953,-2.54284167972397,-2.52472911455355,
-2.51807754648573,-2.51327703918794,-2.51115710299689,-2.50958168586097,
-2.50782882661511,-2.50485046276057,-2.49426806185102,-2.42004704528794,
-2.40032273478815,-2.39517884838337,-2.3920754931402,-2.38928159844871,
-2.38570898279933,-2.37998507469446,-2.3366737105664,-2.30726025807467,
-2.2814023789362,-2.27607276993591,-2.273861822143,-2.27227219030427,-2.27055975911447,
-2.26776271370155,-2.25882483558985,-2.21013823319637,-2.16562853116848,
-2.15898081424815,-2.15555632788938,-2.15277624815042,-2.14957737625101,
-2.14414070234367,-2.12271077631613,-2.06600733106761,-2.04352541983092,
-2.03855563409326,-2.03640597754623,-2.03482632255464,-2.03308800308641,
-2.03017453908286,-2.02020927187821,-1.94569132525569,-1.92559604926915,
-1.92042237079454,-1.9173127347055,-1.91452059446957,-1.91096042740721,
-1.90527714587453,-1.8584728900673,-1.82457079751584,-1.80378100627075,
-1.80031222002498,-1.79845298352699,-1.79689477356601,-1.79494107725788,
-1.79113990096616,-1.76383992326005,-1.75466129094146,-1.7103790584558,
-1.68855634712395,-1.68325002215229,-1.68011120206541,-1.67732415884313,
-1.67381276485327,-1.66829122751587,-1.63556664395172,-1.58908035005274,
-1.56659251959106,-1.56306275472084,-1.56119056593201,-1.55963291817536,
-1.55769418818297,-1.55467093822223,-1.53951992506579,-1.5128189813854),
 .UNSPECIFIED.);
#771=B_SPLINE_CURVE_WITH_KNOTS('',3,(#90530,#90531,#90532,#90533,#90534,
#90535,#90536,#90537,#90538,#90539,#90540,#90541,#90542,#90543,#90544,#90545,
#90546,#90547,#90548,#90549,#90550,#90551,#90552,#90553,#90554,#90555,#90556,
#90557,#90558,#90559,#90560,#90561,#90562,#90563,#90564,#90565,#90566,#90567,
#90568,#90569,#90570,#90571,#90572,#90573,#90574,#90575,#90576,#90577,#90578,
#90579,#90580,#90581,#90582,#90583,#90584,#90585,#90586,#90587,#90588,#90589,
#90590,#90591,#90592,#90593,#90594,#90595,#90596,#90597,#90598,#90599,#90600,
#90601,#90602,#90603,#90604,#90605,#90606,#90607,#90608,#90609,#90610,#90611,
#90612,#90613,#90614,#90615,#90616,#90617,#90618,#90619,#90620,#90621,#90622,
#90623,#90624,#90625,#90626,#90627,#90628,#90629,#90630,#90631,#90632,#90633,
#90634,#90635,#90636,#90637,#90638,#90639,#90640,#90641,#90642,#90643,#90644,
#90645,#90646,#90647,#90648,#90649,#90650,#90651,#90652,#90653,#90654,#90655,
#90656,#90657,#90658,#90659,#90660,#90661,#90662,#90663,#90664,#90665,#90666,
#90667,#90668,#90669,#90670,#90671,#90672,#90673,#90674,#90675,#90676,#90677,
#90678,#90679,#90680,#90681,#90682,#90683,#90684,#90685,#90686,#90687,#90688,
#90689,#90690,#90691,#90692,#90693,#90694,#90695,#90696,#90697,#90698,#90699,
#90700,#90701,#90702,#90703,#90704,#90705,#90706,#90707,#90708,#90709,#90710,
#90711,#90712,#90713,#90714,#90715,#90716),.UNSPECIFIED.,.F.,.F.,(4,3,3,
3,3,3,3,3,3,3,3,3,3,3,3,3,3,3,3,3,3,3,3,3,3,3,3,3,3,3,3,3,3,3,3,3,3,3,3,
3,3,3,3,3,3,3,3,3,3,3,3,3,3,3,3,3,3,3,3,3,3,3,4),(40.8407044966673,40.949576446156,
41.0587417112112,41.16837803931,41.2680660342038,41.3685653530978,41.4689192022502,
41.5691560072746,41.6693287783783,41.7694687756258,41.8696072180232,41.9698456501707,
42.0701320477337,42.1706016493045,42.2668717457736,42.3673710646681,42.467724913821,
42.5679617188459,42.6681344899501,42.768274487198,42.8684129295959,42.9686513617439,
43.0689377593074,43.1694073608787,43.2656774573433,43.3661767762382,43.4665306253915,
43.5667674304169,43.6669402015215,43.7670801987699,43.8672186411682,43.9674570733167,
44.0677434708806,44.1682130724524,44.2644831689131,44.3649824878077,44.4653363369606,
44.5655731419856,44.6657459130898,44.7658859103379,44.8660243527359,44.9662627848839,
45.0665491824475,45.1670187840189,45.2632888804829,45.3637881993776,45.4641420485306,
45.5643788535557,45.66455162466,45.7646916219081,45.8648300643062,45.9650684964543,
46.065354894018,46.1658244955894,46.2620945920527,46.3611093540537,46.4599956905364,
46.5587866981655,46.657515345266,46.7562542414466,46.8549915856982,46.9538361689612,
47.049949307842),.UNSPECIFIED.);
#772=B_SPLINE_CURVE_WITH_KNOTS('',3,(#90717,#90718,#90719,#90720),
 .UNSPECIFIED.,.F.,.F.,(4,4),(40.7676704970196,40.8407044966673),
 .UNSPECIFIED.);
#773=B_SPLINE_CURVE_WITH_KNOTS('',3,(#90721,#90722,#90723,#90724,#90725,
#90726,#90727,#90728,#90729,#90730,#90731,#90732,#90733,#90734,#90735,#90736,
#90737,#90738,#90739,#90740,#90741,#90742,#90743,#90744,#90745,#90746,#90747,
#90748,#90749,#90750,#90751,#90752,#90753,#90754,#90755,#90756,#90757,#90758,
#90759,#90760,#90761,#90762,#90763,#90764,#90765,#90766,#90767,#90768,#90769,
#90770,#90771,#90772,#90773,#90774,#90775,#90776,#90777,#90778,#90779,#90780,
#90781,#90782,#90783,#90784,#90785,#90786,#90787,#90788,#90789,#90790,#90791,
#90792,#90793,#90794,#90795,#90796,#90797,#90798,#90799,#90800,#90801,#90802,
#90803,#90804,#90805,#90806,#90807,#90808,#90809,#90810,#90811,#90812,#90813,
#90814,#90815,#90816,#90817,#90818,#90819,#90820,#90821,#90822,#90823,#90824,
#90825,#90826,#90827,#90828,#90829,#90830,#90831,#90832,#90833,#90834,#90835,
#90836,#90837,#90838,#90839,#90840,#90841,#90842,#90843,#90844,#90845,#90846,
#90847,#90848,#90849,#90850,#90851,#90852,#90853,#90854,#90855,#90856,#90857,
#90858,#90859,#90860,#90861,#90862,#90863,#90864,#90865,#90866,#90867,#90868,
#90869,#90870,#90871,#90872,#90873,#90874,#90875,#90876,#90877,#90878,#90879,
#90880,#90881,#90882,#90883,#90884,#90885,#90886,#90887,#90888,#90889,#90890,
#90891,#90892,#90893,#90894,#90895,#90896,#90897,#90898,#90899,#90900,#90901,
#90902,#90903,#90904,#90905,#90906,#90907,#90908,#90909,#90910,#90911,#90912,
#90913,#90914,#90915,#90916,#90917,#90918,#90919,#90920,#90921,#90922,#90923,
#90924,#90925,#90926,#90927,#90928),.UNSPECIFIED.,.F.,.F.,(4,2,2,2,2,2,
2,2,2,2,2,2,2,2,2,2,2,2,2,2,2,2,2,2,2,2,2,2,2,2,2,2,2,2,2,2,2,2,2,2,2,2,
2,2,2,2,2,2,2,2,2,2,2,2,2,2,2,2,2,2,2,2,2,2,2,2,2,2,2,2,2,2,2,2,2,2,2,2,
2,2,2,2,2,2,2,2,2,2,2,2,2,2,2,2,2,2,2,2,2,2,2,2,2,4),(-1.5128189813854,
-1.49567083096832,-1.45307413227607,-1.44736432644523,-1.44379610752678,
-1.44100295746722,-1.43789765896982,-1.4327440554255,-1.41289821672349,
-1.33701941613466,-1.32788697449916,-1.32506672451318,-1.32334898447117,
-1.32176130779641,-1.31956287674903,-1.31430923522431,-1.28919559950112,
-1.24582570152713,-1.21514795299362,-1.20969473844147,-1.20620360258639,
-1.20341783775063,-1.20026467307552,-1.1948952554176,-1.17220056504091,
-1.1214208005053,-1.09233947219059,-1.08852903105112,-1.08657300928951,
-1.08501424812754,-1.08315589273124,-1.07969285460531,-1.05906965598642,
-1.02506056964473,-0.978207308870275,-0.972523453866462,-0.968962528771095,
-0.966169568558434,-0.963058785891341,-0.957882655229978,-0.937771449854287,
-0.864372594763722,-0.853422151304499,-0.850406491738569,-0.848645133083884,
-0.847071573671554,-0.84496709524445,-0.840254188388205,-0.796780174036855,
-0.744562915832417,-0.735925584321552,-0.732409061490226,-0.729800621453063,
-0.726950120965683,-0.723013448462171,-0.713590663040318,-0.700386264481193,
-0.622310256163776,-0.620474876710382,-0.614551381160995,-0.612176246324312,
-0.610716105446037,-0.609090785945978,-0.606696709856131,-0.600184952828215,
-0.560759598242131,-0.506859750039304,-0.498295110963134,-0.494790644250799,
-0.492184786597833,-0.489330885443234,-0.485378038386267,-0.475860154232796,
-0.462481936633166,-0.423841273510261,-0.382746826914453,-0.376997583257265,
-0.37465152618693,-0.373052024613091,-0.371386839631552,-0.368806489078964,
-0.360876691787964,-0.347834542404448,-0.281506227765355,-0.263572463419871,
-0.258382386911189,-0.255267911273333,-0.252530368026711,-0.249119868729723,
-0.245370897789706,-0.239294959532918,-0.227122340723278,-0.170103188138698,
-0.142247401274889,-0.138453019450219,-0.136500016020774,-0.134940853933661,
-0.133078683496536,-0.129599649296975,-0.1085837118209,-0.0399478565732092,
-0.025297919610965,-0.0204812965032507,-0.0181663831353254),
 .UNSPECIFIED.);
#774=B_SPLINE_CURVE_WITH_KNOTS('',3,(#90934,#90935,#90936,#90937,#90938,
#90939,#90940,#90941,#90942,#90943,#90944,#90945,#90946,#90947,#90948,#90949,
#90950,#90951,#90952,#90953,#90954,#90955,#90956,#90957,#90958,#90959,#90960,
#90961,#90962,#90963,#90964,#90965,#90966,#90967,#90968,#90969,#90970,#90971,
#90972,#90973,#90974,#90975,#90976,#90977,#90978,#90979,#90980,#90981,#90982,
#90983,#90984,#90985,#90986,#90987,#90988,#90989,#90990,#90991,#90992,#90993,
#90994,#90995,#90996,#90997,#90998,#90999,#91000,#91001,#91002,#91003,#91004,
#91005,#91006,#91007,#91008,#91009,#91010,#91011,#91012,#91013,#91014,#91015,
#91016,#91017,#91018,#91019,#91020,#91021,#91022,#91023,#91024,#91025,#91026,
#91027,#91028,#91029,#91030,#91031,#91032,#91033,#91034,#91035,#91036,#91037,
#91038,#91039,#91040,#91041,#91042,#91043,#91044,#91045,#91046,#91047,#91048,
#91049,#91050,#91051,#91052,#91053,#91054,#91055,#91056,#91057,#91058,#91059,
#91060,#91061,#91062,#91063,#91064,#91065,#91066,#91067,#91068,#91069,#91070,
#91071,#91072,#91073,#91074,#91075,#91076,#91077,#91078,#91079,#91080,#91081,
#91082,#91083,#91084,#91085,#91086,#91087,#91088,#91089,#91090,#91091,#91092,
#91093,#91094,#91095,#91096,#91097,#91098,#91099,#91100,#91101,#91102,#91103,
#91104,#91105,#91106,#91107,#91108,#91109,#91110,#91111,#91112,#91113,#91114,
#91115,#91116,#91117,#91118,#91119,#91120,#91121,#91122,#91123,#91124,#91125,
#91126,#91127,#91128,#91129,#91130,#91131,#91132,#91133,#91134,#91135,#91136,
#91137,#91138,#91139,#91140,#91141,#91142,#91143,#91144,#91145,#91146,#91147,
#91148,#91149,#91150,#91151,#91152,#91153,#91154,#91155,#91156,#91157,#91158,
#91159,#91160,#91161,#91162,#91163,#91164,#91165,#91166,#91167,#91168,#91169,
#91170,#91171,#91172,#91173,#91174,#91175,#91176,#91177,#91178,#91179,#91180,
#91181,#91182,#91183,#91184,#91185,#91186,#91187,#91188,#91189,#91190,#91191,
#91192,#91193,#91194,#91195,#91196,#91197,#91198,#91199,#91200,#91201,#91202,
#91203,#91204,#91205,#91206,#91207,#91208,#91209),.UNSPECIFIED.,.F.,.F.,
(4,2,2,2,2,2,2,2,2,2,2,2,2,2,2,2,2,2,2,2,2,2,2,2,2,2,2,2,2,2,2,2,2,2,2,
2,2,2,2,2,2,2,2,2,2,2,2,2,2,2,2,2,2,2,2,2,2,2,2,2,2,2,2,2,2,2,2,2,2,2,2,
2,2,2,2,2,2,2,2,2,2,2,2,2,2,2,2,2,2,2,2,2,2,2,2,2,2,2,2,2,2,2,2,2,2,2,2,
2,2,2,2,2,2,2,2,2,2,2,2,2,2,2,2,2,2,2,2,2,2,2,2,2,2,2,2,2,2,4),(-1.47769960275031,
-1.46520500159341,-1.46142137727949,-1.45948680831023,-1.45794960835698,
-1.45612391342727,-1.45274156019952,-1.4332930110912,-1.36591535240939,
-1.34874335194779,-1.34367663044156,-1.34061753337441,-1.33786243728151,
-1.33433847772105,-1.32704615043421,-1.31752105852131,-1.2940883761119,
-1.25441289907634,-1.24754491635115,-1.24111876512238,-1.2267007419593,
-1.22346408585819,-1.22165017544255,-1.22011224317267,-1.21816318023877,
-1.21418115139273,-1.17604671336282,-1.11648193926087,-1.10820249131097,
-1.10453502196883,-1.10175070383545,-1.09878704986067,-1.09415477188927,
-1.07932624361566,-1.05463844854815,-1.00914539150954,-0.989641672915569,
-0.986425397616695,-0.984442242198698,-0.982901697782013,-0.981112668817764,
-0.977899804998459,-0.961950601712537,-0.923800013111866,-0.875784311267044,
-0.870160873977159,-0.866643949024871,-0.863889828178817,-0.860827159537057,
-0.855743609812093,-0.836199808712195,-0.764026914480133,-0.751301368299504,
-0.748189306226988,-0.746403686550737,-0.744877047662869,-0.74289620513113,
-0.738752740054192,-0.70282407275373,-0.64089710965624,-0.633676407434816,
-0.630098858432703,-0.62749942820228,-0.624710463881338,-0.620951288372684,
-0.612381976041064,-0.600670317028426,-0.543274804524316,-0.514798191759316,
-0.511029197321451,-0.509097732002018,-0.507560670049986,-0.505732384282472,
-0.502337987520761,-0.482599900480575,-0.411100059020389,-0.397509597104142,
-0.39286025354986,-0.38989278275308,-0.38710986771861,-0.383387097114636,
-0.375023329403023,-0.339257224828324,-0.301153845763967,-0.291800206477809,
-0.276398616065952,-0.273387877947604,-0.271466793144273,-0.26993041987305,
-0.269924612150525,-0.269918890519476,-0.269913253570044,-0.269907699920863,
-0.269902228210771,-0.269896837100948,-0.269891525257584,-0.269886291415292,
-0.269881134297622,-0.269876052649428,-0.269870930532896,-0.269865824595588,
-0.269860734729688,-0.269855660845424,-0.269850602840557,-0.269845560625204,
-0.269840534111527,-0.269835523201754,-0.26983052780726,-0.269825547838814,
-0.2698205832146,-0.269815633823564,-0.269810699572557,-0.269805780380058,
-0.269800876165509,-0.269795986828172,-0.267935510432697,-0.264359503994271,
-0.25972102959401,-0.24900911340479,-0.208157785964817,-0.200942191983474,
-0.162927737791891,-0.157310175041958,-0.153794902006492,-0.151040825263961,
-0.14797691847449,-0.142888287428457,-0.123285334514095,-0.0751874841014997,
-0.0593794010607326,-0.0393101460320602,-0.0360714697423875,-0.0340815723064463,
-0.0325403404573989,-0.0310885058504802,-0.0293215905673413,-0.0266877338920759,
-0.000704083095801744),.UNSPECIFIED.);
#775=B_SPLINE_CURVE_WITH_KNOTS('',3,(#91210,#91211,#91212,#91213),
 .UNSPECIFIED.,.F.,.F.,(4,4),(47.049949307842,47.1238898036008),
 .UNSPECIFIED.);
#776=B_SPLINE_CURVE_WITH_KNOTS('',3,(#91215,#91216,#91217,#91218,#91219,
#91220,#91221,#91222,#91223,#91224,#91225,#91226),.UNSPECIFIED.,.F.,.F.,
(4,2,2,2,2,4),(-0.0181663831353254,-0.017448962707184,-0.0147685891677303,
-0.0120368289253415,-0.00702288019292292,-0.000702852059331679),
 .UNSPECIFIED.);
#777=B_SPLINE_CURVE_WITH_KNOTS('',3,(#91227,#91228,#91229,#91230,#91231,
#91232,#91233,#91234,#91235,#91236,#91237,#91238,#91239,#91240,#91241,#91242,
#91243,#91244,#91245,#91246,#91247,#91248,#91249,#91250,#91251,#91252,#91253,
#91254,#91255,#91256,#91257,#91258,#91259,#91260,#91261,#91262,#91263,#91264,
#91265,#91266,#91267,#91268,#91269,#91270,#91271,#91272,#91273,#91274,#91275,
#91276,#91277,#91278,#91279,#91280,#91281,#91282,#91283,#91284,#91285,#91286,
#91287,#91288,#91289,#91290,#91291,#91292,#91293,#91294,#91295,#91296,#91297,
#91298,#91299,#91300,#91301,#91302,#91303,#91304,#91305,#91306,#91307,#91308,
#91309,#91310,#91311,#91312,#91313,#91314,#91315,#91316,#91317,#91318,#91319,
#91320,#91321,#91322,#91323,#91324,#91325,#91326,#91327,#91328,#91329,#91330,
#91331,#91332,#91333,#91334,#91335,#91336,#91337,#91338,#91339,#91340,#91341,
#91342,#91343,#91344,#91345,#91346,#91347,#91348,#91349,#91350,#91351,#91352,
#91353,#91354,#91355,#91356,#91357,#91358,#91359,#91360,#91361,#91362,#91363,
#91364,#91365,#91366,#91367,#91368,#91369,#91370,#91371,#91372,#91373,#91374,
#91375,#91376,#91377,#91378,#91379,#91380,#91381,#91382,#91383,#91384,#91385,
#91386,#91387,#91388,#91389,#91390,#91391,#91392,#91393,#91394,#91395,#91396,
#91397,#91398,#91399,#91400,#91401,#91402,#91403,#91404,#91405,#91406,#91407,
#91408,#91409,#91410,#91411,#91412,#91413,#91414,#91415,#91416,#91417,#91418,
#91419,#91420,#91421,#91422,#91423,#91424,#91425,#91426,#91427,#91428,#91429,
#91430,#91431,#91432,#91433,#91434,#91435,#91436,#91437,#91438,#91439,#91440,
#91441,#91442,#91443,#91444,#91445,#91446,#91447,#91448,#91449,#91450,#91451,
#91452,#91453,#91454,#91455,#91456,#91457,#91458),.UNSPECIFIED.,.F.,.F.,
(4,2,2,2,2,2,2,2,2,2,2,2,2,2,2,2,2,2,2,2,2,2,2,2,2,2,2,2,2,2,2,2,2,2,2,
2,2,2,2,2,2,2,2,2,2,2,2,2,2,2,2,2,2,2,2,2,2,2,2,2,2,2,2,2,2,2,2,2,2,2,2,
2,2,2,2,2,2,2,2,2,2,2,2,2,2,2,2,2,2,2,2,2,2,2,2,2,2,2,2,2,2,2,2,2,2,2,2,
2,2,2,2,2,2,2,2,4),(-2.98920213316816,-2.91355244760858,-2.89256055197457,
-2.88908328851811,-2.88722191595717,-2.88566332840344,-2.88371093550557,
-2.87991742760162,-2.85201164884243,-2.79494528879838,-2.78287689151404,
-2.7768380820173,-2.77310477523359,-2.76969853623019,-2.7696512060653,-2.76960253933043,
-2.76955243875846,-2.7695007984547,-2.76944750285888,-2.76939242557052,
-2.76933542797915,-2.76927635769579,-2.76921504673341,-2.769151309392,-2.76911156297201,
-2.76906336463706,-2.76900459466037,-2.76893244416893,-2.76884310754945,
-2.76837809301476,-2.76563282238037,-2.76197012537908,-2.75388912669262,
-2.69233794823319,-2.65626527350994,-2.65208028375244,-2.6500749403872,
-2.6485127827839,-2.64669195604716,-2.64349185354238,-2.62996962525229,
-2.61661270449268,-2.55974451385223,-2.539576440405,-2.53439580388652,-2.53128403103742,
-2.5284912653393,-2.52493207766387,-2.51925395137538,-2.47234923391076,
-2.43822699481459,-2.41769586878694,-2.41423626310104,-2.41237863238761,
-2.41081981419016,-2.40886289163437,-2.40504828847699,-2.37562615832027,
-2.33099119488012,-2.31256918888605,-2.30445092556886,-2.29800714996462,
-2.29462413902028,-2.2921146254149,-2.28897782975844,-2.28368350035004,
-2.26466322980464,-2.20645409360217,-2.18283200059918,-2.17773645042245,
-2.17556470967348,-2.17398128192594,-2.17225211407082,-2.16938104854387,
-2.15980583077156,-2.08445323571059,-2.06464477732774,-2.05949361222313,
-2.05638845953858,-2.0535945966867,-2.0500243021211,-2.04430875089033,-2.00051510395259,
-1.9741853308782,-1.94601888246039,-1.94046026157136,-1.93821165745488,
-1.93661525445993,-1.935124746125,-1.9325880315953,-1.92562937001219,-1.84720915285884,
-1.8272084820429,-1.82204226805781,-1.81893416595458,-1.81614153235007,
-1.8125781609117,-1.80688454806761,-1.76065567559184,-1.72778263756613,
-1.70549511554985,-1.70197207976544,-1.70010129424701,-1.69854356529405,
-1.69660317414098,-1.69286413337185,-1.66826508452444,-1.62623090197975,
-1.59449671209507,-1.58658218442793,-1.58291072773492,-1.5801042526633,
-1.5770511491648,-1.57213522940316,-1.55670372546374,-1.51236511191743),
 .UNSPECIFIED.);
#778=B_SPLINE_CURVE_WITH_KNOTS('',3,(#91463,#91464,#91465,#91466,#91467,
#91468,#91469,#91470,#91471,#91472,#91473,#91474,#91475,#91476,#91477,#91478,
#91479,#91480,#91481,#91482,#91483,#91484,#91485,#91486,#91487,#91488,#91489,
#91490,#91491,#91492,#91493,#91494,#91495,#91496,#91497,#91498,#91499,#91500,
#91501,#91502,#91503,#91504,#91505,#91506,#91507,#91508,#91509,#91510,#91511,
#91512,#91513,#91514,#91515,#91516,#91517,#91518,#91519,#91520,#91521,#91522,
#91523,#91524,#91525,#91526,#91527,#91528,#91529,#91530,#91531,#91532,#91533,
#91534,#91535,#91536,#91537,#91538,#91539,#91540,#91541,#91542,#91543,#91544,
#91545,#91546,#91547,#91548,#91549,#91550,#91551,#91552,#91553,#91554,#91555,
#91556,#91557,#91558,#91559,#91560,#91561,#91562,#91563,#91564,#91565,#91566,
#91567,#91568,#91569,#91570,#91571,#91572,#91573,#91574,#91575,#91576,#91577,
#91578,#91579,#91580,#91581,#91582,#91583,#91584,#91585,#91586,#91587,#91588,
#91589,#91590,#91591,#91592,#91593,#91594,#91595,#91596,#91597,#91598,#91599,
#91600,#91601,#91602,#91603,#91604,#91605,#91606,#91607,#91608,#91609,#91610,
#91611,#91612,#91613,#91614,#91615,#91616,#91617,#91618,#91619,#91620,#91621,
#91622,#91623,#91624,#91625,#91626,#91627,#91628,#91629,#91630,#91631,#91632,
#91633,#91634,#91635,#91636,#91637,#91638,#91639,#91640,#91641,#91642,#91643,
#91644,#91645,#91646,#91647,#91648,#91649,#91650,#91651,#91652,#91653,#91654,
#91655,#91656,#91657,#91658,#91659,#91660,#91661,#91662,#91663,#91664,#91665,
#91666,#91667,#91668,#91669,#91670,#91671,#91672,#91673,#91674,#91675,#91676,
#91677,#91678,#91679,#91680,#91681,#91682,#91683,#91684,#91685,#91686,#91687,
#91688,#91689,#91690,#91691,#91692,#91693,#91694),.UNSPECIFIED.,.F.,.F.,
(4,2,2,2,2,2,2,2,2,2,2,2,2,2,2,2,2,2,2,2,2,2,2,2,2,2,2,2,2,2,2,2,2,2,2,
2,2,2,2,2,2,2,2,2,2,2,2,2,2,2,2,2,2,2,2,2,2,2,2,2,2,2,2,2,2,2,2,2,2,2,2,
2,2,2,2,2,2,2,2,2,2,2,2,2,2,2,2,2,2,2,2,2,2,2,2,2,2,2,2,2,2,2,2,2,2,2,2,
2,2,2,2,2,2,2,2,4),(-2.97246426759675,-2.94428574081794,-2.90996217957583,
-2.89016588973709,-2.88676899223866,-2.88494017514404,-2.88340314350309,
-2.8814723279444,-2.87770638484499,-2.84933895332952,-2.79212018654989,
-2.78027704843224,-2.77433950402829,-2.77066477541974,-2.7673103358639,
-2.76726337758087,-2.76721516593046,-2.76716560507966,-2.76711459057286,
-2.76706200825653,-2.767007733038,-2.76695162745497,-2.76689354001511,-2.76683330325438,
-2.76677073146232,-2.76673287228551,-2.76668710395592,-2.76663145067519,
-2.76656328640843,-2.76647903738856,-2.76380019796265,-2.76039106209135,
-2.75512389358505,-2.72781730867969,-2.66551997818784,-2.65647705482015,
-2.65042914807023,-2.64812309915009,-2.64653180714845,-2.64508307526343,
-2.64269159855483,-2.63655176890577,-2.55688483291798,-2.54364427703872,
-2.53422607934513,-2.53032334491243,-2.52750943466185,-2.52494297112302,
-2.52084390286609,-2.51315850818247,-2.45634544574622,-2.41565445024759,
-2.41175123235641,-2.4098177719378,-2.40842839237369,-2.40666147352304,
-2.4036305038161,-2.39185556380835,-2.31871669633103,-2.29909538488013,
-2.29400551909441,-2.29094145532281,-2.28818760734047,-2.28467313648524,
-2.27905783472003,-2.23081981948986,-2.20927589691354,-2.18050600425978,
-2.17491956195657,-2.17268517008435,-2.17110793180426,-2.16964360965937,
-2.16758246032872,-2.16206446171813,-2.11539806428787,-2.06401557545253,
-2.05752568542414,-2.05416201200345,-2.05142167411376,-2.04825821985294,
-2.04285785152711,-2.02134372432541,-1.95861752724636,-1.93956075356723,
-1.93619522147561,-1.93437323782737,-1.93283594686783,-1.93089719571369,
-1.92709341352371,-1.89311012534219,-1.84427006320665,-1.82406944758419,
-1.81893269899672,-1.81585822411878,-1.81310623374272,-1.80960948252501,
-1.80405335747445,-1.76860196801606,-1.70821883244269,-1.70043367452667,
-1.6978934053952,-1.69625268564684,-1.69467643079905,-1.69236591784739,
-1.68671321777781,-1.64268482863225,-1.60556522932953,-1.58633464690745,
-1.5812766338537,-1.57821925374063,-1.57546344230171,-1.57193543315433,
-1.56627604415298,-1.523915700132,-1.49489594417815,-1.47769960275031),
 .UNSPECIFIED.);
#779=B_SPLINE_CURVE_WITH_KNOTS('',3,(#91695,#91696,#91697,#91698,#91699,
#91700,#91701,#91702,#91703,#91704,#91705,#91706,#91707,#91708,#91709,#91710,
#91711,#91712,#91713,#91714,#91715,#91716,#91717,#91718,#91719,#91720,#91721,
#91722,#91723,#91724,#91725,#91726,#91727,#91728,#91729,#91730,#91731,#91732,
#91733,#91734,#91735,#91736,#91737,#91738,#91739,#91740,#91741,#91742,#91743,
#91744,#91745,#91746,#91747,#91748,#91749,#91750,#91751,#91752,#91753,#91754,
#91755,#91756,#91757,#91758,#91759,#91760,#91761,#91762,#91763,#91764,#91765,
#91766,#91767,#91768,#91769,#91770,#91771,#91772,#91773,#91774,#91775,#91776,
#91777,#91778,#91779,#91780,#91781,#91782,#91783,#91784,#91785,#91786,#91787,
#91788,#91789,#91790,#91791,#91792,#91793,#91794,#91795,#91796,#91797,#91798,
#91799,#91800,#91801,#91802,#91803,#91804,#91805,#91806,#91807,#91808,#91809,
#91810,#91811,#91812,#91813,#91814,#91815,#91816,#91817,#91818,#91819,#91820,
#91821,#91822,#91823,#91824,#91825,#91826,#91827,#91828,#91829,#91830,#91831,
#91832,#91833,#91834,#91835,#91836,#91837,#91838,#91839,#91840,#91841,#91842,
#91843,#91844,#91845,#91846,#91847,#91848,#91849,#91850,#91851,#91852,#91853,
#91854,#91855,#91856,#91857,#91858,#91859,#91860,#91861,#91862,#91863,#91864,
#91865,#91866,#91867,#91868,#91869,#91870,#91871,#91872,#91873,#91874,#91875,
#91876,#91877,#91878,#91879,#91880,#91881,#91882,#91883,#91884,#91885,#91886,
#91887,#91888,#91889,#91890,#91891,#91892,#91893,#91894,#91895,#91896,#91897,
#91898,#91899,#91900,#91901,#91902,#91903,#91904,#91905,#91906,#91907,#91908,
#91909,#91910,#91911,#91912,#91913,#91914,#91915,#91916,#91917,#91918,#91919,
#91920,#91921,#91922,#91923,#91924,#91925,#91926,#91927,#91928,#91929,#91930,
#91931,#91932,#91933,#91934,#91935,#91936,#91937,#91938,#91939,#91940,#91941,
#91942,#91943,#91944,#91945,#91946,#91947,#91948,#91949,#91950,#91951,#91952,
#91953,#91954,#91955,#91956,#91957,#91958,#91959,#91960,#91961,#91962,#91963,
#91964,#91965,#91966,#91967,#91968,#91969,#91970,#91971,#91972,#91973,#91974,
#91975,#91976),.UNSPECIFIED.,.F.,.F.,(4,2,2,2,2,2,2,2,2,2,2,2,2,2,2,2,2,
2,2,2,2,2,2,2,2,2,2,2,2,2,2,2,2,2,2,2,2,2,2,2,2,2,2,2,2,2,2,2,2,2,2,2,2,
2,2,2,2,2,2,2,2,2,2,2,2,2,2,2,2,2,2,2,2,2,2,2,2,2,2,2,2,2,2,2,2,2,2,2,2,
2,2,2,2,2,2,2,2,2,2,2,2,2,2,2,2,2,2,2,2,2,2,2,2,2,2,2,2,2,2,2,2,2,2,2,2,
2,2,2,2,2,2,2,2,2,2,2,2,2,2,2,4),(-1.51236511191743,-1.4948215896375,-1.49400362409459,
-1.4686262163764,-1.46486013725749,-1.46291377811845,-1.46135563468478,
-1.45948956840321,-1.45598953126205,-1.43436545784749,-1.40129123349152,
-1.35458738447322,-1.34890085264416,-1.34533935037137,-1.34254661797046,
-1.33943679163874,-1.33426391057615,-1.31418755447779,-1.23448407677383,
-1.22849661764815,-1.22611105486576,-1.22464927665935,-1.22302674714407,
-1.22064472822501,-1.21421409017876,-1.17585898450047,-1.12070349777977,
-1.11203193682353,-1.10860362801049,-1.10575787131501,-1.10284082721315,
-1.09856174584771,-1.08688270122094,-1.06930549682172,-1.03491814978669,
-0.996807934368717,-0.991010934055789,-0.98865733668245,-0.987056688094282,
-0.985394243751395,-0.982824932782483,-0.974982140855592,-0.962138488487206,
-0.89908744977156,-0.878132810000619,-0.87273123200272,-0.869539910067627,
-0.866758362868686,-0.863321748415991,-0.856617158496879,-0.810483160660005,
-0.758449072260833,-0.75330076096962,-0.75127590533753,-0.749807946169433,
-0.748192075076011,-0.74584281802364,-0.739635693809925,-0.730307904025884,
-0.698969649687284,-0.64601513080894,-0.637409505825225,-0.633898582092195,
-0.631291654220649,-0.628440227631647,-0.624497530493606,-0.615037113819034,
-0.601763357128723,-0.521701258400831,-0.515972104439006,-0.513629449386597,
-0.512030663291464,-0.510364636536567,-0.507780225697981,-0.499816170268663,
-0.4361905531141,-0.404217280394971,-0.398718201639703,-0.395212533062727,
-0.392424615825467,-0.389279062240039,-0.383947298396088,-0.361804048772071,
-0.33592991183649,-0.31582868044134,-0.281346117350063,-0.277517979809964,
-0.27555786474218,-0.273998501583353,-0.27399208436456,-0.27398575997803,
-0.273979526918604,-0.273973383679682,-0.273967328808087,-0.273961360891179,
-0.273955478513309,-0.27394968030636,-0.273943964918542,-0.273938331010769,
-0.273932777292616,-0.273927302477765,-0.273921905325855,-0.273916584600358,
-0.273911339076235,-0.273906167581931,-0.273901068930202,-0.273895873494243,
-0.273890693693645,-0.273885529409582,-0.273880380549952,-0.273875247030761,
-0.273870128752458,-0.273865025622705,-0.273859937564269,-0.273854864488639,
-0.273849806291677,-0.273844762893142,-0.273839734196123,-0.273834720113091,
-0.271942052655923,-0.26829690104547,-0.263555419882261,-0.216788032005356,
-0.171194387149065,-0.162436099933595,-0.158898774665211,-0.156285051731337,
-0.153438617003792,-0.14952552885499,-0.140245801416345,-0.115016960827674,
-0.0927781658392886,-0.0691895211035217,-0.0438288195000823,-0.0400623809339067,
-0.0381155615756425,-0.0365569009571547,-0.0350712717188883,-0.033225308262869,
-0.0304226243911011,-0.0178739340765507),.UNSPECIFIED.);
#780=B_SPLINE_CURVE_WITH_KNOTS('',3,(#91982,#91983,#91984,#91985,#91986,
#91987,#91988,#91989,#91990,#91991,#91992,#91993,#91994,#91995,#91996,#91997,
#91998,#91999,#92000,#92001,#92002,#92003,#92004,#92005,#92006,#92007,#92008,
#92009,#92010,#92011,#92012,#92013,#92014,#92015,#92016,#92017,#92018,#92019,
#92020,#92021,#92022,#92023,#92024,#92025,#92026,#92027,#92028,#92029,#92030,
#92031,#92032,#92033,#92034,#92035,#92036,#92037,#92038,#92039,#92040,#92041,
#92042,#92043,#92044,#92045,#92046,#92047,#92048,#92049,#92050,#92051,#92052,
#92053,#92054,#92055,#92056,#92057,#92058,#92059,#92060,#92061,#92062,#92063,
#92064,#92065,#92066,#92067,#92068,#92069,#92070,#92071,#92072,#92073,#92074,
#92075,#92076,#92077,#92078,#92079,#92080,#92081,#92082,#92083,#92084,#92085,
#92086,#92087,#92088,#92089,#92090,#92091,#92092,#92093,#92094,#92095,#92096,
#92097,#92098,#92099,#92100,#92101,#92102,#92103,#92104,#92105,#92106,#92107,
#92108,#92109,#92110,#92111,#92112,#92113,#92114,#92115,#92116,#92117,#92118,
#92119,#92120,#92121,#92122,#92123,#92124,#92125,#92126,#92127,#92128,#92129,
#92130,#92131,#92132,#92133,#92134,#92135,#92136,#92137,#92138,#92139,#92140,
#92141,#92142,#92143,#92144,#92145,#92146,#92147,#92148,#92149,#92150,#92151,
#92152,#92153,#92154,#92155,#92156,#92157,#92158,#92159,#92160,#92161,#92162,
#92163,#92164,#92165,#92166,#92167,#92168,#92169,#92170,#92171,#92172,#92173,
#92174,#92175,#92176,#92177,#92178,#92179,#92180,#92181,#92182,#92183,#92184,
#92185,#92186,#92187,#92188,#92189,#92190,#92191,#92192,#92193),
 .UNSPECIFIED.,.F.,.F.,(4,2,2,2,2,2,2,2,2,2,2,2,2,2,2,2,2,2,2,2,2,2,2,2,
2,2,2,2,2,2,2,2,2,2,2,2,2,2,2,2,2,2,2,2,2,2,2,2,2,2,2,2,2,2,2,2,2,2,2,2,
2,2,2,2,2,2,2,2,2,2,2,2,2,2,2,2,2,2,2,2,2,2,2,2,2,2,2,2,2,2,2,2,2,2,2,2,
2,2,2,2,2,2,2,2,2,4),(-1.47839118834467,-1.45095636912055,-1.44537329893961,
-1.44186857293672,-1.43911591034736,-1.43604649321691,-1.43093197654453,
-1.41100670082467,-1.33366421286716,-1.32560904346143,-1.32294356624872,
-1.32127520149056,-1.31969779651749,-1.31746385772411,-1.31188202252239,
-1.28317035018332,-1.26091841659239,-1.21338190405584,-1.20775267528002,
-1.20423360579058,-1.20147871739787,-1.19841613345648,-1.19333492704895,
-1.1738288454657,-1.10212440440244,-1.08892818122723,-1.08578077306755,
-1.08398682614121,-1.08244622254558,-1.0804684196035,-1.07634192919891,
-1.0410724444422,-0.978275102116205,-0.970361939853126,-0.966759401066234,
-0.963984821375909,-0.960992756106465,-0.956233341792901,-0.94022274305942,
-0.91255406991436,-0.873157454503169,-0.86906858727658,-0.851757904462305,
-0.848645297781779,-0.846692997117287,-0.845154475220216,-0.843342156957157,
-0.840023079864386,-0.822009788578399,-0.768673086976097,-0.737666115300506,
-0.732247079219614,-0.728791353776895,-0.726042973695466,-0.722942237806137,
-0.717688134252357,-0.695951476298799,-0.645206635634953,-0.614781252007789,
-0.610988811120715,-0.609052174384358,-0.607514622819395,-0.605690034427372,
-0.602313718855116,-0.58301847102543,-0.517581385307539,-0.498629697051033,
-0.49338592555714,-0.490287559847187,-0.487813871032943,-0.484486115670155,
-0.478172868897464,-0.423656670184969,-0.379935623237664,-0.374276825182988,
-0.37196509667068,-0.370388446901074,-0.368747734352966,-0.36620821980778,
-0.358431011873107,-0.298060309273393,-0.262608566949414,-0.257056554254677,
-0.253560672557908,-0.250883899562267,-0.247899377736921,-0.244772291537913,
-0.240157891697143,-0.231878246545897,-0.212829614210536,-0.170270027584861,
-0.139504304325582,-0.135708801052885,-0.13377159913348,-0.132234126686058,
-0.130410254847438,-0.12703689157107,-0.107806403759334,-0.0350839837826959,
-0.0220026728155107,-0.0174283316283289,-0.0144770441191171,-0.011853202522377,
-0.00913930033583054,-0.0051879348728483,-0.000704354964600651),
 .UNSPECIFIED.);
#781=B_SPLINE_CURVE_WITH_KNOTS('',3,(#92194,#92195,#92196,#92197),
 .UNSPECIFIED.,.F.,.F.,(4,4),(-2.98975612156922,-2.97246426759675),
 .UNSPECIFIED.);
#782=B_SPLINE_CURVE_WITH_KNOTS('',3,(#92199,#92200,#92201,#92202),
 .UNSPECIFIED.,.F.,.F.,(4,4),(-0.0178739340765507,-0.000702727300234043),
 .UNSPECIFIED.);
#783=B_SPLINE_CURVE_WITH_KNOTS('',3,(#92203,#92204,#92205,#92206,#92207,
#92208,#92209,#92210,#92211,#92212,#92213,#92214,#92215,#92216,#92217,#92218,
#92219,#92220,#92221,#92222,#92223,#92224,#92225,#92226,#92227,#92228,#92229,
#92230,#92231,#92232,#92233,#92234,#92235,#92236,#92237,#92238,#92239,#92240,
#92241,#92242,#92243,#92244,#92245,#92246,#92247,#92248,#92249,#92250,#92251,
#92252,#92253,#92254,#92255,#92256,#92257,#92258,#92259,#92260,#92261,#92262,
#92263,#92264,#92265,#92266,#92267,#92268,#92269,#92270,#92271,#92272,#92273,
#92274,#92275,#92276,#92277,#92278,#92279,#92280,#92281,#92282,#92283,#92284,
#92285,#92286,#92287,#92288,#92289,#92290,#92291,#92292,#92293,#92294,#92295,
#92296,#92297,#92298,#92299,#92300,#92301,#92302,#92303,#92304,#92305,#92306,
#92307,#92308,#92309,#92310,#92311,#92312,#92313,#92314,#92315,#92316,#92317,
#92318,#92319,#92320,#92321,#92322,#92323,#92324,#92325,#92326,#92327,#92328,
#92329,#92330,#92331,#92332,#92333,#92334,#92335,#92336,#92337,#92338,#92339,
#92340,#92341,#92342,#92343,#92344,#92345,#92346,#92347,#92348,#92349,#92350,
#92351,#92352,#92353,#92354,#92355,#92356,#92357,#92358,#92359,#92360,#92361,
#92362,#92363,#92364,#92365,#92366,#92367,#92368,#92369,#92370,#92371,#92372,
#92373,#92374,#92375,#92376,#92377,#92378,#92379,#92380,#92381,#92382,#92383,
#92384,#92385,#92386,#92387,#92388,#92389,#92390,#92391,#92392,#92393,#92394,
#92395,#92396,#92397,#92398,#92399,#92400,#92401,#92402,#92403,#92404,#92405,
#92406,#92407,#92408,#92409,#92410,#92411,#92412,#92413,#92414,#92415,#92416,
#92417,#92418,#92419,#92420,#92421,#92422),.UNSPECIFIED.,.F.,.F.,(4,2,2,
2,2,2,2,2,2,2,2,2,2,2,2,2,2,2,2,2,2,2,2,2,2,2,2,2,2,2,2,2,2,2,2,2,2,2,2,
2,2,2,2,2,2,2,2,2,2,2,2,2,2,2,2,2,2,2,2,2,2,2,2,2,2,2,2,2,2,2,2,2,2,2,2,
2,2,2,2,2,2,2,2,2,2,2,2,2,2,2,2,2,2,2,2,2,2,2,2,2,2,2,2,2,2,2,2,2,2,4),
(-2.99059624599852,-2.9242269223958,-2.91484635816592,-2.91091609311936,
-2.90806621662461,-2.9054555721249,-2.90193187652571,-2.89325567514184,
-2.84195233375899,-2.80933436231326,-2.7997928408015,-2.79549955961913,
-2.79217521726917,-2.79032884837834,-2.79031978580954,-2.79031065100499,
-2.79030144276184,-2.79029215985547,-2.79028280104057,-2.79027336503898,
-2.79026385053848,-2.78870416076414,-2.78674269667096,-2.78290918305818,
-2.75140408109271,-2.70262416901521,-2.68034235362197,-2.67500025006063,
-2.67185214251293,-2.6690641299345,-2.66556123485124,-2.66007212298071,
-2.62895195110776,-2.57592712444011,-2.56384755845483,-2.55878755814963,
-2.55490781320999,-2.55296243914939,-2.55155433979417,-2.54974801588207,
-2.54661335092271,-2.53395567319923,-2.46257647063955,-2.44245820461646,
-2.43728027403617,-2.43416837224634,-2.43137438113979,-2.42781210640301,
-2.42212597065061,-2.37519058377616,-2.34105416971642,-2.32054003592188,
-2.31708011969652,-2.31522201124306,-2.31366260861524,-2.31170472091216,
-2.30788756352151,-2.27187050128496,-2.23287930582103,-2.21502101546436,
-2.20320307331589,-2.1989039794478,-2.19598223686012,-2.19313874864965,
-2.18972143305987,-2.1811232000435,-2.12479050938735,-2.0838513959763,-2.07990508347753,
-2.07794634050091,-2.07653690611172,-2.07474031594477,-2.07164783240144,
-2.05948630112066,-1.98753123604281,-1.96741543148461,-1.9622378155508,
-1.95912604737941,-1.95633214113734,-1.95276992633491,-1.9470837886204,
-1.90019779637242,-1.86605451885922,-1.84550407659311,-1.84204282821988,
-1.84018447315634,-1.8386251401515,-1.8366676886051,-1.83285239514693,-1.80346600214544,
-1.75879938133016,-1.74035285224361,-1.732226303213,-1.72577686113148,-1.72239199172821,
-1.71988156547474,-1.71674423261773,-1.71145046261991,-1.69244815616754,
-1.62724459885455,-1.61426188279019,-1.60894437127265,-1.60491053696014,
-1.60293434433125,-1.60137377339904,-1.59953002350305,-1.5962311918276,
-1.58133402829854,-1.53724996492306,-1.51291820589149),.UNSPECIFIED.);
#784=B_SPLINE_CURVE_WITH_KNOTS('',3,(#92427,#92428,#92429,#92430,#92431,
#92432,#92433,#92434,#92435,#92436,#92437,#92438,#92439,#92440,#92441,#92442,
#92443,#92444,#92445,#92446,#92447,#92448,#92449,#92450,#92451,#92452,#92453,
#92454,#92455,#92456,#92457,#92458,#92459,#92460,#92461,#92462,#92463,#92464,
#92465,#92466,#92467,#92468,#92469,#92470,#92471,#92472,#92473,#92474,#92475,
#92476,#92477,#92478,#92479,#92480,#92481,#92482,#92483,#92484,#92485,#92486,
#92487,#92488,#92489,#92490,#92491,#92492,#92493,#92494,#92495,#92496,#92497,
#92498,#92499,#92500,#92501,#92502,#92503,#92504,#92505,#92506,#92507,#92508,
#92509,#92510,#92511,#92512,#92513,#92514,#92515,#92516,#92517,#92518,#92519,
#92520,#92521,#92522,#92523,#92524,#92525,#92526,#92527,#92528,#92529,#92530,
#92531,#92532,#92533,#92534,#92535,#92536,#92537,#92538,#92539,#92540,#92541,
#92542,#92543,#92544,#92545,#92546,#92547,#92548,#92549,#92550,#92551,#92552,
#92553,#92554,#92555,#92556,#92557,#92558,#92559,#92560,#92561,#92562,#92563,
#92564,#92565,#92566,#92567,#92568,#92569,#92570,#92571,#92572,#92573,#92574,
#92575,#92576,#92577,#92578,#92579,#92580,#92581,#92582,#92583,#92584,#92585,
#92586,#92587,#92588,#92589,#92590,#92591,#92592,#92593,#92594,#92595,#92596,
#92597,#92598,#92599,#92600,#92601,#92602,#92603,#92604,#92605,#92606,#92607,
#92608,#92609,#92610,#92611,#92612,#92613,#92614,#92615,#92616,#92617,#92618,
#92619,#92620,#92621,#92622,#92623,#92624,#92625,#92626,#92627,#92628,#92629,
#92630,#92631,#92632,#92633,#92634,#92635,#92636,#92637,#92638,#92639,#92640,
#92641,#92642),.UNSPECIFIED.,.F.,.F.,(4,2,2,2,2,2,2,2,2,2,2,2,2,2,2,2,2,
2,2,2,2,2,2,2,2,2,2,2,2,2,2,2,2,2,2,2,2,2,2,2,2,2,2,2,2,2,2,2,2,2,2,2,2,
2,2,2,2,2,2,2,2,2,2,2,2,2,2,2,2,2,2,2,2,2,2,2,2,2,2,2,2,2,2,2,2,2,2,2,2,
2,2,2,2,2,2,2,2,2,2,2,2,2,2,2,2,2,2,4),(-2.97248562834132,-2.97156067933371,
-2.92779150390965,-2.89482030744997,-2.88122261515143,-2.87161212394087,
-2.86767910884108,-2.86486045668559,-2.86230124776594,-2.85823872603261,
-2.85068782170555,-2.79219885096846,-2.75320557359479,-2.75037087584259,
-2.74795483399847,-2.74635691748857,-2.74482281563557,-2.74251618904016,
-2.73693120885304,-2.69188411114417,-2.65549220308016,-2.64293575198332,
-2.6338934714932,-2.6300539303029,-2.62725204622808,-2.62467327904287,-2.62117458734169,
-2.61247037738203,-2.56440112423484,-2.52915208832837,-2.51922798216468,
-2.51274719725168,-2.51037868804558,-2.50877525212609,-2.50733908456329,
-2.50501259985502,-2.49926082391095,-2.46296783804852,-2.45454866340838,
-2.40276126678399,-2.3955331936639,-2.39202237701551,-2.3892695476409,-2.3862047134983,
-2.38110908961234,-2.36364773451225,-2.35371713560661,-2.2957031459866,
-2.2771300555768,-2.27378642938069,-2.27196939875307,-2.27043212752409,
-2.26848811038663,-2.26540122916047,-2.24857803336442,-2.24445110911132,
-2.20289676623316,-2.16701696938553,-2.1586402971301,-2.15491575147548,
-2.1521330536444,-2.14952541671011,-2.14591428070777,-2.13652612784976,
-2.0755488971694,-2.07260000324708,-2.04311270407503,-2.03745930787644,
-2.03521444513661,-2.03363537947384,-2.03217381233665,-2.03012259874889,
-2.02467733277743,-1.97632597719324,-1.92650570480663,-1.9200385457438,
-1.91667975848291,-1.91393997325214,-1.91077332544168,-1.90535812303464,
-1.88363218370009,-1.82113371858248,-1.80835073044198,-1.80055751824542,
-1.79801660501411,-1.79637597061917,-1.7948002274363,-1.79249112890348,
-1.78684520515815,-1.74266300998612,-1.68862719191158,-1.68234608578561,
-1.67902568349406,-1.67655340916266,-1.67345153968695,-1.66818889860627,
-1.64902769629626,-1.59030518084118,-1.56710458084776,-1.56208332154418,
-1.55994244870059,-1.55838149760638,-1.55667828589076,-1.55385481097013,
-1.54448582904813,-1.49596156717328,-1.48741829385312,-1.47839118834467),
 .UNSPECIFIED.);
#785=B_SPLINE_CURVE_WITH_KNOTS('',3,(#92643,#92644,#92645,#92646,#92647,
#92648,#92649,#92650,#92651,#92652,#92653,#92654,#92655,#92656,#92657,#92658,
#92659,#92660,#92661,#92662,#92663,#92664,#92665,#92666,#92667,#92668,#92669,
#92670,#92671,#92672,#92673,#92674,#92675,#92676,#92677,#92678,#92679,#92680,
#92681,#92682,#92683,#92684,#92685,#92686,#92687,#92688,#92689,#92690,#92691,
#92692,#92693,#92694,#92695,#92696,#92697,#92698,#92699,#92700,#92701,#92702,
#92703,#92704,#92705,#92706,#92707,#92708,#92709,#92710,#92711,#92712,#92713,
#92714,#92715,#92716,#92717,#92718,#92719,#92720,#92721,#92722,#92723,#92724,
#92725,#92726,#92727,#92728,#92729,#92730,#92731,#92732,#92733,#92734,#92735,
#92736,#92737,#92738,#92739,#92740,#92741,#92742,#92743,#92744,#92745,#92746,
#92747,#92748,#92749,#92750,#92751,#92752,#92753,#92754,#92755,#92756,#92757,
#92758,#92759,#92760,#92761,#92762,#92763,#92764,#92765,#92766,#92767,#92768,
#92769,#92770,#92771,#92772,#92773,#92774,#92775,#92776,#92777,#92778,#92779,
#92780,#92781,#92782,#92783,#92784,#92785,#92786,#92787,#92788,#92789,#92790,
#92791,#92792,#92793,#92794,#92795,#92796,#92797,#92798,#92799,#92800,#92801,
#92802,#92803,#92804,#92805,#92806,#92807,#92808,#92809,#92810,#92811,#92812,
#92813,#92814,#92815,#92816,#92817,#92818,#92819,#92820,#92821,#92822,#92823,
#92824,#92825,#92826,#92827,#92828,#92829,#92830,#92831,#92832,#92833,#92834,
#92835,#92836,#92837,#92838,#92839,#92840,#92841,#92842,#92843,#92844,#92845,
#92846,#92847,#92848,#92849,#92850,#92851,#92852,#92853,#92854,#92855,#92856,
#92857,#92858,#92859,#92860,#92861,#92862,#92863,#92864),.UNSPECIFIED.,
 .F.,.F.,(4,2,2,2,2,2,2,2,2,2,2,2,2,2,2,2,2,2,2,2,2,2,2,2,2,2,2,2,2,2,2,
2,2,2,2,2,2,2,2,2,2,2,2,2,2,2,2,2,2,2,2,2,2,2,2,2,2,2,2,2,2,2,2,2,2,2,2,
2,2,2,2,2,2,2,2,2,2,2,2,2,2,2,2,2,2,2,2,2,2,2,2,2,2,2,2,2,2,2,2,2,2,2,2,
2,2,2,2,2,2,2,4),(-1.51291820589149,-1.4955978501673,-1.48868563564395,
-1.48515958090633,-1.48236927418393,-1.4792355956776,-1.47395934358364,
-1.45258156693988,-1.40774651121575,-1.39814287532211,-1.39125436101471,
-1.38469601357356,-1.37027237891115,-1.36700520915586,-1.36516865993728,
-1.36360747038655,-1.36162191430467,-1.35754059874169,-1.31506918560559,
-1.26071560156739,-1.25217413289291,-1.24867362219442,-1.24606869615536,
-1.24321384459742,-1.23925603562992,-1.22970817259507,-1.21627480175101,
-1.17735411016549,-1.13665444913826,-1.13089091199475,-1.12854244651807,
-1.12694244794468,-1.12527787594811,-1.12270043278592,-1.11479495463648,
-1.10180896135062,-1.03646880836714,-1.01762887845479,-1.0123507382666,
-1.00921685979573,-1.00670596413038,-1.0033162333797,-0.996843212778155,
-0.944436665893327,-0.929806331542807,-0.896218114977467,-0.892377260588701,
-0.890414330512949,-0.888854690317843,-0.887000759865873,-0.883560393997282,
-0.863532135212415,-0.787676746748735,-0.777698074474476,-0.773556075634001,
-0.770955404364455,-0.768097728760838,-0.764122082939013,-0.754461607785713,
-0.740819107303395,-0.70080783134114,-0.661610252602209,-0.655832266435037,
-0.653481690264618,-0.651881518153566,-0.650218012661907,-0.647644376192594,
-0.639767442918814,-0.626845996292329,-0.562559155746558,-0.542781723749043,
-0.537403610299997,-0.534248213692101,-0.531740845457862,-0.528382622219717,
-0.522059151776543,-0.46866436682011,-0.423915385958649,-0.418283072930048,
-0.416187484704163,-0.414700774212505,-0.413100850080367,-0.410834895896314,
-0.405170458648868,-0.375901850055044,-0.324134490002468,-0.30516131607259,
-0.299870942016026,-0.296734672891897,-0.294224573873341,-0.29156394675692,
-0.28634126755948,-0.264783519583157,-0.218837360639595,-0.183759298884581,
-0.179918406396861,-0.1779556362976,-0.176396218387824,-0.174542664724284,
-0.172561949813693,-0.164207609181587,-0.134872067375431,-0.106976169080335,
-0.0695224092823296,-0.0638646567633502,-0.0603111449863071,-0.0575184479006353,
-0.0544022074428103,-0.0511775410252991,-0.0463683924039305,-0.0183031829186653),
 .UNSPECIFIED.);
#786=B_SPLINE_CURVE_WITH_KNOTS('',3,(#92870,#92871,#92872,#92873,#92874,
#92875,#92876,#92877,#92878,#92879),.UNSPECIFIED.,.F.,.F.,(4,1,1,1,1,1,
1,4),(72.2566346161759,73.2298488044367,74.2286545160064,75.2274602275762,
76.226265939146,77.2250716507158,78.2238773622855,78.4676963535106),
 .UNSPECIFIED.);
#787=B_SPLINE_CURVE_WITH_KNOTS('',3,(#92880,#92881,#92882,#92883,#92884,
#92885,#92886,#92887,#92888,#92889,#92890,#92891,#92892,#92893,#92894,#92895),
 .UNSPECIFIED.,.F.,.F.,(4,2,2,2,2,2,2,4),(-2.98981850197706,-2.98825670069322,
-2.98643438083612,-2.98490201067196,-2.98342035314125,-2.98192681857162,
-2.97930338862327,-2.97248562834132),.UNSPECIFIED.);
#788=B_SPLINE_CURVE_WITH_KNOTS('',3,(#92897,#92898,#92899,#92900),
 .UNSPECIFIED.,.F.,.F.,(4,4),(-0.0183031829186653,-0.000703111691500607),
 .UNSPECIFIED.);
#789=B_SPLINE_CURVE_WITH_KNOTS('',3,(#92901,#92902,#92903,#92904,#92905,
#92906,#92907,#92908,#92909,#92910),.UNSPECIFIED.,.F.,.F.,(4,1,1,1,1,1,
1,4),(72.2566333488475,72.5142287899751,73.5125762644367,74.5109237388983,
75.5092712133598,76.5076186878214,77.505966162283,78.4665403893118),
 .UNSPECIFIED.);
#790=B_SPLINE_CURVE_WITH_KNOTS('',3,(#92916,#92917,#92918,#92919,#92920,
#92921,#92922,#92923,#92924,#92925,#92926,#92927,#92928,#92929,#92930,#92931,
#92932,#92933,#92934,#92935,#92936,#92937,#92938,#92939,#92940,#92941,#92942,
#92943,#92944,#92945,#92946,#92947,#92948,#92949,#92950,#92951,#92952,#92953,
#92954,#92955,#92956,#92957,#92958,#92959,#92960,#92961,#92962,#92963,#92964,
#92965,#92966,#92967,#92968,#92969,#92970,#92971,#92972,#92973,#92974,#92975,
#92976,#92977,#92978,#92979,#92980,#92981,#92982,#92983,#92984,#92985,#92986,
#92987,#92988,#92989,#92990,#92991,#92992,#92993,#92994,#92995,#92996,#92997,
#92998,#92999,#93000,#93001,#93002,#93003,#93004,#93005,#93006,#93007,#93008,
#93009,#93010,#93011,#93012,#93013,#93014,#93015,#93016,#93017,#93018,#93019,
#93020,#93021,#93022,#93023,#93024,#93025,#93026,#93027,#93028,#93029,#93030,
#93031,#93032,#93033,#93034,#93035,#93036,#93037,#93038,#93039,#93040,#93041,
#93042,#93043,#93044,#93045,#93046,#93047,#93048,#93049,#93050,#93051,#93052,
#93053,#93054,#93055,#93056,#93057,#93058,#93059,#93060,#93061,#93062,#93063,
#93064,#93065,#93066,#93067,#93068,#93069,#93070,#93071,#93072,#93073,#93074,
#93075,#93076,#93077,#93078,#93079,#93080,#93081,#93082,#93083,#93084,#93085,
#93086,#93087,#93088,#93089,#93090,#93091,#93092,#93093,#93094,#93095,#93096,
#93097,#93098,#93099,#93100,#93101,#93102,#93103,#93104,#93105),
 .UNSPECIFIED.,.F.,.F.,(4,3,3,3,3,3,3,3,3,3,3,3,3,3,3,3,3,3,3,3,3,3,3,3,
3,3,3,3,3,3,3,3,3,3,3,3,3,3,3,3,3,3,3,3,3,3,3,3,3,3,3,3,3,3,3,3,3,3,3,3,
3,3,3,4),(78.5398163397449,78.639625262068,78.7394070013408,78.8391931746706,
78.9390862524863,79.0390332714625,79.1391646313106,79.2226830738553,79.32318239275,
79.4235362419029,79.5237730469281,79.6239458180325,79.7240858152806,79.8242242576787,
79.9244626898268,80.0247490873905,80.125218688962,80.2214887854251,80.3219881043198,
80.4223419534728,80.5225787584979,80.6227515296023,80.7228915268504,80.8230299692488,
80.923268401397,81.0235547989607,81.1240244005322,81.2202944969949,81.3207938158895,
81.4211476650429,81.5213844700679,81.6215572411723,81.7216972384203,81.8218356808185,
81.9220741129666,82.0223605105304,82.1228301121019,82.2191002085647,82.3195995274593,
82.4199533766122,82.5201901816374,82.6203629527417,82.7205029499898,82.8206413923881,
82.9208798245363,83.0211662220999,83.1216358236714,83.2179059201344,83.318405239029,
83.4187590881821,83.5189958932072,83.6191686643116,83.7193086615596,83.8194471039578,
83.9196855361059,84.0199719336696,84.1204415352411,84.2167116317042,84.3185060059812,
84.4201415989636,84.5216223522047,84.6230133414407,84.7243377755445,84.7497329240609),
 .UNSPECIFIED.);
#791=B_SPLINE_CURVE_WITH_KNOTS('',3,(#93106,#93107,#93108,#93109),
 .UNSPECIFIED.,.F.,.F.,(4,4),(78.4676963535106,78.539809789393),
 .UNSPECIFIED.);
#792=B_SPLINE_CURVE_WITH_KNOTS('',3,(#93111,#93112,#93113,#93114,#93115),
 .UNSPECIFIED.,.F.,.F.,(4,1,4),(78.4665403893118,78.5043136367446,78.5398163397449),
 .UNSPECIFIED.);
#793=B_SPLINE_CURVE_WITH_KNOTS('',3,(#93116,#93117,#93118,#93119,#93120,
#93121,#93122,#93123,#93124,#93125,#93126,#93127,#93128,#93129,#93130,#93131,
#93132,#93133,#93134,#93135,#93136,#93137,#93138,#93139,#93140,#93141,#93142,
#93143,#93144,#93145,#93146,#93147,#93148,#93149,#93150,#93151,#93152,#93153,
#93154,#93155,#93156,#93157,#93158,#93159,#93160,#93161,#93162,#93163,#93164,
#93165,#93166,#93167,#93168,#93169,#93170,#93171,#93172,#93173,#93174,#93175,
#93176,#93177,#93178,#93179,#93180,#93181,#93182,#93183,#93184,#93185,#93186,
#93187,#93188,#93189,#93190,#93191,#93192,#93193,#93194,#93195,#93196,#93197,
#93198,#93199,#93200,#93201,#93202,#93203,#93204,#93205,#93206,#93207,#93208,
#93209,#93210,#93211,#93212,#93213,#93214,#93215,#93216,#93217,#93218,#93219,
#93220,#93221,#93222,#93223,#93224,#93225,#93226,#93227,#93228,#93229,#93230,
#93231,#93232,#93233,#93234,#93235,#93236,#93237,#93238,#93239,#93240,#93241,
#93242,#93243,#93244,#93245,#93246,#93247,#93248,#93249,#93250,#93251,#93252,
#93253,#93254,#93255,#93256,#93257,#93258,#93259,#93260,#93261,#93262,#93263,
#93264,#93265,#93266,#93267,#93268,#93269,#93270,#93271,#93272,#93273,#93274,
#93275,#93276,#93277,#93278,#93279,#93280,#93281,#93282,#93283,#93284,#93285,
#93286,#93287,#93288,#93289,#93290,#93291,#93292,#93293,#93294,#93295,#93296,
#93297,#93298,#93299,#93300,#93301,#93302,#93303,#93304,#93305,#93306,#93307,
#93308,#93309,#93310,#93311,#93312,#93313,#93314,#93315,#93316,#93317,#93318,
#93319,#93320,#93321,#93322,#93323,#93324,#93325,#93326,#93327,#93328,#93329,
#93330,#93331,#93332,#93333,#93334,#93335,#93336,#93337,#93338,#93339,#93340,
#93341,#93342,#93343,#93344,#93345,#93346,#93347,#93348,#93349,#93350,#93351,
#93352,#93353,#93354,#93355,#93356,#93357,#93358,#93359,#93360,#93361,#93362,
#93363,#93364,#93365,#93366,#93367,#93368,#93369,#93370,#93371,#93372,#93373,
#93374,#93375),.UNSPECIFIED.,.F.,.F.,(4,2,2,2,2,2,2,2,2,2,2,2,2,2,2,2,2,
2,2,2,2,2,2,2,2,2,2,2,2,2,2,2,2,2,2,2,2,2,2,2,2,2,2,2,2,2,2,2,2,2,2,2,2,
2,2,2,2,2,2,2,2,2,2,2,2,2,2,2,2,2,2,2,2,2,2,2,2,2,2,2,2,2,2,2,2,2,2,2,2,
2,2,2,2,2,2,2,2,2,2,2,2,2,2,2,2,2,2,2,2,2,2,2,2,2,2,2,2,2,2,2,2,2,2,2,2,
2,2,2,2,4),(-2.98918321660332,-2.95816385181088,-2.93577202507296,-2.89069523414431,
-2.88402815084895,-2.88059982146384,-2.87781962568173,-2.87462394209342,
-2.86920071949568,-2.84794758267391,-2.79111273857183,-2.77436136512357,
-2.76804493994685,-2.76483589798187,-2.76282311984763,-2.76097329392359,
-2.76096402969731,-2.76095470718103,-2.76094532512873,-2.76093588226905,
-2.7609263773134,-2.76091680891982,-2.76090717574813,-2.76089747640838,
-2.76088770946629,-2.76087787346166,-2.76086932728069,-2.76086049556672,
-2.76085136573228,-2.76084192443884,-2.76083215756958,-2.76082205013897,
-2.76081158621808,-2.7608007488897,-2.7607895201406,-2.76077788078478,-2.76076581036865,
-2.76075328703221,-2.76074028741406,-2.76072678651303,-2.76071275751994,
-2.76069817166731,-2.76068299803468,-2.75916438941005,-2.75714271292296,
-2.75377154592753,-2.73066323607994,-2.6878483444427,-2.65224654810353,
-2.64624469757052,-2.64295501287312,-2.64045364117898,-2.637244593841,-2.63176366149767,
-2.60979175848285,-2.56164472036491,-2.53224333909891,-2.5265678937192,
-2.5243007093267,-2.52270101597106,-2.52121539971995,-2.51912257331459,
-2.51350581557904,-2.46840195072964,-2.41553377784689,-2.40915183393897,
-2.40578216065481,-2.40327449972437,-2.40012954589255,-2.39479583053783,
-2.37535329006914,-2.31067656099045,-2.29773035565358,-2.28984414379551,
-2.28726989190211,-2.28560661485491,-2.28400719119716,-2.28165854850609,
-2.27588942505212,-2.23593615520927,-2.19654612010038,-2.17606815486324,
-2.17086317867483,-2.16774624553651,-2.16495480324629,-2.16140545397049,
-2.15575943518954,-2.1187804145423,-2.09649100125249,-2.05507100136872,
-2.05105560410942,-2.04908372342199,-2.04752422318301,-2.04567899266631,
-2.04237092389592,-2.02731246570253,-1.96394665140559,-1.93923412418153,
-1.93373316610162,-1.93055150887982,-1.92776963020741,-1.9243212759911,
-1.91900735559468,-1.89178198770894,-1.82898193403814,-1.82033144839511,
-1.81446611330096,-1.81216895684591,-1.81056348482962,-1.80908474756827,
-1.80701811608384,-1.80159887350359,-1.75258133540274,-1.70318405765312,
-1.69689975705287,-1.69355021613779,-1.69104415138619,-1.68788357484666,
-1.6824796494565,-1.66238598030677,-1.59841549512706,-1.58551109254505,
-1.57764280506907,-1.57507054090084,-1.57340756950339,-1.57180759641025,
-1.56945684072133,-1.56367600732907,-1.52672374711719,-1.51256178469963),
 .UNSPECIFIED.);
#794=B_SPLINE_CURVE_WITH_KNOTS('',3,(#93381,#93382,#93383,#93384,#93385,
#93386,#93387,#93388,#93389,#93390,#93391,#93392,#93393,#93394,#93395,#93396,
#93397,#93398,#93399,#93400,#93401,#93402,#93403,#93404,#93405,#93406,#93407,
#93408,#93409,#93410,#93411,#93412,#93413,#93414,#93415,#93416,#93417,#93418,
#93419,#93420,#93421,#93422,#93423,#93424,#93425,#93426,#93427,#93428,#93429,
#93430,#93431,#93432,#93433,#93434,#93435,#93436,#93437,#93438,#93439,#93440,
#93441,#93442,#93443,#93444,#93445,#93446,#93447,#93448,#93449,#93450,#93451,
#93452,#93453,#93454,#93455,#93456,#93457,#93458,#93459,#93460,#93461,#93462,
#93463,#93464,#93465,#93466,#93467,#93468,#93469,#93470,#93471,#93472,#93473,
#93474,#93475,#93476,#93477,#93478,#93479,#93480,#93481,#93482,#93483,#93484,
#93485,#93486,#93487,#93488,#93489,#93490,#93491,#93492,#93493,#93494,#93495,
#93496,#93497,#93498,#93499,#93500,#93501,#93502,#93503,#93504,#93505,#93506,
#93507,#93508,#93509,#93510,#93511,#93512,#93513,#93514,#93515,#93516,#93517,
#93518,#93519,#93520,#93521,#93522,#93523,#93524,#93525,#93526,#93527,#93528,
#93529,#93530,#93531,#93532,#93533,#93534,#93535,#93536,#93537,#93538,#93539,
#93540,#93541,#93542,#93543,#93544,#93545,#93546,#93547,#93548,#93549,#93550,
#93551,#93552,#93553,#93554,#93555,#93556,#93557,#93558,#93559,#93560,#93561,
#93562,#93563,#93564,#93565,#93566,#93567,#93568,#93569,#93570,#93571,#93572,
#93573,#93574,#93575,#93576,#93577,#93578,#93579,#93580,#93581,#93582),
 .UNSPECIFIED.,.F.,.F.,(4,2,2,2,2,2,2,2,2,2,2,2,2,2,2,2,2,2,2,2,2,2,2,2,
2,2,2,2,2,2,2,2,2,2,2,2,2,2,2,2,2,2,2,2,2,2,2,2,2,2,2,2,2,2,2,2,2,2,2,2,
2,2,2,2,2,2,2,2,2,2,2,2,2,2,2,2,2,2,2,2,2,2,2,2,2,2,2,2,2,2,2,2,2,2,2,2,
2,2,2,2,4),(-1.4782746125791,-1.4396509137331,-1.41159399107955,-1.40628973330349,
-1.40286868537309,-1.40012300583755,-1.39699852779614,-1.3916375036407,
-1.36836690740716,-1.31437602389714,-1.28881210494715,-1.28507576076022,
-1.28315093326428,-1.28161373742846,-1.27977885810151,-1.27635514245457,
-1.25590198451957,-1.22168177215044,-1.17457442239032,-1.16893949385635,
-1.16541820877157,-1.16266241707564,-1.15959968362865,-1.15452023412004,
-1.13504694935018,-1.09711966574836,-1.05413364404067,-1.04844892312133,
-1.04613258400297,-1.04455478918545,-1.04291485363532,-1.0403799469425,
-1.03264335259191,-0.972209102718155,-0.936755982197143,-0.931198172772021,
-0.927700156260857,-0.924947062848449,-0.921871243726662,-0.91673198898983,
-0.896518852237591,-0.847203909213429,-0.813612938747056,-0.80980672060834,
-0.807866968120856,-0.806329010124019,-0.804506375433296,-0.801140024185952,
-0.782086953227113,-0.7194138822926,-0.697849080511699,-0.692443387723308,
-0.689277817977244,-0.686810427920725,-0.683565905870787,-0.677649478975064,
-0.642990322382811,-0.605936247558776,-0.57593027932295,-0.572142086953887,
-0.570206256676715,-0.568668623658462,-0.566843086458597,-0.563462785564301,
-0.544078610861073,-0.477568156956744,-0.459593297823505,-0.454443469971658,
-0.451365585110331,-0.448888570037038,-0.445530546847995,-0.439071812309515,
-0.43090289350318,-0.412224336496224,-0.366525912809479,-0.338241789697379,
-0.334476140865227,-0.332545215609742,-0.331007957512597,-0.329178697386759,
-0.325780537942659,-0.305960178196428,-0.233163971478154,-0.220633266136224,
-0.216127716266159,-0.213484673222681,-0.210824921190773,-0.207403423127645,
-0.203612346312103,-0.197391716207418,-0.184740905258884,-0.147886959461409,
-0.103415661649691,-0.097779673451371,-0.0954718481460404,-0.0938960488671336,
-0.0922544327903232,-0.0897104128021005,-0.0818950365296063,-0.0690642949045764,
-0.000705350955375777),.UNSPECIFIED.);
#795=B_SPLINE_CURVE_WITH_KNOTS('',3,(#93583,#93584,#93585,#93586),
 .UNSPECIFIED.,.F.,.F.,(4,4),(84.7497329240609,84.8230016469245),
 .UNSPECIFIED.);
#796=B_SPLINE_CURVE_WITH_KNOTS('',3,(#93587,#93588,#93589,#93590,#93591,
#93592,#93593,#93594,#93595,#93596,#93597,#93598,#93599,#93600,#93601,#93602,
#93603,#93604,#93605,#93606,#93607,#93608,#93609,#93610,#93611,#93612,#93613,
#93614,#93615,#93616,#93617,#93618,#93619,#93620,#93621,#93622,#93623,#93624,
#93625,#93626,#93627,#93628,#93629,#93630,#93631,#93632,#93633,#93634,#93635,
#93636,#93637,#93638,#93639,#93640,#93641,#93642,#93643,#93644,#93645,#93646,
#93647,#93648,#93649,#93650,#93651,#93652,#93653,#93654,#93655,#93656,#93657,
#93658,#93659,#93660,#93661,#93662,#93663,#93664,#93665,#93666,#93667,#93668,
#93669,#93670,#93671,#93672,#93673,#93674,#93675,#93676,#93677,#93678,#93679,
#93680,#93681,#93682,#93683,#93684,#93685,#93686,#93687,#93688,#93689,#93690,
#93691,#93692,#93693,#93694,#93695,#93696,#93697,#93698,#93699,#93700,#93701,
#93702,#93703,#93704,#93705,#93706,#93707,#93708,#93709,#93710,#93711,#93712,
#93713,#93714,#93715,#93716,#93717,#93718,#93719,#93720,#93721,#93722,#93723,
#93724,#93725,#93726,#93727,#93728,#93729,#93730,#93731,#93732,#93733,#93734,
#93735,#93736,#93737,#93738,#93739,#93740,#93741,#93742,#93743,#93744,#93745,
#93746,#93747,#93748,#93749,#93750,#93751,#93752,#93753,#93754,#93755,#93756,
#93757,#93758,#93759,#93760,#93761,#93762,#93763,#93764,#93765,#93766,#93767,
#93768,#93769,#93770,#93771,#93772,#93773,#93774,#93775,#93776,#93777,#93778,
#93779,#93780,#93781,#93782,#93783,#93784,#93785,#93786,#93787,#93788,#93789,
#93790,#93791,#93792,#93793,#93794,#93795,#93796,#93797,#93798,#93799,#93800,
#93801,#93802,#93803,#93804,#93805,#93806,#93807,#93808,#93809,#93810,#93811,
#93812,#93813,#93814,#93815,#93816,#93817,#93818,#93819,#93820,#93821,#93822,
#93823,#93824,#93825,#93826,#93827,#93828,#93829,#93830,#93831,#93832,#93833,
#93834,#93835,#93836,#93837,#93838,#93839,#93840,#93841,#93842,#93843,#93844,
#93845,#93846,#93847,#93848,#93849,#93850),.UNSPECIFIED.,.F.,.F.,(4,2,2,
2,2,2,2,2,2,2,2,2,2,2,2,2,2,2,2,2,2,2,2,2,2,2,2,2,2,2,2,2,2,2,2,2,2,2,2,
2,2,2,2,2,2,2,2,2,2,2,2,2,2,2,2,2,2,2,2,2,2,2,2,2,2,2,2,2,2,2,2,2,2,2,2,
2,2,2,2,2,2,2,2,2,2,2,2,2,2,2,2,2,2,2,2,2,2,2,2,2,2,2,2,2,2,2,2,2,2,2,2,
2,2,2,2,2,2,2,2,2,2,2,2,2,2,2,2,2,2,2,2,4),(-1.51256178469963,-1.4953817432681,
-1.46535641570292,-1.45992811232076,-1.4564444474865,-1.45365919909592,
-1.45050077899404,-1.44510791761768,-1.42207541070932,-1.36957684230411,
-1.36267082421071,-1.35641004918383,-1.34170042859708,-1.33841484557679,
-1.33657453571175,-1.33501434807961,-1.3330354266082,-1.32898545107136,
-1.29127028662996,-1.23149065413333,-1.22321474078269,-1.21951695137761,
-1.21669631745552,-1.21368076972235,-1.20893867372257,-1.19348024252329,
-1.16732946253917,-1.12913811357486,-1.11955262173962,-1.10435781900799,
-1.10133118596885,-1.09939116450975,-1.09783308113571,-1.09596108380582,
-1.09243364227792,-1.07003186219425,-1.03726284074255,-1.03190196364829,
-0.991095807270734,-0.985398563845544,-0.981833587765332,-0.979040130457728,
-0.975931558386187,-0.970765622093367,-0.95078099329336,-0.872785101731417,
-0.871473754818147,-0.865115003611904,-0.862668727943834,-0.861195405537403,
-0.859584236328339,-0.857259614993989,-0.851218106252388,-0.842221997512537,
-0.81280549440489,-0.790498037522222,-0.753492259344454,-0.747844048750969,
-0.744293294130027,-0.741500750710934,-0.738382591858399,-0.733175584503152,
-0.712690808936499,-0.673287236015255,-0.633265797060171,-0.627489416205511,
-0.62513897910371,-0.623538729324841,-0.621874973125982,-0.619300655158341,
-0.611419341087762,-0.598488306619038,-0.53405684292646,-0.514407857441494,
-0.50904044571588,-0.505887212577665,-0.503379310200202,-0.50001747919903,
-0.493677621999187,-0.440481135368036,-0.395548432556467,-0.389917987387191,
-0.387822553849985,-0.386335800273472,-0.384735660403504,-0.382469123737077,
-0.376801811462389,-0.347505372594177,-0.311465281050975,-0.278344199223827,
-0.272807362596115,-0.269290200071955,-0.266501105205479,-0.266442339248896,
-0.266388517754334,-0.266339221063827,-0.266294064907373,-0.266252697649597,
-0.266214797660163,-0.266180070843758,-0.266148248330416,-0.266119084328322,
-0.266092354150027,-0.266067852387372,-0.266045391233553,-0.266012309899606,
-0.265979852850944,-0.265948005557679,-0.265916753853183,-0.265886083937673,
-0.262574527655244,-0.256380438170859,-0.248574457770508,-0.231170514684446,
-0.195300185456222,-0.158348933954051,-0.152563782509416,-0.150211871480349,
-0.148611320401091,-0.146947943124938,-0.144375406430151,-0.136508874639095,
-0.12361184137463,-0.0646289259588138,-0.0460606698494302,-0.036728761200554,
-0.0330955323476834,-0.0304574657994303,-0.027793538976715,-0.0250426290603577,
-0.0214416168447533,-0.0182274268811936),.UNSPECIFIED.);
#797=B_SPLINE_CURVE_WITH_KNOTS('',3,(#93855,#93856,#93857,#93858,#93859,
#93860,#93861,#93862,#93863,#93864,#93865,#93866,#93867,#93868,#93869,#93870,
#93871,#93872,#93873,#93874,#93875,#93876,#93877,#93878,#93879,#93880,#93881,
#93882,#93883,#93884,#93885,#93886,#93887,#93888,#93889,#93890,#93891,#93892,
#93893,#93894,#93895,#93896,#93897,#93898,#93899,#93900,#93901,#93902,#93903,
#93904,#93905,#93906,#93907,#93908,#93909,#93910,#93911,#93912,#93913,#93914,
#93915,#93916,#93917,#93918,#93919,#93920,#93921,#93922,#93923,#93924,#93925,
#93926,#93927,#93928,#93929,#93930,#93931,#93932,#93933,#93934,#93935,#93936,
#93937,#93938,#93939,#93940,#93941,#93942,#93943,#93944,#93945,#93946,#93947,
#93948,#93949,#93950,#93951,#93952,#93953,#93954,#93955,#93956,#93957,#93958,
#93959,#93960,#93961,#93962,#93963,#93964,#93965,#93966,#93967,#93968,#93969,
#93970,#93971,#93972,#93973,#93974,#93975,#93976,#93977,#93978,#93979,#93980,
#93981,#93982,#93983,#93984,#93985,#93986,#93987,#93988,#93989,#93990,#93991,
#93992,#93993,#93994,#93995,#93996,#93997,#93998,#93999,#94000,#94001,#94002,
#94003,#94004,#94005,#94006,#94007,#94008,#94009,#94010,#94011,#94012,#94013,
#94014,#94015,#94016,#94017,#94018,#94019,#94020,#94021,#94022,#94023,#94024,
#94025,#94026,#94027,#94028,#94029,#94030,#94031,#94032,#94033,#94034,#94035,
#94036,#94037,#94038,#94039,#94040,#94041,#94042,#94043,#94044,#94045,#94046,
#94047,#94048,#94049,#94050,#94051,#94052,#94053,#94054,#94055,#94056,#94057,
#94058,#94059,#94060,#94061,#94062,#94063,#94064,#94065,#94066,#94067,#94068,
#94069,#94070,#94071,#94072,#94073,#94074,#94075,#94076,#94077,#94078,#94079,
#94080,#94081,#94082,#94083,#94084),.UNSPECIFIED.,.F.,.F.,(4,2,2,2,2,2,
2,2,2,2,2,2,2,2,2,2,2,2,2,2,2,2,2,2,2,2,2,2,2,2,2,2,2,2,2,2,2,2,2,2,2,2,
2,2,2,2,2,2,2,2,2,2,2,2,2,2,2,2,2,2,2,2,2,2,2,2,2,2,2,2,2,2,2,2,2,2,2,2,
2,2,2,2,2,2,2,2,2,2,2,2,2,2,2,2,2,2,2,2,2,2,2,2,2,2,2,2,2,2,2,2,2,2,2,2,
4),(-2.97297727746947,-2.95221453996876,-2.9494940641458,-2.94769156185505,
-2.94623135474866,-2.94469390590804,-2.94275495456382,-2.93895077642154,
-2.9066755594628,-2.881763692486,-2.85564790422669,-2.83590801533075,-2.83079210636194,
-2.82772192694603,-2.82496862466811,-2.8214631449971,-2.8158789431899,-2.77942483221904,
-2.77068148341162,-2.71942709430567,-2.7122162238443,-2.70979726981379,
-2.70815401062335,-2.70657928892087,-2.70427714976083,-2.69867549839649,
-2.65360976955837,-2.61719653010085,-2.60463310989038,-2.59558590040179,
-2.59174434251351,-2.58894101455537,-2.5863609378248,-2.58286049904218,
-2.57415209617595,-2.52602673949374,-2.49078452476213,-2.48085910621145,
-2.47437682572526,-2.4720073621897,-2.47040315865921,-2.46896621122825,
-2.46663829189167,-2.46088211357877,-2.42245226969945,-2.38810801114708,
-2.37057840747024,-2.35895178203451,-2.35471577562704,-2.35183599458596,
-2.34903301644091,-2.34566440704953,-2.3371925427222,-2.27958809703861,
-2.27150050523808,-2.24213650914775,-2.23649330888341,-2.23424946028425,
-2.23267007327095,-2.23120738031702,-2.22915346080045,-2.22369210998522,
-2.17565708943197,-2.12510574928066,-2.11886905131563,-2.11555716575829,
-2.11308488597496,-2.10997468268039,-2.10467735616917,-2.08529777665042,
-2.02030338340487,-2.0073609083736,-1.99949734144815,-1.99694720355168,
-1.99530405588822,-1.99372883869859,-1.99142504635005,-1.98581472900864,
-1.94076624125344,-1.90433757449402,-1.89177025856211,-1.88272057092448,
-1.87887823905397,-1.87607444769401,-1.8734940151019,-1.8699932015744,-1.86128442662558,
-1.81304130268261,-1.777880790207,-1.7679670708958,-1.76149019258386,-1.75912127302491,
-1.75751701095387,-1.75607968673327,-1.75375055499176,-1.74798837224119,
-1.71004500748069,-1.67471632238995,-1.65748424215765,-1.64600276498108,
-1.64178658252846,-1.63891057835832,-1.6361038118058,-1.63272161135779,
-1.624165837611,-1.56758444947759,-1.54283849185021,-1.52563434545013,-1.5223540419327,
-1.52054989904816,-1.51901030199244,-1.51704635046194,-1.51389570332999,
-1.49580382761679,-1.4782746125791),.UNSPECIFIED.);
#798=B_SPLINE_CURVE_WITH_KNOTS('',3,(#94086,#94087,#94088,#94089,#94090,
#94091),.UNSPECIFIED.,.F.,.F.,(4,2,4),(-0.0182274268811936,-0.0134492786994115,
-0.000702675572520198),.UNSPECIFIED.);
#799=B_SPLINE_CURVE_WITH_KNOTS('',3,(#94092,#94093,#94094,#94095,#94096,
#94097,#94098,#94099,#94100,#94101,#94102,#94103,#94104,#94105,#94106,#94107,
#94108,#94109,#94110,#94111,#94112,#94113,#94114,#94115,#94116,#94117,#94118,
#94119,#94120,#94121,#94122,#94123,#94124,#94125,#94126,#94127,#94128,#94129,
#94130,#94131,#94132,#94133,#94134,#94135,#94136,#94137,#94138,#94139,#94140,
#94141,#94142,#94143,#94144,#94145,#94146,#94147,#94148,#94149,#94150,#94151,
#94152,#94153,#94154,#94155,#94156,#94157,#94158,#94159,#94160,#94161,#94162,
#94163,#94164,#94165,#94166,#94167,#94168,#94169,#94170,#94171,#94172,#94173,
#94174,#94175,#94176,#94177,#94178,#94179,#94180,#94181,#94182,#94183,#94184,
#94185,#94186,#94187,#94188,#94189,#94190,#94191,#94192,#94193,#94194,#94195,
#94196,#94197,#94198,#94199,#94200,#94201,#94202,#94203,#94204,#94205,#94206,
#94207,#94208,#94209,#94210,#94211,#94212,#94213,#94214,#94215,#94216,#94217,
#94218,#94219,#94220,#94221,#94222,#94223,#94224,#94225,#94226,#94227,#94228,
#94229,#94230,#94231,#94232,#94233,#94234,#94235,#94236,#94237,#94238,#94239,
#94240,#94241,#94242,#94243,#94244,#94245,#94246,#94247,#94248,#94249,#94250,
#94251,#94252,#94253,#94254,#94255,#94256,#94257,#94258,#94259,#94260,#94261,
#94262,#94263,#94264,#94265,#94266,#94267,#94268,#94269,#94270,#94271,#94272,
#94273,#94274,#94275,#94276,#94277,#94278,#94279,#94280,#94281,#94282,#94283,
#94284,#94285,#94286,#94287,#94288,#94289,#94290,#94291,#94292,#94293,#94294,
#94295,#94296,#94297),.UNSPECIFIED.,.F.,.F.,(4,2,2,2,2,2,2,2,2,2,2,2,2,
2,2,2,2,2,2,2,2,2,2,2,2,2,2,2,2,2,2,2,2,2,2,2,2,2,2,2,2,2,2,2,2,2,2,2,2,
2,2,2,2,2,2,2,2,2,2,2,2,2,2,2,2,2,2,2,2,2,2,2,2,2,2,2,2,2,2,2,2,2,2,2,2,
2,2,2,2,2,2,2,2,2,2,2,2,2,2,2,2,2,4),(-2.98887565051434,-2.924502732387,
-2.9116084080508,-2.90374471214077,-2.90117315191559,-2.89951043355443,
-2.89791052968358,-2.89555960578578,-2.88977701208323,-2.85291143240863,
-2.82172016481015,-2.80142529955388,-2.79275082837876,-2.786023203112,-2.78259492680106,
-2.77991850353311,-2.7768063029024,-2.77162327817418,-2.75374583182232,
-2.687348427526,-2.67430110292321,-2.66637058556449,-2.66379067400412,-2.6621259570535,
-2.66052705313884,-2.65818211698718,-2.65243678498901,-2.61135467233543,
-2.57276607095971,-2.55252580314062,-2.54733906489724,-2.54422577895641,
-2.54143301420749,-2.53787569303257,-2.53220431057548,-2.48534630200705,
-2.45141203101676,-2.43063988579794,-2.42717072049725,-2.42531096040646,
-2.4237521232111,-2.42179740320996,-2.4179935483166,-2.38939056749786,-2.35564728515263,
-2.3296602452943,-2.31426483236396,-2.30952922856423,-2.30651487625532,
-2.30369330975633,-2.29999132504619,-2.29169328771963,-2.23206647392036,
-2.22579654900007,-2.19653850833415,-2.19087543859783,-2.18860973878453,
-2.18700990119698,-2.18552319164231,-2.18342751216897,-2.17779417307367,
-2.13312923248987,-2.07970556899923,-2.07338163539794,-2.07002333369528,
-2.06751596896705,-2.0643606712224,-2.05898294882711,-2.03921090304679,
-1.98169539181991,-1.95824977221685,-1.95317307697667,-1.95100443971885,
-1.94942137778761,-1.94769058250375,-1.94481271288965,-1.93517823272047,
-1.85988337229967,-1.84007745313684,-1.8349261213889,-1.83182072207062,
-1.82902654434142,-1.82545571894948,-1.81973905678311,-1.77608387858558,
-1.74630057633959,-1.7210332881551,-1.71576381880236,-1.71356264241937,
-1.71197442681424,-1.71025761566779,-1.70744187570374,-1.69834880242274,
-1.62245283417048,-1.60934495296105,-1.59997468515844,-1.59604744091723,
-1.59319929301744,-1.59058991356684,-1.58706744303955,-1.5783918062132,
-1.52724399612353,-1.51202174447739),.UNSPECIFIED.);
#800=B_SPLINE_CURVE_WITH_KNOTS('',3,(#94303,#94304,#94305,#94306,#94307,
#94308,#94309,#94310,#94311,#94312,#94313,#94314,#94315,#94316,#94317,#94318,
#94319,#94320,#94321,#94322,#94323,#94324,#94325,#94326,#94327,#94328,#94329,
#94330,#94331,#94332,#94333,#94334,#94335,#94336,#94337,#94338,#94339,#94340,
#94341,#94342,#94343,#94344,#94345,#94346,#94347,#94348,#94349,#94350,#94351,
#94352,#94353,#94354,#94355,#94356,#94357,#94358,#94359,#94360,#94361,#94362,
#94363,#94364,#94365,#94366,#94367,#94368,#94369,#94370,#94371,#94372,#94373,
#94374,#94375,#94376,#94377,#94378,#94379,#94380,#94381,#94382,#94383,#94384,
#94385,#94386,#94387,#94388,#94389,#94390,#94391,#94392,#94393,#94394,#94395,
#94396,#94397,#94398,#94399,#94400,#94401,#94402,#94403,#94404,#94405,#94406,
#94407,#94408,#94409,#94410,#94411,#94412,#94413,#94414,#94415,#94416,#94417,
#94418,#94419,#94420,#94421,#94422,#94423,#94424,#94425,#94426,#94427,#94428,
#94429,#94430,#94431,#94432,#94433,#94434,#94435,#94436,#94437,#94438,#94439,
#94440,#94441,#94442,#94443,#94444,#94445,#94446,#94447,#94448,#94449,#94450,
#94451,#94452,#94453,#94454,#94455,#94456,#94457,#94458,#94459,#94460,#94461,
#94462,#94463,#94464,#94465,#94466,#94467,#94468,#94469,#94470,#94471,#94472,
#94473,#94474,#94475,#94476,#94477,#94478,#94479,#94480,#94481,#94482,#94483,
#94484,#94485,#94486,#94487,#94488,#94489,#94490,#94491,#94492,#94493,#94494,
#94495,#94496,#94497,#94498,#94499,#94500,#94501,#94502,#94503,#94504,#94505,
#94506,#94507,#94508,#94509,#94510,#94511,#94512,#94513,#94514),
 .UNSPECIFIED.,.F.,.F.,(4,2,2,2,2,2,2,2,2,2,2,2,2,2,2,2,2,2,2,2,2,2,2,2,
2,2,2,2,2,2,2,2,2,2,2,2,2,2,2,2,2,2,2,2,2,2,2,2,2,2,2,2,2,2,2,2,2,2,2,2,
2,2,2,2,2,2,2,2,2,2,2,2,2,2,2,2,2,2,2,2,2,2,2,2,2,2,2,2,2,2,2,2,2,2,2,2,
2,2,2,2,2,2,2,2,2,4),(-1.47775839119131,-1.4611779278763,-1.41924546235713,
-1.38795686037687,-1.38415872913402,-1.38222151583026,-1.38068473641341,
-1.37886251446716,-1.37549436186771,-1.35635671360715,-1.29265286538653,
-1.27212884030762,-1.26680917396854,-1.26366473802928,-1.26092356717381,
-1.25753666538795,-1.25093058139933,-1.20594092436458,-1.15599682897976,
-1.15440641496971,-1.14789817105003,-1.14545039208858,-1.14399134575219,
-1.14241063578823,-1.14015623704611,-1.13444097310608,-1.12605307584872,
-1.06320357555216,-1.0354849517325,-1.03019731993654,-1.02678271786948,
-1.02403943531407,-1.02091467672117,-1.0155456064936,-0.9921090339615,-0.937125568051097,
-0.926871617136693,-0.912026020893665,-0.909049117047158,-0.907138680987286,
-0.905603173256661,-0.903758575493711,-0.90028502239137,-0.878417209564425,
-0.845194532079808,-0.798648930300137,-0.79303062573563,-0.789515714665283,
-0.786762431963749,-0.783699934362523,-0.778614880008762,-0.759041904507518,
-0.686483927225724,-0.674144929703243,-0.671065463761088,-0.66928760085356,
-0.667900154196183,-0.665982939097033,-0.662159274111292,-0.65717523893782,
-0.645295636299193,-0.594038544143118,-0.5608257336881,-0.555336689632327,
-0.551860436297277,-0.549110945961338,-0.546024982760459,-0.540834749594743,
-0.51993979883592,-0.478969588224529,-0.440842122753212,-0.43507618958467,
-0.432747112309301,-0.431310303621506,-0.429707082188517,-0.427340519604145,
-0.420875072259536,-0.410984444704404,-0.375956862431396,-0.327644102324335,
-0.318942327777471,-0.315443707571479,-0.312864664618153,-0.31006216422699,
-0.306221221296459,-0.297483189667764,-0.285305251943957,-0.221868465436772,
-0.217342998222484,-0.199726635508437,-0.196592772698569,-0.19463436611401,
-0.193095842780582,-0.191639337613152,-0.188903092060043,-0.178963690163551,
-0.160699276119067,-0.133760562345111,-0.0860423214136049,-0.0804145980755769,
-0.0768963544657262,-0.0741420414966949,-0.0710800240874364,-0.0659995859047076,
-0.0599518565472093,-0.000705108085373342),.UNSPECIFIED.);
#801=B_SPLINE_CURVE_WITH_KNOTS('',3,(#94515,#94516,#94517,#94518),
 .UNSPECIFIED.,.F.,.F.,(4,4),(-2.99015346847395,-2.97297727746947),
 .UNSPECIFIED.);
#802=B_SPLINE_CURVE_WITH_KNOTS('',3,(#94519,#94520,#94521,#94522,#94523,
#94524,#94525,#94526,#94527,#94528,#94529,#94530,#94531,#94532,#94533,#94534,
#94535,#94536,#94537,#94538,#94539,#94540,#94541,#94542,#94543,#94544,#94545,
#94546,#94547,#94548,#94549,#94550,#94551,#94552,#94553,#94554,#94555,#94556,
#94557,#94558,#94559,#94560,#94561,#94562,#94563,#94564,#94565,#94566,#94567,
#94568,#94569,#94570,#94571,#94572,#94573,#94574,#94575,#94576,#94577,#94578,
#94579,#94580,#94581,#94582,#94583,#94584,#94585,#94586,#94587,#94588,#94589,
#94590,#94591,#94592,#94593,#94594,#94595,#94596,#94597,#94598,#94599,#94600,
#94601,#94602,#94603,#94604,#94605,#94606,#94607,#94608,#94609,#94610,#94611,
#94612,#94613,#94614,#94615,#94616,#94617,#94618,#94619,#94620,#94621,#94622,
#94623,#94624,#94625,#94626,#94627,#94628,#94629,#94630,#94631,#94632,#94633,
#94634,#94635,#94636,#94637,#94638,#94639,#94640,#94641,#94642,#94643,#94644,
#94645,#94646,#94647,#94648,#94649,#94650,#94651,#94652,#94653,#94654,#94655,
#94656,#94657,#94658,#94659,#94660,#94661,#94662,#94663,#94664,#94665,#94666,
#94667,#94668,#94669,#94670,#94671,#94672,#94673,#94674,#94675,#94676,#94677,
#94678,#94679,#94680,#94681,#94682,#94683,#94684,#94685,#94686,#94687,#94688,
#94689,#94690,#94691,#94692,#94693,#94694,#94695,#94696,#94697,#94698,#94699,
#94700,#94701,#94702,#94703,#94704,#94705,#94706,#94707,#94708,#94709,#94710,
#94711,#94712,#94713,#94714,#94715,#94716,#94717,#94718,#94719,#94720,#94721,
#94722,#94723,#94724,#94725,#94726,#94727,#94728,#94729,#94730,#94731,#94732,
#94733,#94734,#94735,#94736,#94737,#94738,#94739,#94740,#94741,#94742,#94743,
#94744,#94745,#94746),.UNSPECIFIED.,.F.,.F.,(4,2,2,2,2,2,2,2,2,2,2,2,2,
2,2,2,2,2,2,2,2,2,2,2,2,2,2,2,2,2,2,2,2,2,2,2,2,2,2,2,2,2,2,2,2,2,2,2,2,
2,2,2,2,2,2,2,2,2,2,2,2,2,2,2,2,2,2,2,2,2,2,2,2,2,2,2,2,2,2,2,2,2,2,2,2,
2,2,2,2,2,2,2,2,2,2,2,2,2,2,2,2,2,2,2,2,2,2,2,2,2,2,2,2,4),(-1.51202174447739,
-1.49454904547617,-1.48047647626758,-1.47723513990231,-1.47540506904566,
-1.47384419879638,-1.47185238202793,-1.46773586712831,-1.42890611890207,
-1.37057961537579,-1.3621608425291,-1.35843811289281,-1.35561371845074,
-1.35260881984386,-1.34791412522944,-1.33288540212958,-1.30780132189531,
-1.26541787817727,-1.2610243371997,-1.24348457387812,-1.24033348088928,
-1.23835577300944,-1.23679598327268,-1.23495547551074,-1.23157518761894,
-1.212916632683,-1.15447851769646,-1.12903790133968,-1.12331786150973,-1.12005434928619,
-1.11755551154115,-1.11432301604353,-1.10858765767323,-1.0796058035442,
-1.04353236837729,-1.03032647780455,-1.02184158158486,-1.00598788047094,
-1.00292536993841,-1.00097462449748,-0.999416446127392,-0.997554476047233,
-0.994073212571871,-0.97295471418744,-0.939315910191897,-0.892652793814085,
-0.886965413263028,-0.883403850123935,-0.880611361153735,-0.87750210641738,
-0.872330885185528,-0.852270457105418,-0.772842320038168,-0.766649953058824,
-0.7642308084342,-0.762762865528405,-0.761147214997645,-0.758798621887785,
-0.752595231872824,-0.74327471609675,-0.711977772137954,-0.658973867250021,
-0.650371263336323,-0.646861015091463,-0.644254387368612,-0.64140309232168,
-0.63746021466311,-0.627997588604397,-0.614719458818356,-0.53878994188948,
-0.52991546547017,-0.527125223894997,-0.525413832246053,-0.523822707501726,
-0.521606177441953,-0.516246404653856,-0.490106156189358,-0.45024763806163,
-0.417348804721315,-0.411819486184611,-0.408304694585921,-0.405515957460026,
-0.402376289526936,-0.397071119966351,-0.37529378405299,-0.33121177996708,
-0.317697977874013,-0.30997757874266,-0.293670360335373,-0.290581576561852,
-0.288622337688618,-0.287063039614836,-0.285206446211447,-0.281973279058032,
-0.264981414398109,-0.21866767413947,-0.180202739992224,-0.174526968883625,
-0.170968009066002,-0.168174669778125,-0.165061479275423,-0.16184120849513,
-0.150894364641724,-0.119680003097134,-0.0931455658162746,-0.0915427925875306,
-0.057017804551295,-0.0531777008401065,-0.0512150774252604,-0.0496556400471943,
-0.0478019023790041,-0.0458209384900077,-0.0426901689906602,-0.0178547436485936),
 .UNSPECIFIED.);
#803=B_SPLINE_CURVE_WITH_KNOTS('',3,(#94751,#94752,#94753,#94754,#94755,
#94756,#94757,#94758,#94759,#94760,#94761,#94762,#94763,#94764,#94765,#94766,
#94767,#94768,#94769,#94770,#94771,#94772,#94773,#94774,#94775,#94776,#94777,
#94778,#94779,#94780,#94781,#94782,#94783,#94784,#94785,#94786,#94787,#94788,
#94789,#94790,#94791,#94792,#94793,#94794,#94795,#94796,#94797,#94798,#94799,
#94800,#94801,#94802,#94803,#94804,#94805,#94806,#94807,#94808,#94809,#94810,
#94811,#94812,#94813,#94814,#94815,#94816,#94817,#94818,#94819,#94820,#94821,
#94822,#94823,#94824,#94825,#94826,#94827,#94828,#94829,#94830,#94831,#94832,
#94833,#94834,#94835,#94836,#94837,#94838,#94839,#94840,#94841,#94842,#94843,
#94844,#94845,#94846,#94847,#94848,#94849,#94850,#94851,#94852,#94853,#94854,
#94855,#94856,#94857,#94858,#94859,#94860,#94861,#94862,#94863,#94864,#94865,
#94866,#94867,#94868,#94869,#94870,#94871,#94872,#94873,#94874,#94875,#94876,
#94877,#94878,#94879,#94880,#94881,#94882,#94883,#94884,#94885,#94886,#94887,
#94888,#94889,#94890,#94891,#94892,#94893,#94894,#94895,#94896,#94897,#94898,
#94899,#94900,#94901,#94902,#94903,#94904,#94905,#94906,#94907,#94908,#94909,
#94910,#94911,#94912,#94913,#94914,#94915,#94916,#94917,#94918,#94919,#94920,
#94921,#94922,#94923,#94924,#94925,#94926,#94927,#94928,#94929,#94930,#94931,
#94932,#94933,#94934,#94935,#94936,#94937,#94938,#94939,#94940,#94941,#94942,
#94943,#94944,#94945,#94946,#94947,#94948,#94949,#94950,#94951,#94952,#94953,
#94954,#94955,#94956,#94957,#94958,#94959,#94960,#94961,#94962,#94963,#94964,
#94965,#94966,#94967,#94968,#94969,#94970,#94971,#94972,#94973,#94974,#94975,
#94976,#94977,#94978),.UNSPECIFIED.,.F.,.F.,(4,2,2,2,2,2,2,2,2,2,2,2,2,
2,2,2,2,2,2,2,2,2,2,2,2,2,2,2,2,2,2,2,2,2,2,2,2,2,2,2,2,2,2,2,2,2,2,2,2,
2,2,2,2,2,2,2,2,2,2,2,2,2,2,2,2,2,2,2,2,2,2,2,2,2,2,2,2,2,2,2,2,2,2,2,2,
2,2,2,2,2,2,2,2,2,2,2,2,2,2,2,2,2,2,2,2,2,2,2,2,2,2,2,2,4),(-2.97195118185969,
-2.9369490547122,-2.93226175452182,-2.92910505028776,-2.92604856518349,
-2.92329348615702,-2.91976631159245,-2.91410805118695,-2.87171596726723,
-2.84438886087576,-2.81388158733176,-2.81200237225385,-2.80897499325155,
-2.80714019892494,-2.80560398575201,-2.80368154244454,-2.80066588080868,
-2.78516978194972,-2.78288127370539,-2.77840688596625,-2.71511747190682,
-2.70283392999893,-2.69400861379573,-2.69016861850486,-2.68736648366754,
-2.68478754184567,-2.68128869912165,-2.67258455885489,-2.62442157915607,
-2.58924068632587,-2.57932654774481,-2.57285044962834,-2.57048248913528,
-2.5688790775123,-2.5674426679379,-2.56511530173446,-2.55935890187728,-2.52133832720534,
-2.48032483337261,-2.45941782231408,-2.45422698257092,-2.45114101134447,
-2.44839173050279,-2.44491603522207,-2.43942840241542,-2.40626182341202,
-2.35492215363733,-2.34303259120955,-2.3380459607788,-2.33422100921978,
-2.33230358111693,-2.33091616954396,-2.32913859240383,-2.32606019634413,
-2.31373242493805,-2.24120266433382,-2.22163486114178,-2.21655023855645,
-2.21348780229,-2.21073444624916,-2.20721926499839,-2.20160011642017,-2.15499582423271,
-2.12166369863531,-2.09990151012898,-2.09643142233339,-2.094587532026,-2.09305195578115,
-2.09114061966151,-2.08816088627562,-2.07326734853567,-2.06315909275528,
-2.00813713993986,-1.98469587966175,-1.97932644762113,-1.97620152933803,
-1.9734581344623,-1.97004342940281,-1.96475566167598,-1.93705056922101,
-1.87420237739287,-1.86577185686649,-1.86003505377718,-1.85777716225911,
-1.85619569101364,-1.85473728171475,-1.85269776521772,-1.84734106505971,
-1.79758790832624,-1.74910404224857,-1.74260775703456,-1.73924307800478,
-1.73650306472142,-1.7333412604279,-1.72794682195026,-1.70650610604253,
-1.64943223513945,-1.63283852572199,-1.62658239155219,-1.62201633952051,
-1.61995631612376,-1.61840739531866,-1.61666560062987,-1.61366749514505,
-1.60262207004701,-1.53561223692235,-1.50985417869354,-1.50434232731809,
-1.5011862949276,-1.49844594424172,-1.49507404219208,-1.48854212004445,
-1.48025519169541,-1.47775839119131),.UNSPECIFIED.);
#804=B_SPLINE_CURVE_WITH_KNOTS('',3,(#94980,#94981,#94982,#94983),
 .UNSPECIFIED.,.F.,.F.,(4,4),(-0.0178547436485936,-0.00070312019684868),
 .UNSPECIFIED.);
#805=B_SPLINE_CURVE_WITH_KNOTS('',3,(#94984,#94985,#94986,#94987,#94988,
#94989,#94990,#94991,#94992,#94993,#94994,#94995,#94996,#94997,#94998,#94999,
#95000,#95001,#95002,#95003,#95004,#95005,#95006,#95007,#95008,#95009,#95010,
#95011,#95012,#95013,#95014,#95015,#95016,#95017,#95018,#95019,#95020,#95021,
#95022,#95023,#95024,#95025,#95026,#95027,#95028,#95029,#95030,#95031,#95032,
#95033,#95034,#95035,#95036,#95037,#95038,#95039,#95040,#95041,#95042,#95043,
#95044,#95045,#95046,#95047,#95048,#95049,#95050,#95051,#95052,#95053,#95054,
#95055,#95056,#95057,#95058,#95059,#95060,#95061,#95062,#95063,#95064,#95065,
#95066,#95067,#95068,#95069,#95070,#95071,#95072,#95073,#95074,#95075,#95076,
#95077,#95078,#95079,#95080,#95081,#95082,#95083,#95084,#95085,#95086,#95087,
#95088,#95089,#95090,#95091,#95092,#95093,#95094,#95095,#95096,#95097,#95098,
#95099,#95100,#95101,#95102,#95103,#95104,#95105,#95106,#95107,#95108,#95109,
#95110,#95111,#95112,#95113,#95114,#95115,#95116,#95117,#95118,#95119,#95120,
#95121,#95122,#95123,#95124,#95125,#95126,#95127,#95128,#95129,#95130,#95131,
#95132,#95133,#95134,#95135,#95136,#95137,#95138,#95139,#95140,#95141,#95142,
#95143,#95144,#95145,#95146,#95147,#95148,#95149,#95150,#95151,#95152,#95153,
#95154,#95155,#95156,#95157,#95158,#95159,#95160,#95161,#95162,#95163,#95164,
#95165,#95166,#95167,#95168,#95169,#95170,#95171,#95172,#95173,#95174,#95175,
#95176,#95177,#95178,#95179,#95180,#95181,#95182,#95183,#95184,#95185,#95186,
#95187,#95188,#95189,#95190,#95191,#95192,#95193,#95194,#95195,#95196,#95197),
 .UNSPECIFIED.,.F.,.F.,(4,2,2,2,2,2,2,2,2,2,2,2,2,2,2,2,2,2,2,2,2,2,2,2,
2,2,2,2,2,2,2,2,2,2,2,2,2,2,2,2,2,2,2,2,2,2,2,2,2,2,2,2,2,2,2,2,2,2,2,2,
2,2,2,2,2,2,2,2,2,2,2,2,2,2,2,2,2,2,2,2,2,2,2,2,2,2,2,2,2,2,2,2,2,2,2,2,
2,2,2,2,2,2,2,2,2,2,4),(-2.98816441937799,-2.94356845749968,-2.92995261709646,
-2.92561308819106,-2.92170371885123,-2.91886101117686,-2.91625140995095,
-2.91272072754498,-2.90398440736828,-2.85659656848203,-2.82107533596852,
-2.80612646805003,-2.8030567042658,-2.80122445450541,-2.79966564044199,
-2.7976814659872,-2.79450556971702,-2.77639981707171,-2.7258598640443,-2.70374524833081,
-2.69455564951707,-2.68755673914181,-2.68400531139556,-2.68121618627363,
-2.67810593514233,-2.67292183735761,-2.65499867934137,-2.59028462549177,
-2.56946381304208,-2.5659958438401,-2.56413762103748,-2.56258059896764,
-2.56062881791686,-2.55756019794813,-2.54156297305539,-2.53342368024984,
-2.478054108746,-2.45452058110026,-2.44909850677268,-2.44593588457654,-2.44315470177134,
-2.43968634307538,-2.43430155823529,-2.4052501969039,-2.35036330524257,
-2.33212389796571,-2.3287649428226,-2.32692997772095,-2.3253711725584,-2.32338997682959,
-2.32022444583021,-2.30234234717104,-2.28172950497194,-2.24463311279488,
-2.22688011892884,-2.21896889385078,-2.21265736295332,-2.20930391364666,
-2.20679943500284,-2.20364679990158,-2.19827121263619,-2.17847615589279,
-2.11426408838042,-2.1013527822919,-2.0934834627502,-2.09091248942569,-2.08925076484646,
-2.08765234661296,-2.08530442556419,-2.07953330766194,-2.04215632577042,
-2.00088836693657,-1.98701845046527,-1.97723724975104,-1.97324470036676,
-1.97038614143557,-1.96779227443219,-1.96367749198135,-1.95603375647796,
-1.89852665416244,-1.8621035047574,-1.8558259994071,-1.85346765045097,-1.85185100906884,
-1.85038660168186,-1.84837219642747,-1.84327982078029,-1.79085276816924,
-1.76496169687726,-1.74281978611869,-1.73749235527656,-1.73434993836325,
-1.73156515427559,-1.7280638975639,-1.72257261421912,-1.69069730093992,
-1.62708123617219,-1.61908060655544,-1.61649349393351,-1.61482803034779,
-1.61323174362351,-1.61089578481211,-1.60519811378123,-1.56236171378938,
-1.54229641354551,-1.51864233044459,-1.5126710689066),.UNSPECIFIED.);
#806=B_SPLINE_CURVE_WITH_KNOTS('',3,(#95203,#95204,#95205,#95206,#95207,
#95208,#95209,#95210,#95211,#95212,#95213,#95214,#95215,#95216,#95217,#95218,
#95219,#95220,#95221,#95222,#95223,#95224,#95225,#95226,#95227,#95228,#95229,
#95230,#95231,#95232,#95233,#95234,#95235,#95236,#95237,#95238,#95239,#95240,
#95241,#95242,#95243,#95244,#95245,#95246,#95247,#95248,#95249,#95250,#95251,
#95252,#95253,#95254,#95255,#95256,#95257,#95258,#95259,#95260,#95261,#95262,
#95263,#95264,#95265,#95266,#95267,#95268,#95269,#95270,#95271,#95272,#95273,
#95274,#95275,#95276,#95277,#95278,#95279,#95280,#95281,#95282,#95283,#95284,
#95285,#95286,#95287,#95288,#95289,#95290,#95291,#95292,#95293,#95294,#95295,
#95296,#95297,#95298,#95299,#95300,#95301,#95302,#95303,#95304,#95305,#95306,
#95307,#95308,#95309,#95310,#95311,#95312,#95313,#95314,#95315,#95316,#95317,
#95318,#95319,#95320,#95321,#95322,#95323,#95324,#95325,#95326,#95327,#95328,
#95329,#95330,#95331,#95332,#95333,#95334,#95335,#95336,#95337,#95338,#95339,
#95340,#95341,#95342,#95343,#95344,#95345,#95346,#95347,#95348,#95349,#95350,
#95351,#95352,#95353,#95354,#95355,#95356,#95357,#95358,#95359,#95360,#95361,
#95362,#95363,#95364,#95365,#95366,#95367,#95368,#95369,#95370,#95371,#95372,
#95373,#95374,#95375,#95376,#95377,#95378,#95379,#95380,#95381,#95382,#95383,
#95384,#95385,#95386,#95387,#95388,#95389,#95390,#95391,#95392,#95393,#95394,
#95395,#95396,#95397,#95398,#95399,#95400,#95401,#95402,#95403,#95404,#95405,
#95406,#95407,#95408,#95409,#95410),.UNSPECIFIED.,.F.,.F.,(4,2,2,2,2,2,
2,2,2,2,2,2,2,2,2,2,2,2,2,2,2,2,2,2,2,2,2,2,2,2,2,2,2,2,2,2,2,2,2,2,2,2,
2,2,2,2,2,2,2,2,2,2,2,2,2,2,2,2,2,2,2,2,2,2,2,2,2,2,2,2,2,2,2,2,2,2,2,2,
2,2,2,2,2,2,2,2,2,2,2,2,2,2,2,2,2,2,2,2,2,2,2,2,2,4),(-1.47746825606646,
-1.47709627062028,-1.47209694916288,-1.44909236909339,-1.39051927519349,
-1.37113071817875,-1.36583512835576,-1.36272662260841,-1.36025606675236,
-1.35694695811006,-1.35071707483464,-1.30060828375161,-1.25211572248421,
-1.24667659591132,-1.24462642346029,-1.24316532322844,-1.24158644242032,
-1.23934132486027,-1.23368453375267,-1.20415745200467,-1.15601140840689,
-1.13403220163634,-1.12859984754024,-1.12542958831988,-1.12269054298271,
-1.11933754787313,-1.11289693191768,-1.06253539433096,-1.01467415296095,
-1.00920915638578,-1.00715548421374,-1.00569338472111,-1.00411509121056,
-1.00187354789131,-0.996239986142577,-0.966964557799699,-0.957057943040063,
-0.901504238793805,-0.893067141873779,-0.889614134086156,-0.887046719413081,
-0.88423539516573,-0.880342970013861,-0.870982853562216,-0.857846035403174,
-0.780930925816261,-0.77252883090844,-0.769819827658108,-0.768142060505955,
-0.766570123362722,-0.764364736072971,-0.758958064051164,-0.697625271886426,
-0.660150085066973,-0.654543497433236,-0.65103175909567,-0.648278389114548,
-0.645213141002927,-0.640117271690002,-0.62042043620004,-0.546354932893747,
-0.535405917794819,-0.532416574712538,-0.530676412952253,-0.529126522577678,
-0.527061956296651,-0.522472915608532,-0.516177212879489,-0.499429108935249,
-0.441627794874962,-0.421031982487848,-0.415705145876597,-0.412558268467668,
-0.409816072336617,-0.406429323415642,-0.399828132120443,-0.35504187528113,
-0.329502828303619,-0.299292561881776,-0.295503193983947,-0.29356747120792,
-0.29203029848529,-0.290205750324685,-0.287039153145369,-0.27053520969566,
-0.226969864796906,-0.185050931584614,-0.179396039097259,-0.175869509344014,
-0.173114060955056,-0.170056271022691,-0.166897805205537,-0.156299319948201,
-0.127170685538684,-0.101402950954814,-0.0616978449188197,-0.0579506763742791,
-0.0560239940333789,-0.0544873128780441,-0.0526554164545771,-0.0506965542130373,
-0.0475960528900393,-0.0415486408128117,-0.00070472459549365),
 .UNSPECIFIED.);
#807=B_SPLINE_CURVE_WITH_KNOTS('',3,(#95411,#95412,#95413,#95414),
 .UNSPECIFIED.,.F.,.F.,(4,4),(-2.98953857001745,-2.97195118185969),
 .UNSPECIFIED.);
#808=B_SPLINE_CURVE_WITH_KNOTS('',3,(#95415,#95416,#95417,#95418,#95419,
#95420,#95421,#95422,#95423,#95424,#95425,#95426,#95427,#95428,#95429,#95430,
#95431,#95432,#95433,#95434,#95435,#95436,#95437,#95438,#95439,#95440,#95441,
#95442,#95443,#95444,#95445,#95446,#95447,#95448,#95449,#95450,#95451,#95452,
#95453,#95454,#95455,#95456,#95457,#95458,#95459,#95460,#95461,#95462,#95463,
#95464,#95465,#95466,#95467,#95468,#95469,#95470,#95471,#95472,#95473,#95474,
#95475,#95476,#95477,#95478,#95479,#95480,#95481,#95482,#95483,#95484,#95485,
#95486,#95487,#95488,#95489,#95490,#95491,#95492,#95493,#95494,#95495,#95496,
#95497,#95498,#95499,#95500,#95501,#95502,#95503,#95504,#95505,#95506,#95507,
#95508,#95509,#95510,#95511,#95512,#95513,#95514,#95515,#95516,#95517,#95518,
#95519,#95520,#95521,#95522,#95523,#95524,#95525,#95526,#95527,#95528,#95529,
#95530,#95531,#95532,#95533,#95534,#95535,#95536,#95537,#95538,#95539,#95540,
#95541,#95542,#95543,#95544,#95545,#95546,#95547,#95548,#95549,#95550,#95551,
#95552,#95553,#95554,#95555,#95556,#95557,#95558,#95559,#95560,#95561,#95562,
#95563,#95564,#95565,#95566,#95567,#95568,#95569,#95570,#95571,#95572,#95573,
#95574,#95575,#95576,#95577,#95578,#95579,#95580,#95581,#95582,#95583,#95584,
#95585,#95586,#95587,#95588,#95589,#95590,#95591,#95592,#95593,#95594,#95595,
#95596,#95597,#95598,#95599,#95600,#95601,#95602,#95603,#95604,#95605,#95606,
#95607,#95608,#95609,#95610,#95611,#95612,#95613,#95614,#95615,#95616,#95617,
#95618,#95619,#95620,#95621,#95622,#95623,#95624,#95625,#95626),
 .UNSPECIFIED.,.F.,.F.,(4,2,2,2,2,2,2,2,2,2,2,2,2,2,2,2,2,2,2,2,2,2,2,2,
2,2,2,2,2,2,2,2,2,2,2,2,2,2,2,2,2,2,2,2,2,2,2,2,2,2,2,2,2,2,2,2,2,2,2,2,
2,2,2,2,2,2,2,2,2,2,2,2,2,2,2,2,2,2,2,2,2,2,2,2,2,2,2,2,2,2,2,2,2,2,2,2,
2,2,2,2,2,2,2,2,2,4),(-1.5126710689066,-1.50902900777726,-1.50166488034743,
-1.49809872716826,-1.49530672181284,-1.49220220991738,-1.48704876977966,
-1.46718852130175,-1.39101341317623,-1.38216756132172,-1.37938191037392,
-1.37767227012861,-1.37608193812814,-1.37386531542221,-1.36849960589727,
-1.31047961773172,-1.2699440296854,-1.2642510525941,-1.26068822557359,-1.25789613057838,
-1.25478874285753,-1.24962399348292,-1.22963356587977,-1.15141395098973,
-1.14427581272797,-1.14171299607487,-1.14021747513831,-1.13862473547355,
-1.13639587950957,-1.13095769957971,-1.10402316342254,-1.07807015851243,
-1.03253510520935,-1.02683637259012,-1.02327131396667,-1.02047831652466,
-1.01737079676933,-1.01220788206989,-0.992251840888327,-0.914684047025733,
-0.906987746394055,-0.904347839999176,-0.902836811919838,-0.901252426853539,
-0.899074679307156,-0.893943939462053,-0.86999723419399,-0.809797496904229,
-0.792799560897511,-0.787708460028692,-0.784616337296652,-0.781819307729638,
-0.778224216072073,-0.770717423751258,-0.742093109111218,-0.69515724074363,
-0.687180457292685,-0.671025128574803,-0.667945051528449,-0.665988693212269,
-0.664429872060102,-0.662571692219192,-0.659109636481321,-0.638513782347949,
-0.604483258052994,-0.557618787560536,-0.551934980463562,-0.548374014816828,
-0.545580979119142,-0.542470067262867,-0.537293615108414,-0.517179730856772,
-0.444484243736937,-0.432939215277158,-0.429866574029808,-0.42809261411862,
-0.426679611725878,-0.424687958781014,-0.420574238647885,-0.415121977240386,
-0.35140648672764,-0.319705044798057,-0.314215513623113,-0.310712992975402,
-0.307925707943216,-0.304778878344555,-0.299440071282056,-0.277535166898882,
-0.230267609507277,-0.196858781148106,-0.193018486480805,-0.191055880367547,
-0.189496517683828,-0.188014097360527,-0.185240673862887,-0.174870888381879,
-0.155486013627489,-0.128300830884341,-0.0826822284841619,-0.0769900749504804,
-0.0734263033018798,-0.0706325653283003,-0.0675224178842369,-0.062350886356143,
-0.0561881268009385,-0.0182968368378989),.UNSPECIFIED.);
#809=B_SPLINE_CURVE_WITH_KNOTS('',3,(#95631,#95632,#95633,#95634,#95635,
#95636,#95637,#95638,#95639,#95640,#95641,#95642,#95643,#95644,#95645,#95646,
#95647,#95648,#95649,#95650,#95651,#95652,#95653,#95654,#95655,#95656,#95657,
#95658,#95659,#95660,#95661,#95662,#95663,#95664,#95665,#95666,#95667,#95668,
#95669,#95670,#95671,#95672,#95673,#95674,#95675,#95676,#95677,#95678,#95679,
#95680,#95681,#95682,#95683,#95684,#95685,#95686,#95687,#95688,#95689,#95690,
#95691,#95692,#95693,#95694,#95695,#95696,#95697,#95698,#95699,#95700,#95701,
#95702,#95703,#95704,#95705,#95706,#95707,#95708,#95709,#95710,#95711,#95712,
#95713,#95714,#95715,#95716,#95717,#95718,#95719,#95720,#95721,#95722,#95723,
#95724,#95725,#95726,#95727,#95728,#95729,#95730,#95731,#95732,#95733,#95734,
#95735,#95736,#95737,#95738,#95739,#95740,#95741,#95742,#95743,#95744,#95745,
#95746,#95747,#95748,#95749,#95750,#95751,#95752,#95753,#95754,#95755,#95756,
#95757,#95758,#95759,#95760,#95761,#95762,#95763,#95764,#95765,#95766,#95767,
#95768,#95769,#95770,#95771,#95772,#95773,#95774,#95775,#95776,#95777,#95778,
#95779,#95780,#95781,#95782,#95783,#95784,#95785,#95786,#95787,#95788,#95789,
#95790,#95791,#95792,#95793,#95794,#95795,#95796,#95797,#95798,#95799,#95800,
#95801,#95802,#95803,#95804,#95805,#95806,#95807,#95808,#95809,#95810,#95811,
#95812,#95813,#95814,#95815,#95816,#95817,#95818,#95819,#95820,#95821,#95822,
#95823,#95824,#95825,#95826,#95827,#95828,#95829,#95830,#95831,#95832,#95833,
#95834,#95835,#95836,#95837,#95838,#95839,#95840,#95841,#95842,#95843,#95844,
#95845,#95846,#95847,#95848,#95849,#95850,#95851,#95852,#95853,#95854,#95855,
#95856,#95857,#95858,#95859,#95860,#95861,#95862,#95863,#95864,#95865,#95866,
#95867,#95868,#95869,#95870,#95871,#95872,#95873,#95874,#95875,#95876,#95877,
#95878,#95879,#95880,#95881,#95882),.UNSPECIFIED.,.F.,.F.,(4,2,2,2,2,2,
2,2,2,2,2,2,2,2,2,2,2,2,2,2,2,2,2,2,2,2,2,2,2,2,2,2,2,2,2,2,2,2,2,2,2,2,
2,2,2,2,2,2,2,2,2,2,2,2,2,2,2,2,2,2,2,2,2,2,2,2,2,2,2,2,2,2,2,2,2,2,2,2,
2,2,2,2,2,2,2,2,2,2,2,2,2,2,2,2,2,2,2,2,2,2,2,2,2,2,2,2,2,2,2,2,2,2,2,2,
2,2,2,2,2,2,2,2,2,2,2,4),(-2.97105222820656,-2.92530151267993,-2.91538079316817,
-2.90890247926954,-2.90653503873986,-2.90493237564454,-2.90349693776976,
-2.90117170463306,-2.895423370209,-2.85808058991527,-2.82613219202151,-2.80650998840188,
-2.7980623344165,-2.79149927038503,-2.78813138876897,-2.78808881943302,
-2.78804466416076,-2.78799882046067,-2.78795117695518,-2.78790161241877,
-2.78784999467852,-2.78779617937313,-2.7877400085451,-2.78768130904727,
-2.78761989071349,-2.78758617227167,-2.78754414668624,-2.78749157245197,
-2.78742549492871,-2.78734195753053,-2.78723555921924,-2.78448544777219,
-2.78098941248966,-2.77543107034222,-2.74046848892012,-2.69085164613979,
-2.67336026453325,-2.67006853388269,-2.66826319041914,-2.66672570013493,
-2.66476845273363,-2.66163617456593,-2.64387132620129,-2.62275903217099,
-2.59396029863855,-2.55950270680088,-2.55359849283462,-2.55035866590881,
-2.54789394517402,-2.54473057676797,-2.53932562865379,-2.51771679613077,
-2.46082157020576,-2.44426799892404,-2.43802286764056,-2.43346348980179,
-2.43140522404205,-2.42985709387879,-2.42811560093025,-2.42511671889659,
-2.41405442068574,-2.36690267704485,-2.3225272142909,-2.31637118902119,
-2.31307801114676,-2.31036803877725,-2.30715908430598,-2.30155446291995,
-2.27707308805575,-2.21742480722635,-2.20484233231857,-2.19965751723748,
-2.19571402444066,-2.19377329846871,-2.19223673643475,-2.19041830635657,
-2.18715890214725,-2.17237776118083,-2.16209775319349,-2.1071384565206,
-2.08371233434017,-2.07834506624147,-2.07522121730192,-2.07247864731743,
-2.06906482003752,-2.06377812615093,-2.03606778559913,-1.97321740707834,
-1.96481064081507,-1.95908646828845,-1.95683096579821,-1.95525030031179,
-1.95379194259511,-1.95175156690936,-1.94638537858148,-1.89678922401156,
-1.84773390010898,-1.84151491598415,-1.83820832487275,-1.83573824803327,
-1.83262851463997,-1.82732628710088,-1.80785737019362,-1.74302629120196,
-1.73010072077122,-1.7222462694604,-1.719698500221,-1.71805673138258,-1.7164827103165,
-1.71418047346966,-1.70857297528363,-1.66375602990719,-1.61032566586255,
-1.6040541270702,-1.60073639625711,-1.59826510340564,-1.59516314800567,
-1.58989712492058,-1.57068800126628,-1.51200201039136,-1.49475244590984,
-1.48532634065609,-1.48249699836122,-1.48079283551505,-1.47923295084144,
-1.47746825606646),.UNSPECIFIED.);
#810=B_SPLINE_CURVE_WITH_KNOTS('',3,(#95884,#95885,#95886,#95887),
 .UNSPECIFIED.,.F.,.F.,(4,4),(-0.0182968368378989,-0.000703552307223293),
 .UNSPECIFIED.);
#811=B_SPLINE_CURVE_WITH_KNOTS('',3,(#95888,#95889,#95890,#95891,#95892,
#95893,#95894,#95895,#95896,#95897,#95898),.UNSPECIFIED.,.F.,.F.,(4,1,1,
1,1,1,1,1,4),(116.238928182822,116.441517666285,117.439865140746,118.438212615208,
119.43656008967,120.434907564131,121.433255038593,122.431602513054,122.449185868852),
 .UNSPECIFIED.);
#812=B_SPLINE_CURVE_WITH_KNOTS('',3,(#95904,#95905,#95906,#95907,#95908,
#95909,#95910,#95911,#95912,#95913,#95914,#95915,#95916,#95917,#95918,#95919,
#95920,#95921,#95922,#95923,#95924,#95925,#95926,#95927,#95928,#95929,#95930,
#95931,#95932,#95933,#95934,#95935,#95936,#95937,#95938,#95939,#95940,#95941,
#95942,#95943,#95944,#95945,#95946,#95947,#95948,#95949,#95950,#95951,#95952,
#95953,#95954,#95955,#95956,#95957,#95958,#95959,#95960,#95961,#95962,#95963,
#95964,#95965,#95966,#95967,#95968,#95969,#95970,#95971,#95972,#95973,#95974,
#95975,#95976,#95977,#95978,#95979,#95980,#95981,#95982,#95983,#95984,#95985,
#95986,#95987,#95988,#95989,#95990,#95991,#95992,#95993,#95994,#95995,#95996,
#95997,#95998,#95999,#96000,#96001,#96002,#96003,#96004,#96005,#96006,#96007,
#96008,#96009,#96010,#96011,#96012,#96013,#96014,#96015,#96016,#96017,#96018,
#96019,#96020,#96021,#96022,#96023,#96024,#96025,#96026,#96027,#96028,#96029,
#96030,#96031,#96032,#96033,#96034,#96035,#96036,#96037,#96038,#96039,#96040,
#96041,#96042,#96043,#96044,#96045,#96046,#96047,#96048,#96049,#96050,#96051,
#96052,#96053,#96054,#96055,#96056,#96057,#96058,#96059,#96060,#96061,#96062,
#96063,#96064,#96065,#96066,#96067,#96068,#96069,#96070,#96071,#96072,#96073,
#96074,#96075,#96076,#96077,#96078,#96079,#96080,#96081,#96082,#96083,#96084,
#96085,#96086,#96087,#96088,#96089,#96090,#96091,#96092,#96093,#96094,#96095,
#96096,#96097,#96098,#96099,#96100,#96101,#96102,#96103,#96104,#96105,#96106,
#96107,#96108,#96109,#96110,#96111,#96112,#96113,#96114,#96115,#96116,#96117,
#96118,#96119,#96120,#96121,#96122,#96123,#96124,#96125),.UNSPECIFIED.,
 .F.,.F.,(4,2,2,2,2,2,2,2,2,2,2,2,2,2,2,2,2,2,2,2,2,2,2,2,2,2,2,2,2,2,2,
2,2,2,2,2,2,2,2,2,2,2,2,2,2,2,2,2,2,2,2,2,2,2,2,2,2,2,2,2,2,2,2,2,2,2,2,
2,2,2,2,2,2,2,2,2,2,2,2,2,2,2,2,2,2,2,2,2,2,2,2,2,2,2,2,2,2,2,2,2,2,2,2,
2,2,2,2,2,2,2,4),(-1.47793342396516,-1.47159962187165,-1.4660379402415,
-1.46283796696356,-1.46012649238102,-1.45682034373151,-1.45060631668525,
-1.40225134133357,-1.3517649051731,-1.34646836074566,-1.34443704887868,
-1.34298079575677,-1.34139744942583,-1.33912990428269,-1.33333118643874,
-1.32478081060184,-1.26208573097235,-1.23446978938446,-1.22918575339998,
-1.22577204759006,-1.22302855875104,-1.21990256045232,-1.21452882960185,
-1.19102770864582,-1.13568054371755,-1.12673892458363,-1.11109250659368,
-1.10806886204215,-1.1061440343247,-1.10460777071771,-1.10277511142929,
-1.09935848510082,-1.07904394878322,-1.04475288864464,-0.997633447767629,
-0.992002901482155,-0.988484110867937,-0.985730120867635,-0.98266923504059,
-0.977592486795252,-0.958124846283896,-0.886799042433985,-0.873268274774364,
-0.870095825806595,-0.868296558952147,-0.866757232702543,-0.864788611259076,
-0.86070699330488,-0.822718483866519,-0.763169229744586,-0.754888630349755,
-0.751221024377858,-0.748436749114557,-0.74547328146437,-0.74084158770654,
-0.726017511987287,-0.701340221735429,-0.655861797813584,-0.636332726975957,
-0.633115482879547,-0.631132068715903,-0.629591542299174,-0.627802786050468,
-0.624591025500221,-0.608660404659928,-0.570595614235536,-0.522455439561844,
-0.516843548249632,-0.513330148149617,-0.510576502270404,-0.50751200621222,
-0.502419881557107,-0.482770413072307,-0.409315563165325,-0.397799365546918,
-0.394791582528596,-0.393029988137725,-0.391639678682922,-0.389698299193982,
-0.38575559746242,-0.380573540307272,-0.368005628469173,-0.30859069759747,
-0.300150886308403,-0.282757436445097,-0.277667586959828,-0.274603287024916,
-0.271922614699323,-0.268515172002092,-0.261724008637028,-0.252935447257296,
-0.232146904518091,-0.184801719550013,-0.177466924465691,-0.160884594063012,
-0.157809361891572,-0.155868567865602,-0.154331049681059,-0.15251042605993,
-0.149151659557329,-0.130252418459665,-0.0770446139636898,-0.0588631097972616,
-0.0445357484533284,-0.0397921013985291,-0.0368039172630358,-0.0341622528282387,
-0.0314694229747601,-0.027975389799477,-0.0183619817347547,-0.000704113525364955),
 .UNSPECIFIED.);
#813=B_SPLINE_CURVE_WITH_KNOTS('',3,(#96126,#96127,#96128,#96129),
 .UNSPECIFIED.,.F.,.F.,(4,4),(-2.9882406571501,-2.97105222820656),
 .UNSPECIFIED.);
#814=B_SPLINE_CURVE_WITH_KNOTS('',3,(#96131,#96132,#96133,#96134),
 .UNSPECIFIED.,.F.,.F.,(4,4),(122.449185868852,122.522113490002),
 .UNSPECIFIED.);
#815=B_SPLINE_CURVE_WITH_KNOTS('',3,(#96135,#96136,#96137,#96138,#96139,
#96140,#96141,#96142,#96143,#96144,#96145,#96146,#96147,#96148,#96149,#96150,
#96151,#96152,#96153,#96154,#96155,#96156,#96157,#96158,#96159,#96160,#96161,
#96162,#96163,#96164,#96165,#96166,#96167,#96168,#96169,#96170,#96171,#96172,
#96173,#96174,#96175,#96176,#96177,#96178,#96179,#96180,#96181,#96182,#96183,
#96184,#96185,#96186,#96187,#96188,#96189,#96190,#96191,#96192,#96193,#96194,
#96195,#96196,#96197,#96198,#96199,#96200,#96201,#96202,#96203,#96204,#96205,
#96206,#96207,#96208,#96209,#96210,#96211,#96212,#96213,#96214,#96215,#96216,
#96217,#96218,#96219,#96220,#96221,#96222,#96223,#96224,#96225,#96226,#96227,
#96228,#96229,#96230,#96231,#96232,#96233,#96234,#96235,#96236,#96237,#96238,
#96239,#96240,#96241,#96242,#96243,#96244,#96245,#96246,#96247,#96248,#96249,
#96250,#96251,#96252,#96253,#96254,#96255,#96256,#96257,#96258,#96259,#96260,
#96261,#96262,#96263,#96264,#96265,#96266,#96267,#96268,#96269,#96270,#96271,
#96272,#96273,#96274,#96275,#96276,#96277,#96278,#96279,#96280,#96281,#96282,
#96283,#96284,#96285,#96286,#96287,#96288,#96289,#96290,#96291,#96292,#96293,
#96294,#96295,#96296,#96297,#96298,#96299,#96300,#96301,#96302,#96303,#96304,
#96305,#96306,#96307,#96308,#96309,#96310,#96311,#96312,#96313,#96314,#96315,
#96316,#96317,#96318,#96319,#96320,#96321,#96322,#96323,#96324,#96325,#96326,
#96327,#96328,#96329,#96330,#96331,#96332,#96333,#96334,#96335,#96336,#96337,
#96338,#96339,#96340,#96341,#96342),.UNSPECIFIED.,.F.,.F.,(4,2,2,2,2,2,
2,2,2,2,2,2,2,2,2,2,2,2,2,2,2,2,2,2,2,2,2,2,2,2,2,2,2,2,2,2,2,2,2,2,2,2,
2,2,2,2,2,2,2,2,2,2,2,2,2,2,2,2,2,2,2,2,2,2,2,2,2,2,2,2,2,2,2,2,2,2,2,2,
2,2,2,2,2,2,2,2,2,2,2,2,2,2,2,2,2,2,2,2,2,2,2,2,2,4),(-2.99000648890043,
-2.94584961950891,-2.91750563332864,-2.90119728980008,-2.89636597661476,
-2.89333076978242,-2.89051718050843,-2.88686488964828,-2.87884288406013,
-2.81678963173155,-2.79147746640786,-2.78325120439183,-2.77938364032968,
-2.77631785259106,-2.77453625899897,-2.7730700105066,-2.7711114424974,-2.76728997175505,
-2.73168083212128,-2.6923351469078,-2.67446276990647,-2.66263866834934,
-2.65833929055804,-2.65541792140491,-2.65257523007425,-2.64915939487085,
-2.64056774525176,-2.58418313772043,-2.54359038310803,-2.53946696465267,
-2.53747338372987,-2.53591189421763,-2.53408197125094,-2.53084296728536,
-2.51681167995195,-2.50699989596687,-2.45109292763761,-2.42745022026519,
-2.42201598502322,-2.41884816587808,-2.41606355259808,-2.41259241123449,
-2.40720618384692,-2.3782511272735,-2.32316628647195,-2.30488778050943,
-2.30152378009873,-2.29968630137048,-2.29812550910223,-2.29614197743889,
-2.29297307131489,-2.27508243189597,-2.21442327651552,-2.19005460165781,
-2.18457358753396,-2.18139552271497,-2.17861205906584,-2.17515559611704,
-2.16981747173299,-2.14203608715072,-2.08582675482622,-2.06741264787652,
-2.06404231129803,-2.06220345234582,-2.06064275690239,-2.05866097050875,
-2.05549790390484,-2.03772978845781,-1.97211757853999,-1.95198234233895,
-1.94680360034088,-1.94369182908404,-1.94089834619067,-1.93733725691012,
-1.9316541003244,-1.88461847257711,-1.85095469856973,-1.83010275215818,
-1.82663020595846,-1.8247695891278,-1.82321059541139,-1.82125638604744,
-1.81818402684617,-1.80216924694576,-1.79719936234036,-1.79068417392659,
-1.75149391529011,-1.71605893443987,-1.71006050617056,-1.70677068307643,
-1.70426830902027,-1.70105674514441,-1.6955685016196,-1.6735170599907,-1.61155431797976,
-1.59252469258765,-1.58912650580283,-1.58728162235004,-1.58572136219572,
-1.58374719215495,-1.58060947530326,-1.56336042347625,-1.55920972524322,
-1.51274127243884),.UNSPECIFIED.);
#816=B_SPLINE_CURVE_WITH_KNOTS('',3,(#96347,#96348,#96349,#96350,#96351,
#96352,#96353,#96354,#96355,#96356,#96357,#96358,#96359,#96360,#96361,#96362,
#96363,#96364,#96365,#96366,#96367,#96368,#96369,#96370,#96371,#96372,#96373,
#96374,#96375,#96376,#96377,#96378,#96379,#96380,#96381,#96382,#96383,#96384,
#96385,#96386,#96387,#96388,#96389,#96390,#96391,#96392,#96393,#96394,#96395,
#96396,#96397,#96398,#96399,#96400,#96401,#96402,#96403,#96404,#96405,#96406,
#96407,#96408,#96409,#96410,#96411,#96412,#96413,#96414,#96415,#96416,#96417,
#96418,#96419,#96420,#96421,#96422,#96423,#96424,#96425,#96426,#96427,#96428,
#96429,#96430,#96431,#96432,#96433,#96434,#96435,#96436,#96437,#96438,#96439,
#96440,#96441,#96442,#96443,#96444,#96445,#96446,#96447,#96448,#96449,#96450,
#96451,#96452,#96453,#96454,#96455,#96456,#96457,#96458,#96459,#96460,#96461,
#96462,#96463,#96464,#96465,#96466,#96467,#96468,#96469,#96470,#96471,#96472,
#96473,#96474,#96475,#96476,#96477,#96478,#96479,#96480,#96481,#96482,#96483,
#96484,#96485,#96486,#96487,#96488,#96489,#96490,#96491,#96492,#96493,#96494,
#96495,#96496,#96497,#96498,#96499,#96500,#96501,#96502,#96503,#96504,#96505,
#96506,#96507,#96508,#96509,#96510,#96511,#96512,#96513,#96514,#96515,#96516,
#96517,#96518,#96519,#96520,#96521,#96522,#96523,#96524,#96525,#96526,#96527,
#96528,#96529,#96530,#96531,#96532,#96533,#96534,#96535,#96536,#96537,#96538,
#96539,#96540,#96541,#96542,#96543,#96544,#96545,#96546,#96547,#96548,#96549,
#96550,#96551,#96552,#96553,#96554),.UNSPECIFIED.,.F.,.F.,(4,2,2,2,2,2,
2,2,2,2,2,2,2,2,2,2,2,2,2,2,2,2,2,2,2,2,2,2,2,2,2,2,2,2,2,2,2,2,2,2,2,2,
2,2,2,2,2,2,2,2,2,2,2,2,2,2,2,2,2,2,2,2,2,2,2,2,2,2,2,2,2,2,2,2,2,2,2,2,
2,2,2,2,2,2,2,2,2,2,2,2,2,2,2,2,2,2,2,2,2,2,2,2,2,4),(-2.97245970569877,
-2.92214142952578,-2.90540104299264,-2.89416444720541,-2.88998453515166,
-2.88711724732677,-2.88430654192965,-2.88026812300541,-2.87071750805123,
-2.80991567029712,-2.80366616555044,-2.78370546701035,-2.77664279248751,
-2.77318320814191,-2.77040254914006,-2.76869567365967,-2.76720286901453,
-2.76521015750593,-2.76188911393139,-2.73917838155429,-2.68275001270377,
-2.65906925382898,-2.65368384135151,-2.65055523597599,-2.64781196009358,
-2.64440178348323,-2.63912940350878,-2.6118240669353,-2.54952293218338,
-2.53600628326957,-2.53294353728047,-2.53118739644393,-2.52964148803829,
-2.52764075755106,-2.52429249396449,-2.50091202790177,-2.44508431901798,
-2.42150249536741,-2.4161231738138,-2.41299573356251,-2.41025205980173,
-2.40683953559697,-2.40155998275564,-2.37408241569683,-2.31155847385648,
-2.30278117696173,-2.29686733692576,-2.2945818746975,-2.29299488471608,
-2.29154227326443,-2.28952533861236,-2.28432614855628,-2.23288302457447,
-2.18612792754243,-2.17946190520251,-2.17606221906702,-2.17331938318625,
-2.17018254612168,-2.1648984297429,-2.14485078258701,-2.08663205782153,
-2.06971086020924,-2.06337243880631,-2.05875974429205,-2.05669098805927,
-2.05514066800377,-2.05340299282845,-2.05042444804163,-2.03958378307114,
-1.96544366575285,-1.9524356509498,-1.94314461485686,-1.93926320064969,
-1.93645352673468,-1.93388328167895,-1.93041992631652,-1.92192473051514,
-1.86727322850476,-1.82452161311394,-1.82069813992169,-1.81878092520041,
-1.81739344515303,-1.81561547293187,-1.81253570679418,-1.80019351885902,
-1.72767259544492,-1.70810452157173,-1.70301961625593,-1.6999569720883,
-1.69720340524019,-1.69368792191613,-1.68806822370022,-1.64145632923907,
-1.60811179656522,-1.5863614245952,-1.58289154700259,-1.58104761784714,
-1.57951192243395,-1.57760032957371,-1.57462000213366,-1.55971912451465,
-1.5554069349699,-1.49544486761083,-1.47793342396516),.UNSPECIFIED.);
#817=B_SPLINE_CURVE_WITH_KNOTS('',3,(#96555,#96556,#96557,#96558,#96559,
#96560,#96561,#96562,#96563,#96564,#96565,#96566,#96567,#96568,#96569,#96570,
#96571,#96572,#96573,#96574,#96575,#96576,#96577,#96578,#96579,#96580,#96581,
#96582,#96583,#96584,#96585,#96586,#96587,#96588,#96589,#96590,#96591,#96592,
#96593,#96594,#96595,#96596,#96597,#96598,#96599,#96600,#96601,#96602,#96603,
#96604,#96605,#96606,#96607,#96608,#96609,#96610,#96611,#96612,#96613,#96614,
#96615,#96616,#96617,#96618,#96619,#96620,#96621,#96622,#96623,#96624,#96625,
#96626,#96627,#96628,#96629,#96630,#96631,#96632,#96633,#96634,#96635,#96636,
#96637,#96638,#96639,#96640,#96641,#96642,#96643,#96644,#96645,#96646,#96647,
#96648,#96649,#96650,#96651,#96652,#96653,#96654,#96655,#96656,#96657,#96658,
#96659,#96660,#96661,#96662,#96663,#96664,#96665,#96666,#96667,#96668,#96669,
#96670,#96671,#96672,#96673,#96674,#96675,#96676,#96677,#96678,#96679,#96680,
#96681,#96682,#96683,#96684,#96685,#96686,#96687,#96688,#96689,#96690,#96691,
#96692,#96693,#96694,#96695,#96696,#96697,#96698,#96699,#96700,#96701,#96702,
#96703,#96704,#96705,#96706,#96707,#96708,#96709,#96710,#96711,#96712,#96713,
#96714,#96715,#96716,#96717,#96718,#96719,#96720,#96721,#96722,#96723,#96724,
#96725,#96726,#96727,#96728,#96729,#96730,#96731,#96732,#96733,#96734,#96735,
#96736,#96737,#96738,#96739,#96740,#96741,#96742,#96743,#96744,#96745,#96746,
#96747,#96748,#96749,#96750,#96751,#96752,#96753,#96754,#96755,#96756,#96757,
#96758,#96759,#96760,#96761,#96762,#96763,#96764,#96765,#96766,#96767,#96768,
#96769,#96770,#96771,#96772,#96773,#96774,#96775,#96776,#96777,#96778,#96779,
#96780,#96781,#96782,#96783,#96784,#96785,#96786,#96787,#96788,#96789,#96790,
#96791,#96792,#96793,#96794,#96795,#96796,#96797,#96798,#96799,#96800,#96801,
#96802,#96803,#96804,#96805,#96806,#96807,#96808,#96809,#96810),
 .UNSPECIFIED.,.F.,.F.,(4,2,2,2,2,2,2,2,2,2,2,2,2,2,2,2,2,2,2,2,2,2,2,2,
2,2,2,2,2,2,2,2,2,2,2,2,2,2,2,2,2,2,2,2,2,2,2,2,2,2,2,2,2,2,2,2,2,2,2,2,
2,2,2,2,2,2,2,2,2,2,2,2,2,2,2,2,2,2,2,2,2,2,2,2,2,2,2,2,2,2,2,2,2,2,2,2,
2,2,2,2,2,2,2,2,2,2,2,2,2,2,2,2,2,2,2,2,2,2,2,2,2,2,2,2,2,2,2,4),(-1.51274127243884,
-1.49549398668246,-1.47715139789912,-1.47191936647955,-1.46879576988828,
-1.46628350754593,-1.46287932608243,-1.45633549067589,-1.40341849350104,
-1.35854339385021,-1.35291250969525,-1.35081696648587,-1.34933015024703,
-1.34772995972947,-1.34546337878145,-1.33979609649977,-1.3105010996305,
-1.30598427432574,-1.24433015989774,-1.23626162848646,-1.23260049860598,
-1.22978512106834,-1.22675293215949,-1.22193708368748,-1.20578588627485,
-1.17785593043212,-1.14521375320881,-1.13837746412902,-1.13192657775694,
-1.11740099292549,-1.11412732626893,-1.11228950905734,-1.11072876593191,
-1.10874572729469,-1.1046760509969,-1.06517436595889,-1.00750043041296,
-0.999127436817403,-0.995690764935652,-0.992842645836684,-0.989927835918512,
-0.985660663950069,-0.974068680490885,-0.956670052802494,-0.92081829779567,
-0.883849468738206,-0.878065502341966,-0.875713933138073,-0.874113567733765,
-0.872450337143972,-0.86987794744299,-0.862011242166212,-0.849113273710083,
-0.785210006884101,-0.765059982366121,-0.75965734035212,-0.75649657246078,
-0.753989847298627,-0.750638761412244,-0.744349423434949,-0.694626261157236,
-0.645892577052872,-0.640451299269309,-0.638381326364837,-0.636901453009344,
-0.635296153212917,-0.633001575103994,-0.627155225252009,-0.618543660064297,
-0.555722423090365,-0.528472500800093,-0.523156782458076,-0.519707287692145,
-0.516924525973986,-0.513741899032524,-0.508239375172271,-0.48352385291504,
-0.420214970398746,-0.405033773951311,-0.402007472732476,-0.40006729161317,
-0.398508819011127,-0.396636041380429,-0.393106278093656,-0.370656799772542,
-0.321193150647477,-0.291215968601058,-0.285788658773259,-0.282304906209567,
-0.279519121306193,-0.279467355042463,-0.279419976725557,-0.27937660280131,
-0.279336884477936,-0.27930050452084,-0.279267174318047,-0.279236631205406,
-0.279208636042033,-0.279182971010811,-0.279159437620457,-0.279137854908755,
-0.279104992352874,-0.279072745814695,-0.279041100108549,-0.279010040475174,
-0.278979552569855,-0.275673812187924,-0.269521690979313,-0.261771545500601,
-0.244546376309817,-0.203779465665771,-0.168494842914406,-0.164653168898947,
-0.162690190869913,-0.161130709281989,-0.159277199984235,-0.155838226582873,
-0.135837036075348,-0.0919629954157552,-0.0729435991846148,-0.0527102775772208,
-0.0472999482011549,-0.0441372506986406,-0.041630390480389,-0.0389781980499252,
-0.0356992516244263,-0.0307588796484749,-0.0182762009540131),
 .UNSPECIFIED.);
#818=B_SPLINE_CURVE_WITH_KNOTS('',3,(#96816,#96817,#96818,#96819,#96820,
#96821,#96822,#96823,#96824,#96825,#96826,#96827,#96828,#96829,#96830,#96831,
#96832,#96833,#96834,#96835,#96836,#96837,#96838,#96839,#96840,#96841,#96842,
#96843,#96844,#96845,#96846,#96847,#96848,#96849,#96850,#96851,#96852,#96853,
#96854,#96855,#96856,#96857,#96858,#96859,#96860,#96861,#96862,#96863,#96864,
#96865,#96866,#96867,#96868,#96869,#96870,#96871,#96872,#96873,#96874,#96875,
#96876,#96877,#96878,#96879,#96880,#96881,#96882,#96883,#96884,#96885,#96886,
#96887,#96888,#96889,#96890,#96891,#96892,#96893,#96894,#96895,#96896,#96897,
#96898,#96899,#96900,#96901,#96902,#96903,#96904,#96905,#96906,#96907,#96908,
#96909,#96910,#96911,#96912,#96913,#96914,#96915,#96916,#96917,#96918,#96919,
#96920,#96921,#96922,#96923,#96924,#96925,#96926,#96927,#96928,#96929,#96930,
#96931,#96932,#96933,#96934,#96935,#96936,#96937,#96938,#96939,#96940,#96941,
#96942,#96943,#96944,#96945,#96946,#96947,#96948,#96949,#96950,#96951,#96952,
#96953,#96954,#96955,#96956,#96957,#96958,#96959,#96960,#96961,#96962,#96963,
#96964,#96965,#96966,#96967,#96968,#96969,#96970,#96971,#96972,#96973,#96974,
#96975,#96976,#96977,#96978,#96979,#96980,#96981,#96982,#96983,#96984,#96985,
#96986,#96987,#96988,#96989,#96990,#96991,#96992,#96993,#96994,#96995,#96996,
#96997,#96998,#96999,#97000,#97001,#97002,#97003,#97004,#97005,#97006,#97007,
#97008,#97009,#97010,#97011,#97012,#97013,#97014,#97015,#97016,#97017,#97018,
#97019,#97020,#97021,#97022,#97023,#97024,#97025,#97026,#97027,#97028,#97029),
 .UNSPECIFIED.,.F.,.F.,(4,2,2,2,2,2,2,2,2,2,2,2,2,2,2,2,2,2,2,2,2,2,2,2,
2,2,2,2,2,2,2,2,2,2,2,2,2,2,2,2,2,2,2,2,2,2,2,2,2,2,2,2,2,2,2,2,2,2,2,2,
2,2,2,2,2,2,2,2,2,2,2,2,2,2,2,2,2,2,2,2,2,2,2,2,2,2,2,2,2,2,2,2,2,2,2,2,
2,2,2,2,2,2,2,2,2,2,4),(-1.47765371799144,-1.45142745756412,-1.44576112899101,
-1.44344851691512,-1.44187199792082,-1.4402321442346,-1.43769521092576,
-1.42993567632337,-1.3695627018735,-1.33412821553208,-1.32857313560911,
-1.32507682309873,-1.32232506213325,-1.31925072262929,-1.31411391864714,
-1.2939101260195,-1.24470366157367,-1.2110448045594,-1.20724049397964,-1.20530169388443,
-1.20376448058945,-1.20194271617302,-1.19857794039293,-1.17953286531276,
-1.11687703999204,-1.09533530595162,-1.0899331425105,-1.08676931348704,
-1.08430310269733,-1.08105991289151,-1.07514523528644,-1.04047048631585,
-1.00423675424185,-0.973490342597509,-0.969696136292642,-0.967759570096034,
-0.966222588323663,-0.964399282199045,-0.961026922533679,-0.94180090162142,
-0.877116019589753,-0.857518254725743,-0.852203753372913,-0.849090639811394,
-0.846619964327545,-0.843315226846412,-0.837108518188459,-0.78942467591477,
-0.738138697120928,-0.732920383228218,-0.730900565727312,-0.729447288336196,
-0.727861170436274,-0.725579644421702,-0.719690659690047,-0.710963148971715,
-0.648434678628104,-0.620936979259781,-0.6156573651419,-0.612244899571475,
-0.609501356501994,-0.606374155623114,-0.600995481362829,-0.577422260160876,
-0.521657765063854,-0.514091564330872,-0.497642949625792,-0.494575201808842,
-0.492636894586785,-0.491099827876407,-0.48927794940316,-0.485912213763665,
-0.466840042870094,-0.403880221409232,-0.38263106354139,-0.377255299656835,
-0.374097682196106,-0.371357191622453,-0.367986694848489,-0.361462530434708,
-0.307377819699041,-0.263615346754291,-0.25796110247614,-0.2556506714107,
-0.254074718260244,-0.252467481373426,-0.250015012302373,-0.247123966559145,
-0.241647450292063,-0.228023513600522,-0.193676029608931,-0.146529591470678,
-0.140899171299612,-0.137380330053458,-0.134626220580472,-0.131565119861788,
-0.126487822606833,-0.107015575728412,-0.0356453510311497,-0.0240297605022315,
-0.0196655814877161,-0.0176643188754654,-0.016163978162886,-0.0147204199484846,
-0.0129967245031383,-0.0104687631420757,-0.000704102697230447),
 .UNSPECIFIED.);
#819=B_SPLINE_CURVE_WITH_KNOTS('',3,(#97030,#97031,#97032,#97033),
 .UNSPECIFIED.,.F.,.F.,(4,4),(-2.98994510152635,-2.97245970569877),
 .UNSPECIFIED.);
#820=B_SPLINE_CURVE_WITH_KNOTS('',3,(#97035,#97036,#97037,#97038),
 .UNSPECIFIED.,.F.,.F.,(4,4),(-0.0182762009540131,-0.000702744675276971),
 .UNSPECIFIED.);
#821=B_SPLINE_CURVE_WITH_KNOTS('',3,(#97039,#97040,#97041,#97042,#97043,
#97044,#97045,#97046,#97047,#97048,#97049,#97050,#97051,#97052,#97053,#97054,
#97055,#97056,#97057,#97058,#97059,#97060,#97061,#97062,#97063,#97064,#97065,
#97066,#97067,#97068,#97069,#97070,#97071,#97072,#97073,#97074,#97075,#97076,
#97077,#97078,#97079,#97080,#97081,#97082,#97083,#97084,#97085,#97086,#97087,
#97088,#97089,#97090,#97091,#97092,#97093,#97094,#97095,#97096,#97097,#97098,
#97099,#97100,#97101,#97102,#97103,#97104,#97105,#97106,#97107,#97108,#97109,
#97110,#97111,#97112,#97113,#97114,#97115,#97116,#97117,#97118,#97119,#97120,
#97121,#97122,#97123,#97124,#97125,#97126,#97127,#97128,#97129,#97130,#97131,
#97132,#97133,#97134,#97135,#97136,#97137,#97138,#97139,#97140,#97141,#97142,
#97143,#97144,#97145,#97146,#97147,#97148,#97149,#97150,#97151,#97152,#97153,
#97154,#97155,#97156,#97157,#97158,#97159,#97160,#97161,#97162,#97163,#97164,
#97165,#97166,#97167,#97168,#97169,#97170,#97171,#97172,#97173,#97174,#97175,
#97176,#97177,#97178,#97179,#97180,#97181,#97182,#97183,#97184,#97185,#97186,
#97187,#97188,#97189,#97190,#97191,#97192,#97193,#97194,#97195,#97196,#97197,
#97198,#97199,#97200,#97201,#97202,#97203,#97204,#97205,#97206,#97207,#97208,
#97209,#97210,#97211,#97212,#97213,#97214,#97215,#97216,#97217,#97218,#97219,
#97220,#97221,#97222,#97223,#97224,#97225,#97226,#97227,#97228,#97229,#97230,
#97231,#97232,#97233,#97234,#97235,#97236,#97237,#97238,#97239,#97240,#97241,
#97242,#97243,#97244,#97245,#97246,#97247,#97248,#97249,#97250,#97251,#97252,
#97253,#97254,#97255,#97256),.UNSPECIFIED.,.F.,.F.,(4,2,2,2,2,2,2,2,2,2,
2,2,2,2,2,2,2,2,2,2,2,2,2,2,2,2,2,2,2,2,2,2,2,2,2,2,2,2,2,2,2,2,2,2,2,2,
2,2,2,2,2,2,2,2,2,2,2,2,2,2,2,2,2,2,2,2,2,2,2,2,2,2,2,2,2,2,2,2,2,2,2,2,
2,2,2,2,2,2,2,2,2,2,2,2,2,2,2,2,2,2,2,2,2,2,2,2,2,2,4),(-2.98990986834267,
-2.92589827377045,-2.91790264009375,-2.91531455028523,-2.91364780976403,
-2.912049745725,-2.90971033311418,-2.90399996945836,-2.86133972365879,-2.8358616406499,
-2.81552684940263,-2.80683975774228,-2.80012033891742,-2.79668688038249,
-2.79664121284996,-2.79659394193871,-2.79654496529467,-2.79649417193831,
-2.79644144135315,-2.79393060958563,-2.79079685546178,-2.7855190211026,
-2.76668177341165,-2.70130235832172,-2.68830972825382,-2.68040211965345,
-2.67782439675567,-2.67615976402111,-2.67455979966933,-2.67221154322354,
-2.66644925829432,-2.62561756680326,-2.58683368139395,-2.5665315003627,
-2.56133853346357,-2.55822317057154,-2.55542959105554,-2.5518726697505,
-2.54620482473542,-2.49937304034869,-2.46614000274728,-2.44463981483692,
-2.44114253579803,-2.43927640933814,-2.43771731915679,-2.43576866035675,
-2.43271528995482,-2.41705837521584,-2.40829076098589,-2.3491724791566,
-2.33585493713671,-2.32636910338221,-2.32242149275693,-2.31956851121527,
-2.31696152383361,-2.31345257279434,-2.30486215254651,-2.251435761258,-2.22037896474988,
-2.21109722379226,-2.20491304405002,-2.20256673849671,-2.20095109613951,
-2.19948193293225,-2.19705843365786,-2.1908426855805,-2.11143997697347,
-2.09137763858312,-2.08620460210324,-2.08309398493847,-2.08030009829476,
-2.07673651367095,-2.07104536623521,-2.02432779106774,-1.99062780407669,
-1.96952019868146,-1.96603786829361,-1.96417511781295,-1.96261615803266,
-1.96066428129978,-1.95687460803613,-1.92928588836175,-1.87727573845112,
-1.85433604069524,-1.84894877038702,-1.84579113836016,-1.84300507484848,
-1.83951839423567,-1.834081469451,-1.80386739892158,-1.74997563501545,-1.73184606268024,
-1.72848895140245,-1.72665290844792,-1.72509191096596,-1.72310629399625,
-1.71993061397123,-1.70190013653771,-1.68106279015895,-1.64414960195492,
-1.62643469254374,-1.61468657719638,-1.61039729347355,-1.6074776821537,
-1.60463278844666,-1.60120957906441,-1.59257343486644,-1.53678204388997,
-1.51273582755968),.UNSPECIFIED.);
#822=B_SPLINE_CURVE_WITH_KNOTS('',3,(#97261,#97262,#97263,#97264,#97265,
#97266,#97267,#97268,#97269,#97270,#97271,#97272,#97273,#97274,#97275,#97276,
#97277,#97278,#97279,#97280,#97281,#97282,#97283,#97284,#97285,#97286,#97287,
#97288,#97289,#97290,#97291,#97292,#97293,#97294,#97295,#97296,#97297,#97298,
#97299,#97300,#97301,#97302,#97303,#97304,#97305,#97306,#97307,#97308,#97309,
#97310,#97311,#97312,#97313,#97314,#97315,#97316,#97317,#97318,#97319,#97320,
#97321,#97322,#97323,#97324,#97325,#97326,#97327,#97328,#97329,#97330,#97331,
#97332,#97333,#97334,#97335,#97336,#97337,#97338,#97339,#97340,#97341,#97342,
#97343,#97344,#97345,#97346,#97347,#97348,#97349,#97350,#97351,#97352,#97353,
#97354,#97355,#97356,#97357,#97358,#97359,#97360,#97361,#97362,#97363,#97364,
#97365,#97366,#97367,#97368,#97369,#97370,#97371,#97372,#97373,#97374,#97375,
#97376,#97377,#97378,#97379,#97380,#97381,#97382,#97383,#97384,#97385,#97386,
#97387,#97388,#97389,#97390,#97391,#97392,#97393,#97394,#97395,#97396,#97397,
#97398,#97399,#97400,#97401,#97402,#97403,#97404,#97405,#97406,#97407,#97408,
#97409,#97410,#97411,#97412,#97413,#97414,#97415,#97416,#97417,#97418,#97419,
#97420,#97421,#97422,#97423,#97424,#97425,#97426,#97427,#97428,#97429,#97430,
#97431,#97432,#97433,#97434,#97435,#97436,#97437,#97438,#97439,#97440,#97441,
#97442,#97443,#97444,#97445,#97446,#97447,#97448,#97449,#97450,#97451,#97452,
#97453,#97454,#97455,#97456,#97457,#97458,#97459,#97460,#97461,#97462,#97463,
#97464,#97465,#97466),.UNSPECIFIED.,.F.,.F.,(4,2,2,2,2,2,2,2,2,2,2,2,2,
2,2,2,2,2,2,2,2,2,2,2,2,2,2,2,2,2,2,2,2,2,2,2,2,2,2,2,2,2,2,2,2,2,2,2,2,
2,2,2,2,2,2,2,2,2,2,2,2,2,2,2,2,2,2,2,2,2,2,2,2,2,2,2,2,2,2,2,2,2,2,2,2,
2,2,2,2,2,2,2,2,2,2,2,2,2,2,2,2,2,4),(-2.97176568216088,-2.96872105170352,
-2.95972050146067,-2.89185505033743,-2.87284393448954,-2.86948173076718,
-2.8676610454326,-2.86612454991605,-2.8641864205224,-2.86038272706146,-2.8249595191706,
-2.78535439701824,-2.76745110893685,-2.75564547704731,-2.75242182978618,
-2.74981077156188,-2.74712833812788,-2.7440165420145,-2.73865994653809,
-2.71713973115572,-2.65445810896365,-2.63541092860209,-2.63204685973361,
-2.63022564381836,-2.62868898578821,-2.6267510142312,-2.62294870739234,
-2.58913854524189,-2.57486177967326,-2.5222255774948,-2.51580519899522,
-2.51245648550289,-2.50971780318085,-2.5065444412584,-2.50109807983616,
-2.47891791216427,-2.41690490556003,-2.3979197705736,-2.39455816612544,
-2.39273738008213,-2.39120054274797,-2.38926165728933,-2.38619141726884,
-2.36968571550571,-2.36230251816553,-2.30649141213079,-2.28291548056584,
-2.27753738106449,-2.27441063358931,-2.27166755699529,-2.26825576168443,
-2.26297731000146,-2.23550445328324,-2.17299232357434,-2.16421886532137,
-2.15830728918988,-2.15602247394333,-2.15443585900521,-2.15298353266008,
-2.15096691627438,-2.14576808682149,-2.09434363735776,-2.04730393459202,
-2.04081535582008,-2.03745233306374,-2.03471251090759,-2.0315496360009,
-2.02615021759127,-2.00463924706465,-1.94192572650429,-1.92287261387068,
-1.91950771747663,-1.91768607683776,-1.91614907456029,-1.91421068658743,
-1.91040761448511,-1.87643881418507,-1.82759975911285,-1.80740297745391,
-1.80226719670048,-1.79919329988616,-1.79644182618105,-1.79294573042378,
-1.78739064478555,-1.75194577298051,-1.69157119874507,-1.68378982592072,
-1.68125031576849,-1.67960996578412,-1.67803396282162,-1.67572365929685,
-1.67007067408029,-1.62614751802524,-1.58896448683082,-1.57625022918979,
-1.56712029874236,-1.56326549549487,-1.56046041912332,-1.55788422801519,
-1.55439743863851,-1.5457342247264,-1.49481472321863,-1.47765371799144),
 .UNSPECIFIED.);
#823=B_SPLINE_CURVE_WITH_KNOTS('',3,(#97467,#97468,#97469,#97470,#97471,
#97472,#97473,#97474,#97475,#97476,#97477,#97478,#97479,#97480,#97481,#97482,
#97483,#97484,#97485,#97486,#97487,#97488,#97489,#97490,#97491,#97492,#97493,
#97494,#97495,#97496,#97497,#97498,#97499,#97500,#97501,#97502,#97503,#97504,
#97505,#97506,#97507,#97508,#97509,#97510,#97511,#97512,#97513,#97514,#97515,
#97516,#97517,#97518,#97519,#97520,#97521,#97522,#97523,#97524,#97525,#97526,
#97527,#97528,#97529,#97530,#97531,#97532,#97533,#97534,#97535,#97536,#97537,
#97538,#97539,#97540,#97541,#97542,#97543,#97544,#97545,#97546,#97547,#97548,
#97549,#97550,#97551,#97552,#97553,#97554,#97555,#97556,#97557,#97558,#97559,
#97560,#97561,#97562,#97563,#97564,#97565,#97566,#97567,#97568,#97569,#97570,
#97571,#97572,#97573,#97574,#97575,#97576,#97577,#97578,#97579,#97580,#97581,
#97582,#97583,#97584,#97585,#97586,#97587,#97588,#97589,#97590,#97591,#97592,
#97593,#97594,#97595,#97596,#97597,#97598,#97599,#97600,#97601,#97602,#97603,
#97604,#97605,#97606,#97607,#97608,#97609,#97610,#97611,#97612,#97613,#97614,
#97615,#97616,#97617,#97618,#97619,#97620,#97621,#97622,#97623,#97624,#97625,
#97626,#97627,#97628,#97629,#97630,#97631,#97632,#97633,#97634,#97635,#97636,
#97637,#97638,#97639,#97640,#97641,#97642,#97643,#97644,#97645,#97646,#97647,
#97648,#97649,#97650,#97651,#97652,#97653,#97654,#97655,#97656,#97657,#97658,
#97659,#97660,#97661,#97662,#97663,#97664,#97665,#97666,#97667,#97668,#97669,
#97670,#97671,#97672,#97673,#97674,#97675,#97676,#97677,#97678,#97679,#97680,
#97681,#97682),.UNSPECIFIED.,.F.,.F.,(4,2,2,2,2,2,2,2,2,2,2,2,2,2,2,2,2,
2,2,2,2,2,2,2,2,2,2,2,2,2,2,2,2,2,2,2,2,2,2,2,2,2,2,2,2,2,2,2,2,2,2,2,2,
2,2,2,2,2,2,2,2,2,2,2,2,2,2,2,2,2,2,2,2,2,2,2,2,2,2,2,2,2,2,2,2,2,2,2,2,
2,2,2,2,2,2,2,2,2,2,2,2,2,2,2,2,2,2,4),(-1.51273582755968,-1.49533009439322,
-1.49145300152984,-1.4894823103939,-1.48792216612365,-1.48607430729772,
-1.48266259777879,-1.46332313891588,-1.39785925583083,-1.37913500448887,
-1.37386797111017,-1.37073657882099,-1.36822537979251,-1.36483224077331,
-1.35834249433802,-1.30952180667387,-1.26014662303698,-1.25474526821147,
-1.25268042986114,-1.25120174885727,-1.24959493319984,-1.24729353762033,
-1.24140485726079,-1.2327108801626,-1.16995571829231,-1.14275634338727,
-1.13744191572076,-1.1339924830641,-1.13120926399711,-1.12802555896641,
-1.1225197558781,-1.09776291714441,-1.03413794464092,-1.01926034253567,
-1.01596275186856,-1.01411930237346,-1.01255872680346,-1.01058221077209,
-1.00654666027565,-1.0012266938936,-0.988236036753984,-0.922820106098911,
-0.904047660223555,-0.898775862710917,-0.895643321881228,-0.893132142281531,
-0.889740258144957,-0.883257099179764,-0.831450284803719,-0.785271298367369,
-0.779700350307255,-0.7776130450655,-0.776128337169116,-0.774526255956581,
-0.772250174779494,-0.766523891281055,-0.758146659589103,-0.702018719648352,
-0.668137691632259,-0.662577046371655,-0.659052510502516,-0.656262457136877,
-0.65312806524388,-0.647848197781125,-0.626420093698929,-0.581375938007835,
-0.577020946712195,-0.545132634245399,-0.541293187550638,-0.539330490903698,
-0.537770778091171,-0.53591645591085,-0.532474561284134,-0.512412442043688,
-0.435892584727484,-0.426414620254934,-0.422758399284,-0.420114404713707,
-0.417289066016605,-0.413500260763577,-0.404944110542066,-0.367919035203341,
-0.352959483710124,-0.310422040261175,-0.304706512188651,-0.302366261786151,
-0.300768059649106,-0.299101595237071,-0.296514683807388,-0.288747587277735,
-0.228300376322557,-0.19316411950662,-0.187566764711083,-0.184031504253709,
-0.181240831796681,-0.178113990707515,-0.173217453633384,-0.154668976338493,
-0.119786530530212,-0.0726714303882921,-0.0671620863195167,-0.0650831649812104,
-0.0636008725397968,-0.0619974234875304,-0.0597128594454045,-0.0571189548369731,
-0.0486132338801387,-0.0178597978295153),.UNSPECIFIED.);
#824=B_SPLINE_CURVE_WITH_KNOTS('',3,(#97688,#97689,#97690,#97691,#97692,
#97693,#97694,#97695,#97696,#97697,#97698,#97699,#97700,#97701,#97702,#97703,
#97704,#97705,#97706,#97707,#97708,#97709,#97710,#97711,#97712,#97713,#97714,
#97715,#97716,#97717,#97718,#97719,#97720,#97721,#97722,#97723,#97724,#97725,
#97726,#97727,#97728,#97729,#97730,#97731,#97732,#97733,#97734,#97735,#97736,
#97737,#97738,#97739,#97740,#97741,#97742,#97743,#97744,#97745,#97746,#97747,
#97748,#97749,#97750,#97751,#97752,#97753,#97754,#97755,#97756,#97757,#97758,
#97759,#97760,#97761,#97762,#97763,#97764,#97765,#97766,#97767,#97768,#97769,
#97770,#97771,#97772,#97773,#97774,#97775,#97776,#97777,#97778,#97779,#97780,
#97781,#97782,#97783,#97784,#97785,#97786,#97787,#97788,#97789,#97790,#97791,
#97792,#97793,#97794,#97795,#97796,#97797,#97798,#97799,#97800,#97801,#97802,
#97803,#97804,#97805,#97806,#97807,#97808,#97809,#97810,#97811,#97812,#97813,
#97814,#97815,#97816,#97817,#97818,#97819,#97820,#97821,#97822,#97823,#97824,
#97825,#97826,#97827,#97828,#97829,#97830,#97831,#97832,#97833,#97834,#97835,
#97836,#97837,#97838,#97839,#97840,#97841,#97842,#97843,#97844,#97845,#97846,
#97847,#97848,#97849,#97850,#97851,#97852,#97853,#97854,#97855,#97856,#97857,
#97858,#97859,#97860,#97861,#97862,#97863,#97864,#97865,#97866,#97867,#97868,
#97869,#97870,#97871,#97872,#97873,#97874,#97875,#97876,#97877,#97878,#97879,
#97880,#97881,#97882,#97883,#97884,#97885,#97886,#97887,#97888,#97889,#97890,
#97891,#97892,#97893,#97894,#97895,#97896,#97897,#97898,#97899,#97900,#97901,
#97902,#97903,#97904,#97905,#97906,#97907,#97908,#97909,#97910,#97911,#97912,
#97913,#97914,#97915,#97916,#97917,#97918,#97919,#97920,#97921),
 .UNSPECIFIED.,.F.,.F.,(4,2,2,2,2,2,2,2,2,2,2,2,2,2,2,2,2,2,2,2,2,2,2,2,
2,2,2,2,2,2,2,2,2,2,2,2,2,2,2,2,2,2,2,2,2,2,2,2,2,2,2,2,2,2,2,2,2,2,2,2,
2,2,2,2,2,2,2,2,2,2,2,2,2,2,2,2,2,2,2,2,2,2,2,2,2,2,2,2,2,2,2,2,2,2,2,2,
2,2,2,2,2,2,2,2,2,2,2,2,2,2,2,2,2,2,2,2,4),(-1.47803507761506,-1.4374382166583,
-1.42902327118118,-1.42566395721682,-1.42286355569726,-1.41998113674546,
-1.41573133860918,-1.40400284259666,-1.38626022836868,-1.34933916660219,
-1.32835208862582,-1.3102866655161,-1.30713792004883,-1.30517484722609,
-1.30363577175521,-1.30183205387249,-1.29855184675731,-1.28132977592769,
-1.25652702998621,-1.2001283038934,-1.1917446170029,-1.18830021066431,-1.18573435123345,
-1.18291997774264,-1.17901453134801,-1.16957959344572,-1.15630656989121,
-1.08170717121051,-1.07158472945669,-1.06867871926907,-1.06695688576749,
-1.06540167930469,-1.06330024680825,-1.05850693628611,-1.05184653958829,
-1.03361023354797,-0.969184367184311,-0.955827057811356,-0.95120815174358,
-0.948247057246169,-0.945460903105427,-0.941719724616904,-0.933253648008918,
-0.896613958422921,-0.853537293916598,-0.835069355832113,-0.83188894335215,
-0.829916348242102,-0.82837645503442,-0.826579441268595,-0.823330778887602,
-0.806728306024424,-0.762718975575585,-0.721312156487068,-0.715659828246629,
-0.712133841846288,-0.709378168350001,-0.706319462222812,-0.701255805482828,
-0.681960396031265,-0.644622824114802,-0.600836007622749,-0.595178876073316,
-0.592867515410677,-0.591291012797656,-0.589650367743824,-0.587110774356832,
-0.579331891156864,-0.518968595377029,-0.48352882298928,-0.477972731526719,
-0.474475768804785,-0.471723487626494,-0.468648558179329,-0.463510747875674,
-0.443302727661449,-0.394142336559927,-0.360421489890999,-0.356616502027983,
-0.354677346967185,-0.353139846597439,-0.351317735677201,-0.347952306769623,
-0.328903169174258,-0.266230682763259,-0.24469571757594,-0.239334067050411,
-0.236220014883805,-0.233740028253042,-0.233655368160887,-0.233587204057685,
-0.233530493093196,-0.233482156739802,-0.233360576876392,-0.233241224047959,
-0.233123063555533,-0.233005218496759,-0.23288692072389,-0.232767476824585,
-0.232646243675562,-0.23252261029551,-0.232395983961024,-0.232265779279798,
-0.228405497879208,-0.21866179705136,-0.169602741123395,-0.125606219698173,
-0.119951956199722,-0.117641164493793,-0.116064847083046,-0.114424174022154,
-0.11188419698253,-0.104101477988992,-0.0437464108273202,-0.00971125300947028,
-0.00384469650073024,-0.000705366426058919),.UNSPECIFIED.);
#825=B_SPLINE_CURVE_WITH_KNOTS('',3,(#97922,#97923,#97924,#97925,#97926,
#97927,#97928,#97929,#97930,#97931,#97932,#97933),.UNSPECIFIED.,.F.,.F.,
(4,2,2,2,2,4),(-2.9891191772697,-2.98772513884422,-2.98543450742337,-2.98285334584464,
-2.97881195257422,-2.97176568216088),.UNSPECIFIED.);
#826=B_SPLINE_CURVE_WITH_KNOTS('',3,(#97935,#97936,#97937,#97938),
 .UNSPECIFIED.,.F.,.F.,(4,4),(-0.0178597978295153,-0.000703565759050232),
 .UNSPECIFIED.);
#827=B_SPLINE_CURVE_WITH_KNOTS('',3,(#97939,#97940,#97941,#97942,#97943,
#97944,#97945,#97946,#97947,#97948,#97949,#97950,#97951,#97952,#97953,#97954,
#97955,#97956,#97957,#97958,#97959,#97960,#97961,#97962,#97963,#97964,#97965,
#97966,#97967,#97968,#97969,#97970,#97971,#97972,#97973,#97974,#97975,#97976,
#97977,#97978,#97979,#97980,#97981,#97982,#97983,#97984,#97985,#97986,#97987,
#97988,#97989,#97990,#97991,#97992,#97993,#97994,#97995,#97996,#97997,#97998,
#97999,#98000,#98001,#98002,#98003,#98004,#98005,#98006,#98007,#98008,#98009,
#98010,#98011,#98012,#98013,#98014,#98015,#98016,#98017,#98018,#98019,#98020,
#98021,#98022,#98023,#98024,#98025,#98026,#98027,#98028,#98029,#98030,#98031,
#98032,#98033,#98034,#98035,#98036,#98037,#98038,#98039,#98040,#98041,#98042,
#98043,#98044,#98045,#98046,#98047,#98048,#98049,#98050,#98051,#98052,#98053,
#98054,#98055,#98056,#98057,#98058,#98059,#98060,#98061,#98062,#98063,#98064,
#98065,#98066,#98067,#98068,#98069,#98070,#98071,#98072,#98073,#98074,#98075,
#98076,#98077,#98078,#98079,#98080,#98081,#98082,#98083,#98084,#98085,#98086,
#98087,#98088,#98089,#98090,#98091,#98092,#98093,#98094,#98095,#98096,#98097,
#98098,#98099,#98100,#98101,#98102,#98103,#98104,#98105,#98106,#98107,#98108,
#98109,#98110,#98111,#98112,#98113,#98114,#98115,#98116,#98117,#98118,#98119,
#98120,#98121,#98122,#98123,#98124,#98125,#98126,#98127,#98128,#98129,#98130,
#98131,#98132,#98133,#98134,#98135,#98136,#98137,#98138,#98139,#98140,#98141,
#98142,#98143,#98144,#98145,#98146,#98147,#98148),.UNSPECIFIED.,.F.,.F.,
(4,2,2,2,2,2,2,2,2,2,2,2,2,2,2,2,2,2,2,2,2,2,2,2,2,2,2,2,2,2,2,2,2,2,2,
2,2,2,2,2,2,2,2,2,2,2,2,2,2,2,2,2,2,2,2,2,2,2,2,2,2,2,2,2,2,2,2,2,2,2,2,
2,2,2,2,2,2,2,2,2,2,2,2,2,2,2,2,2,2,2,2,2,2,2,2,2,2,2,2,2,2,2,2,2,4),(-2.98869725023108,
-2.94478634572554,-2.93996525139911,-2.93673637914376,-2.93361763812439,
-2.93082743710486,-2.92728357025766,-2.92165410752704,-2.88528881974124,
-2.85699877390433,-2.82713274602364,-2.81861194066847,-2.81662066431204,
-2.81476000028187,-2.81320199906365,-2.81125033216377,-2.80745821492658,
-2.77956042165103,-2.72251147978083,-2.70432593050842,-2.69940406275812,
-2.6962962254929,-2.69350407822626,-2.68994166929962,-2.68425028701077,
-2.64408074789386,-2.59970276303459,-2.5825051973328,-2.57919547841962,
-2.57737042573491,-2.57580951260509,-2.57381206574106,-2.57059468046712,
-2.55172952614159,-2.53155636551345,-2.49501275335206,-2.47727105002767,
-2.46551208427408,-2.46122315176185,-2.45830503385862,-2.45546255770236,
-2.45204342034472,-2.44342394195459,-2.38751742307331,-2.37793658340261,
-2.34879338056555,-2.3431425529687,-2.34087948847909,-2.33928073111228,
-2.337587610471,-2.3348768564197,-2.32663681141175,-2.24978037870746,-2.22987711381173,
-2.22471964514284,-2.22161392193877,-2.2188215966232,-2.21525609684678,
-2.20955396767431,-2.16765007521875,-2.13857941870352,-2.11118390042684,
-2.10570135757225,-2.10346564575699,-2.10187204706687,-2.10016969644309,
-2.09741656709454,-2.08883686713255,-2.01239439569718,-1.99252056878035,
-1.98736607473593,-1.98426132086768,-1.9814693445828,-1.97790356908542,
-1.97219953347957,-1.92996558713754,-1.88690798812862,-1.87043773092777,
-1.86716667405698,-1.86535025335834,-1.8637887506722,-1.86178019927249,
-1.85852487050036,-1.83874640873644,-1.79775591495437,-1.76084327726368,
-1.75230337524243,-1.74851948686979,-1.74569692363156,-1.74305487433179,
-1.73940030820839,-1.72992048911928,-1.65344896115047,-1.63339647369863,
-1.62995710641481,-1.62810429239469,-1.62654592952984,-1.6245850490982,
-1.62074950432182,-1.58892893328139,-1.55838625006236,-1.53248072178885,
-1.51712033679016,-1.5123901083176,-1.51231102550938),.UNSPECIFIED.);
#828=B_SPLINE_CURVE_WITH_KNOTS('',3,(#98153,#98154,#98155,#98156,#98157,
#98158,#98159,#98160,#98161,#98162,#98163,#98164,#98165,#98166,#98167,#98168,
#98169,#98170,#98171,#98172,#98173,#98174,#98175,#98176,#98177,#98178,#98179,
#98180,#98181,#98182,#98183,#98184,#98185,#98186,#98187,#98188,#98189,#98190,
#98191,#98192,#98193,#98194,#98195,#98196,#98197,#98198,#98199,#98200,#98201,
#98202,#98203,#98204,#98205,#98206,#98207,#98208,#98209,#98210,#98211,#98212,
#98213,#98214,#98215,#98216,#98217,#98218,#98219,#98220,#98221,#98222,#98223,
#98224,#98225,#98226,#98227,#98228,#98229,#98230,#98231,#98232,#98233,#98234,
#98235,#98236,#98237,#98238,#98239,#98240,#98241,#98242,#98243,#98244,#98245,
#98246,#98247,#98248,#98249,#98250,#98251,#98252,#98253,#98254,#98255,#98256,
#98257,#98258,#98259,#98260,#98261,#98262,#98263,#98264,#98265,#98266,#98267,
#98268,#98269,#98270,#98271,#98272,#98273,#98274,#98275,#98276,#98277,#98278,
#98279,#98280,#98281,#98282,#98283,#98284,#98285,#98286,#98287,#98288,#98289,
#98290,#98291,#98292,#98293,#98294,#98295,#98296,#98297,#98298,#98299,#98300,
#98301,#98302,#98303,#98304,#98305,#98306,#98307,#98308,#98309,#98310,#98311,
#98312,#98313,#98314,#98315,#98316,#98317,#98318,#98319,#98320,#98321,#98322,
#98323,#98324,#98325,#98326,#98327,#98328,#98329,#98330,#98331,#98332,#98333,
#98334,#98335,#98336,#98337,#98338,#98339,#98340,#98341,#98342,#98343,#98344,
#98345,#98346,#98347,#98348,#98349,#98350,#98351,#98352,#98353,#98354,#98355,
#98356,#98357,#98358,#98359,#98360,#98361,#98362,#98363,#98364,#98365,#98366,
#98367,#98368,#98369,#98370,#98371,#98372,#98373,#98374,#98375,#98376,#98377,
#98378,#98379,#98380,#98381,#98382,#98383,#98384,#98385,#98386,#98387,#98388,
#98389,#98390,#98391,#98392,#98393,#98394,#98395,#98396,#98397,#98398,#98399,
#98400,#98401,#98402,#98403,#98404,#98405,#98406,#98407,#98408,#98409,#98410,
#98411,#98412,#98413,#98414,#98415,#98416,#98417,#98418,#98419,#98420,#98421,
#98422,#98423,#98424,#98425,#98426,#98427,#98428,#98429,#98430,#98431,#98432,
#98433,#98434,#98435,#98436,#98437,#98438,#98439,#98440,#98441,#98442,#98443,
#98444,#98445,#98446,#98447,#98448,#98449,#98450,#98451,#98452,#98453,#98454,
#98455,#98456,#98457,#98458),.UNSPECIFIED.,.F.,.F.,(4,2,2,2,2,2,2,2,2,2,
2,2,2,2,2,2,2,2,2,2,2,2,2,2,2,2,2,2,2,2,2,2,2,2,2,2,2,2,2,2,2,2,2,2,2,2,
2,2,2,2,2,2,2,2,2,2,2,2,2,2,2,2,2,2,2,2,2,2,2,2,2,2,2,2,2,2,2,2,2,2,2,2,
2,2,2,2,2,2,2,2,2,2,2,2,2,2,2,2,2,2,2,2,2,2,2,2,2,2,2,2,2,2,2,2,2,2,2,2,
2,2,2,2,2,2,2,2,2,2,2,2,2,2,2,2,2,2,2,2,2,2,2,2,2,2,2,2,2,2,2,2,2,2,4),
(-2.9723526798557,-2.97147367758802,-2.96947216547705,-2.96795877905284,
-2.96646860463858,-2.96474477447139,-2.96182936926877,-2.95161537306312,
-2.93951555371508,-2.87673067507901,-2.85699506679948,-2.8518879152199,
-2.84881533186768,-2.84605492998145,-2.84253348732493,-2.83690935729481,
-2.79041241366749,-2.7512981176478,-2.74054688101143,-2.73589267366465,
-2.73229897861837,-2.73044204480278,-2.73043710560119,-2.73043215127893,
-2.73042718173856,-2.73042219688213,-2.73041719664725,-2.73041218094353,
-2.73040714966964,-2.73040210274658,-2.73039704008575,-2.73039196158955,
-2.73038686716928,-2.7303817567387,-2.73037663021558,-2.73037148749642,
-2.73036641433062,-2.73036126587527,-2.73035604091821,-2.73035073820319,
-2.73034535647939,-2.73033989445168,-2.73033435080217,-2.73032872420341,
-2.73032301330493,-2.73031721671264,-2.73031133302377,-2.73030536080352,
-2.73029929859911,-2.7302931449125,-2.73028689823818,-2.73028055702682,
-2.73027411970475,-2.73026758468242,-2.73026095031405,-2.73025421494658,
-2.73024737690837,-2.73024043447437,-2.73023338588709,-2.73022622936283,
-2.73021896308281,-2.73021158520149,-2.730204093834,-2.73019648706117,-2.7301887629238,
-2.72873979435687,-2.7268035292362,-2.72301764881134,-2.69332078750982,
-2.64021484433467,-2.62005479049749,-2.61492071620485,-2.61184641371106,
-2.6090936652735,-2.60559469433469,-2.60003254616515,-2.56442148225037,
-2.50406726932473,-2.49632694258815,-2.49379287875546,-2.49215405179859,
-2.49057891793114,-2.48826758809657,-2.48260013316845,-2.43937872987733,
-2.40168845675221,-2.38229308990374,-2.37722558143666,-2.37416865470849,
-2.37141723149979,-2.36790038581627,-2.36227030904764,-2.31516642473108,
-2.28153888883397,-2.26048297906383,-2.25704058779779,-2.25520365962458,
-2.25366833314637,-2.25175074997344,-2.2480455406783,-2.22343732013175,
-2.18108013194337,-2.14941496686595,-2.14155074734815,-2.13791800614312,
-2.13514809809557,-2.13251089763286,-2.12803679210106,-2.11572883732265,
-2.04270739292887,-2.02287505417673,-2.01947542767887,-2.0176453950244,
-2.01610790732421,-2.0141770156478,-2.01041108729613,-1.98204701900106,
-1.92479075014335,-1.91297925358472,-1.90435293890396,-1.90058395495811,
-1.89779349219172,-1.89519678345639,-1.89162944270307,-1.88251996069581,
-1.81266254311245,-1.78796889419894,-1.78278779448989,-1.78061963283496,
-1.77905408186768,-1.77757188155018,-1.7750072647872,-1.76770119044484,
-1.72488378750006,-1.68850174997462,-1.67594545340269,-1.66690264559348,
-1.66306239326959,-1.66025982027577,-1.65768030369917,-1.65418042343413,
-1.64547240122963,-1.59743633690341,-1.56212688730419,-1.55219198877646,
-1.5457054738535,-1.54333576803615,-1.54173178298661,-1.54029511554569,
-1.53796820681521,-1.53221741670429,-1.49562193104974,-1.47803507761506),
 .UNSPECIFIED.);
#829=B_SPLINE_CURVE_WITH_KNOTS('',3,(#98459,#98460,#98461,#98462,#98463,
#98464,#98465,#98466,#98467,#98468,#98469,#98470,#98471,#98472,#98473,#98474,
#98475,#98476,#98477,#98478,#98479,#98480,#98481,#98482,#98483,#98484,#98485,
#98486,#98487,#98488,#98489,#98490,#98491,#98492,#98493,#98494,#98495,#98496,
#98497,#98498,#98499,#98500,#98501,#98502,#98503,#98504,#98505,#98506,#98507,
#98508,#98509,#98510,#98511,#98512,#98513,#98514,#98515,#98516,#98517,#98518,
#98519,#98520,#98521,#98522,#98523,#98524,#98525,#98526,#98527,#98528,#98529,
#98530,#98531,#98532,#98533,#98534,#98535,#98536,#98537,#98538,#98539,#98540,
#98541,#98542,#98543,#98544,#98545,#98546,#98547,#98548,#98549,#98550,#98551,
#98552,#98553,#98554,#98555,#98556,#98557,#98558,#98559,#98560,#98561,#98562,
#98563,#98564,#98565,#98566,#98567,#98568,#98569,#98570,#98571,#98572,#98573,
#98574,#98575,#98576,#98577,#98578,#98579,#98580,#98581,#98582,#98583,#98584,
#98585,#98586,#98587,#98588,#98589,#98590,#98591,#98592,#98593,#98594,#98595,
#98596,#98597,#98598,#98599,#98600,#98601,#98602,#98603,#98604,#98605,#98606,
#98607,#98608,#98609,#98610,#98611,#98612,#98613,#98614,#98615,#98616,#98617,
#98618,#98619,#98620,#98621,#98622,#98623,#98624,#98625,#98626,#98627,#98628,
#98629,#98630,#98631,#98632,#98633,#98634,#98635,#98636,#98637,#98638,#98639,
#98640,#98641,#98642,#98643,#98644,#98645,#98646,#98647,#98648,#98649,#98650,
#98651,#98652,#98653,#98654,#98655,#98656,#98657,#98658,#98659,#98660,#98661,
#98662,#98663,#98664,#98665,#98666,#98667,#98668,#98669,#98670,#98671,#98672,
#98673,#98674),.UNSPECIFIED.,.F.,.F.,(4,2,2,2,2,2,2,2,2,2,2,2,2,2,2,2,2,
2,2,2,2,2,2,2,2,2,2,2,2,2,2,2,2,2,2,2,2,2,2,2,2,2,2,2,2,2,2,2,2,2,2,2,2,
2,2,2,2,2,2,2,2,2,2,2,2,2,2,2,2,2,2,2,2,2,2,2,2,2,2,2,2,2,2,2,2,2,2,2,2,
2,2,2,2,2,2,2,2,2,2,2,2,2,2,2,2,2,2,4),(-1.51231102550938,-1.50937795378451,
-1.5065575892059,-1.5028559415549,-1.4948704996413,-1.46173491400937,-1.41883717248856,
-1.41381874968353,-1.39625132694891,-1.39309937667654,-1.39112162685282,
-1.38956208308337,-1.3877221529687,-1.38434387898383,-1.36572181637724,
-1.30758876903333,-1.28187577983948,-1.27664570300112,-1.27322342327221,
-1.27044385722297,-1.26724415740081,-1.26165858777699,-1.23550874200421,
-1.16433896777091,-1.15715537125209,-1.15458032033267,-1.15308240502432,
-1.15149145486357,-1.1492717954386,-1.14388803196606,-1.1174941258089,-1.11399542278392,
-1.06582504404247,-1.04399981113337,-1.03853007460249,-1.03532393679724,
-1.03254494112992,-1.02913122264479,-1.02253455089204,-1.01417128633876,
-0.99492975249179,-0.960975205301778,-0.941888522027811,-0.921800609081408,
-0.918532314651245,-0.916519650731639,-0.914957441929174,-0.913143056947562,
-0.909882772945706,-0.893621379949587,-0.854143268104672,-0.80806810645506,
-0.802376332445633,-0.798813489944883,-0.79602091190884,-0.792912501232409,
-0.787744906062139,-0.76772795930744,-0.689058446235256,-0.682276588338172,
-0.679766776138107,-0.678281276463881,-0.676679806042403,-0.674407929542478,
-0.668710084178113,-0.639088837451255,-0.590721339391454,-0.569242800693029,
-0.563800563178923,-0.560599182519575,-0.557817368010485,-0.554391296161003,
-0.547742215746839,-0.503284418711376,-0.454771575717138,-0.445576276743383,
-0.442748356083229,-0.441028689960377,-0.43944296094844,-0.437250912072291,
-0.432027220060372,-0.407182439707801,-0.356593571960495,-0.332167885948443,
-0.326514170286668,-0.323267244046988,-0.320519058481895,-0.31717151635646,
-0.310888269430139,-0.261295333244967,-0.212345008996586,-0.206966340545937,
-0.204906089468333,-0.203429754876905,-0.201953601928911,-0.19978898497157,
-0.194808303689184,-0.187706196878368,-0.167678666386733,-0.150885307902492,
-0.0995906345809307,-0.0909097994206186,-0.0873849550592839,-0.0847737139333753,
-0.081923428716779,-0.0779930536770725,-0.0686142555213277,-0.0182935576830915),
 .UNSPECIFIED.);
#830=B_SPLINE_CURVE_WITH_KNOTS('',3,(#98678,#98679,#98680,#98681,#98682,
#98683),.UNSPECIFIED.,.F.,.F.,(4,1,1,4),(-4.09293042013064,-3.99338989784634,
-2.99504242338476,-2.06901289643202),.UNSPECIFIED.);
#831=B_SPLINE_CURVE_WITH_KNOTS('',3,(#98687,#98688,#98689,#98690,#98691,
#98692,#98693,#98694,#98695,#98696,#98697,#98698,#98699,#98700,#98701,#98702,
#98703,#98704,#98705,#98706,#98707,#98708,#98709,#98710,#98711,#98712,#98713,
#98714,#98715,#98716,#98717,#98718,#98719,#98720,#98721,#98722,#98723),
 .UNSPECIFIED.,.F.,.F.,(4,3,3,3,3,3,3,3,3,3,3,3,4),(0.,0.0974621470036353,
0.194867321320676,0.295359620101813,0.39274979403887,0.490157456371112,
0.587604110657141,0.685111293680858,0.78276525835489,0.880505077811792,
0.978410992324384,0.998805711569776,1.11730040836826),.UNSPECIFIED.);
#832=B_SPLINE_CURVE_WITH_KNOTS('',3,(#98725,#98726,#98727,#98728,#98729,
#98730,#98731,#98732,#98733,#98734,#98735,#98736,#98737,#98738,#98739,#98740,
#98741,#98742,#98743,#98744,#98745,#98746,#98747,#98748,#98749,#98750,#98751,
#98752,#98753,#98754,#98755,#98756,#98757,#98758,#98759,#98760,#98761,#98762,
#98763,#98764,#98765,#98766,#98767,#98768,#98769,#98770,#98771,#98772,#98773,
#98774,#98775,#98776,#98777,#98778,#98779,#98780,#98781,#98782,#98783,#98784,
#98785,#98786,#98787,#98788,#98789,#98790,#98791,#98792,#98793,#98794,#98795,
#98796,#98797,#98798,#98799,#98800,#98801,#98802,#98803,#98804,#98805,#98806,
#98807,#98808,#98809,#98810,#98811,#98812,#98813,#98814,#98815,#98816,#98817,
#98818,#98819,#98820,#98821,#98822,#98823,#98824,#98825,#98826,#98827,#98828,
#98829,#98830,#98831,#98832,#98833,#98834,#98835,#98836,#98837,#98838,#98839,
#98840,#98841,#98842,#98843,#98844,#98845,#98846,#98847,#98848,#98849,#98850,
#98851,#98852,#98853,#98854,#98855,#98856,#98857,#98858,#98859,#98860,#98861,
#98862,#98863,#98864,#98865,#98866,#98867,#98868,#98869,#98870,#98871,#98872,
#98873,#98874,#98875,#98876,#98877,#98878,#98879,#98880,#98881,#98882,#98883,
#98884,#98885,#98886,#98887,#98888,#98889,#98890,#98891,#98892,#98893,#98894,
#98895,#98896,#98897,#98898,#98899,#98900,#98901,#98902,#98903,#98904,#98905,
#98906,#98907,#98908,#98909,#98910,#98911,#98912,#98913,#98914,#98915,#98916,
#98917,#98918,#98919,#98920,#98921,#98922,#98923,#98924,#98925,#98926,#98927,
#98928,#98929,#98930,#98931,#98932),.UNSPECIFIED.,.F.,.F.,(4,3,3,3,3,3,
3,3,3,3,3,3,3,3,3,3,3,3,3,3,3,3,3,3,3,3,3,3,3,3,3,3,3,3,3,3,3,3,3,3,3,3,
3,3,3,3,3,3,3,3,3,3,3,3,3,3,3,3,3,3,3,3,3,3,3,3,3,3,3,4),(1.11730040857369,
1.21026936232094,1.30311793855996,1.39587642027055,1.48858757671237,1.58127988763124,
1.67398180531496,1.76677948692346,1.85963092734075,1.9526328138594,1.99761142313956,
2.09298165155123,2.188220560694,2.28335751558291,2.37842514156716,2.47345765340052,
2.56848143150041,2.66352284114503,2.75866633648478,2.85386709030249,2.94921898643841,
2.99641713470934,3.09181289507372,3.1870804966658,3.28224925142725,3.37735319725211,
3.47242482594695,3.56749048050769,3.66257649114042,3.75776847975029,3.85302001444509,
3.94842577423536,3.99522284627912,4.09032351438071,4.18529104306171,4.28015519178503,
4.37494905104444,4.46970730681924,4.56445668469983,4.65922389510171,4.75409518218335,
4.84902445655776,4.94410867188475,4.9940285578489,5.08928497076329,5.18441006852906,
5.27943338437871,5.37438813325423,5.46930829119369,5.564220388636,5.65915094149034,
5.75418553061646,5.84927833113956,5.9445248238826,5.99283426941868,6.08808320371743,
6.18320112491135,6.27821757512862,6.37316595376636,6.4680800519387,6.56298640897521,
6.65791154995309,6.75294126289703,6.8480294847337,6.94327190966745,6.99163998098847,
7.09673724801162,7.20153978237807,7.30582428634004,7.4004855048612),
 .UNSPECIFIED.);
#833=B_SPLINE_CURVE_WITH_KNOTS('',3,(#98934,#98935,#98936,#98937,#98938,
#98939,#98940,#98941,#98942,#98943),.UNSPECIFIED.,.F.,.F.,(4,1,1,1,1,1,
1,4),(7.40048571554784,7.99044569255824,8.98925140412801,9.98805711569779,
10.9868628272676,11.9856685388373,12.9844742504071,13.6836710227274),
 .UNSPECIFIED.);
#834=B_SPLINE_CURVE_WITH_KNOTS('',3,(#98945,#98946,#98947,#98948,#98949,
#98950,#98951,#98952,#98953,#98954,#98955,#98956,#98957,#98958,#98959,#98960,
#98961,#98962,#98963,#98964,#98965,#98966,#98967,#98968,#98969,#98970,#98971,
#98972,#98973,#98974,#98975,#98976,#98977,#98978,#98979,#98980,#98981,#98982,
#98983,#98984,#98985,#98986,#98987,#98988,#98989,#98990,#98991,#98992,#98993,
#98994,#98995,#98996,#98997,#98998,#98999,#99000,#99001,#99002,#99003,#99004,
#99005,#99006,#99007,#99008,#99009,#99010,#99011,#99012,#99013,#99014,#99015,
#99016,#99017,#99018,#99019,#99020,#99021,#99022,#99023,#99024,#99025,#99026,
#99027,#99028,#99029,#99030,#99031,#99032,#99033,#99034,#99035,#99036,#99037,
#99038,#99039,#99040,#99041,#99042,#99043,#99044,#99045,#99046,#99047,#99048,
#99049,#99050,#99051,#99052,#99053,#99054,#99055,#99056,#99057,#99058,#99059,
#99060,#99061,#99062,#99063,#99064,#99065,#99066,#99067,#99068,#99069,#99070,
#99071,#99072,#99073,#99074,#99075,#99076,#99077,#99078,#99079,#99080,#99081,
#99082,#99083,#99084,#99085,#99086,#99087,#99088,#99089,#99090,#99091,#99092,
#99093,#99094,#99095,#99096,#99097,#99098,#99099,#99100,#99101,#99102,#99103,
#99104,#99105,#99106,#99107,#99108,#99109,#99110,#99111,#99112,#99113,#99114,
#99115,#99116,#99117,#99118,#99119,#99120,#99121,#99122,#99123,#99124,#99125,
#99126,#99127,#99128,#99129,#99130,#99131,#99132,#99133,#99134,#99135,#99136,
#99137,#99138,#99139,#99140,#99141,#99142,#99143,#99144,#99145,#99146,#99147,
#99148,#99149,#99150,#99151,#99152),.UNSPECIFIED.,.F.,.F.,(4,3,3,3,3,3,
3,3,3,3,3,3,3,3,3,3,3,3,3,3,3,3,3,3,3,3,3,3,3,3,3,3,3,3,3,3,3,3,3,3,3,3,
3,3,3,3,3,3,3,3,3,3,3,3,3,3,3,3,3,3,3,3,3,3,3,3,3,3,3,4),(13.6836712041916,
13.797991322231,13.9138835030568,13.9832799619769,14.0785092135632,14.1736070391483,
14.2686030110431,14.3635304257209,14.4584232661345,14.55330809716,14.6482114691976,
14.7432191749856,14.8382852213964,14.9335054242281,14.9820856735467,15.0773147893924,
15.1724124783643,15.2674083129692,15.3623355899308,15.4572282924156,15.5521129854716,
15.6470162196709,15.7420237886646,15.8370896986706,15.9323097670429,15.9808913851164,
16.0761204340477,16.1712180545898,16.2662138193526,16.3611410246546,16.4560336543772,
16.5509182736553,16.645821433147,16.7408289264676,16.8358947601386,16.9311147518851,
16.9796970966862,17.0749262208139,17.1700239176513,17.2650197596961,17.3599470434276,
17.4548397522635,17.5497244512421,17.6446276909254,17.7396352646988,17.834701179091,
17.9299212511898,17.978502808256,18.0737319081004,18.1688295804472,18.2638253978294,
18.3587526567462,18.4536453406822,18.5485300147066,18.6434332294124,18.7384407783249,
18.8335066678857,18.9287267154421,18.9773085198258,19.0723820620226,19.1673242839475,
19.2621649731371,19.3569377633092,19.4516766625256,19.5464084270052,19.6411597992607,
19.7360155760681,19.8309310201432,19.925997941627,19.966856329907),
 .UNSPECIFIED.);
#835=B_SPLINE_CURVE_WITH_KNOTS('',3,(#99154,#99155,#99156,#99157,#99158,
#99159,#99160,#99161,#99162,#99163,#99164,#99165),.UNSPECIFIED.,.F.,.F.,
(4,2,1,1,1,1,1,1,4),(19.966856329907,19.9761142313955,20.9749199429653,
21.9737256545351,22.9725313661049,23.9713370776747,24.9701427892444,25.9689485008142,
26.2500372664898),.UNSPECIFIED.);
#836=B_SPLINE_CURVE_WITH_KNOTS('',3,(#99167,#99168,#99169,#99170,#99171,
#99172,#99173,#99174,#99175,#99176,#99177,#99178,#99179,#99180,#99181,#99182,
#99183,#99184,#99185,#99186,#99187,#99188,#99189,#99190,#99191,#99192,#99193,
#99194,#99195,#99196,#99197,#99198,#99199,#99200,#99201,#99202,#99203,#99204,
#99205,#99206,#99207,#99208,#99209,#99210,#99211,#99212,#99213,#99214,#99215,
#99216,#99217,#99218,#99219,#99220,#99221,#99222,#99223,#99224,#99225,#99226,
#99227,#99228,#99229,#99230,#99231,#99232,#99233,#99234,#99235,#99236,#99237,
#99238,#99239,#99240,#99241,#99242,#99243,#99244,#99245,#99246,#99247,#99248,
#99249,#99250,#99251,#99252,#99253,#99254,#99255,#99256,#99257,#99258,#99259,
#99260,#99261,#99262,#99263,#99264,#99265,#99266,#99267,#99268,#99269,#99270,
#99271,#99272,#99273,#99274,#99275,#99276,#99277,#99278,#99279,#99280,#99281,
#99282,#99283,#99284,#99285,#99286,#99287,#99288,#99289,#99290,#99291,#99292,
#99293,#99294,#99295,#99296,#99297,#99298,#99299,#99300,#99301,#99302,#99303,
#99304,#99305,#99306,#99307,#99308,#99309,#99310,#99311,#99312,#99313,#99314,
#99315,#99316,#99317,#99318,#99319,#99320,#99321,#99322,#99323,#99324,#99325,
#99326,#99327,#99328,#99329,#99330,#99331,#99332,#99333,#99334,#99335,#99336,
#99337,#99338,#99339,#99340,#99341,#99342,#99343,#99344,#99345,#99346,#99347,
#99348,#99349,#99350,#99351,#99352,#99353,#99354,#99355,#99356,#99357,#99358,
#99359,#99360,#99361,#99362,#99363,#99364,#99365,#99366,#99367,#99368,#99369,
#99370,#99371,#99372,#99373,#99374),.UNSPECIFIED.,.F.,.F.,(4,3,3,3,3,3,
3,3,3,3,3,3,3,3,3,3,3,3,3,3,3,3,3,3,3,3,3,3,3,3,3,3,3,3,3,3,3,3,3,3,3,3,
3,3,3,3,3,3,3,3,3,3,3,3,3,3,3,3,3,3,3,3,3,3,3,3,3,3,3,4),(26.2500416370866,
26.3441968333611,26.4383096251651,26.5324074449842,26.6265177047687,26.7207282412848,
26.8149931960284,26.9094154392851,26.967754212384,27.0629833121013,27.1580809842519,
27.2530768013692,27.3480040599197,27.4428967434264,27.5377814169589,27.6326846311107,
27.7276921793768,27.8227580682378,27.9179781150178,27.9665599239538,28.0617890236771,
28.1568866958333,28.2518825129561,28.3468097715119,28.4417024550238,28.5365871285611,
28.6314903427171,28.7264978909876,28.8215637798526,28.9167838266362,28.9653656355235,
29.060594735272,29.155692407454,29.2506882246028,29.3456154831852,29.440508166724,
29.5353928402884,29.6302960544723,29.7253036027704,29.8203694916634,29.9155895384748,
29.9641713470933,30.0594004468259,30.1544981189915,30.2494939361243,30.3444211946902,
30.4393138782123,30.5341985517602,30.6291017659269,30.7241093142081,30.8191752030844,
30.914395249879,30.9629770586631,31.0582061583978,31.1533038305661,31.2482996477012,
31.3432269062693,31.4381195897934,31.5330042633433,31.6279074775115,31.7229150257946,
31.8179809146729,31.9132009614694,31.9617827702329,32.0592107277751,32.1564851134588,
32.253594530523,32.3506070134981,32.4475346235577,32.5332269442662),
 .UNSPECIFIED.);
#837=B_SPLINE_CURVE_WITH_KNOTS('',3,(#99376,#99377,#99378,#99379,#99380,
#99381,#99382,#99383,#99384,#99385),.UNSPECIFIED.,.F.,.F.,(4,1,1,1,1,1,
1,4),(32.5332323413119,32.9605884818027,33.9593941933724,34.9581999049422,
35.957005616512,36.9558113280818,37.9546170396515,38.8164122514458),
 .UNSPECIFIED.);
#838=B_SPLINE_CURVE_WITH_KNOTS('',3,(#99387,#99388,#99389,#99390,#99391,
#99392,#99393,#99394,#99395,#99396,#99397),.UNSPECIFIED.,.F.,.F.,(4,1,1,
1,1,1,1,1,4),(38.8164122514458,38.9534227512213,39.9522284627911,40.9510341743609,
41.9498398859306,42.9486455975004,43.9474513090702,44.94625702064,45.0995975586254),
 .UNSPECIFIED.);
#839=B_SPLINE_CURVE_WITH_KNOTS('',3,(#99399,#99400,#99401,#99402,#99403,
#99404,#99405,#99406,#99407,#99408),.UNSPECIFIED.,.F.,.F.,(4,1,1,1,1,1,
1,4),(45.0995975586254,45.9450627322098,46.9438684437795,47.9426741553493,
48.9414798669191,49.9402855784889,50.9390912900586,51.3827784970663),
 .UNSPECIFIED.);
#840=B_SPLINE_CURVE_WITH_KNOTS('',3,(#99410,#99411,#99412,#99413,#99414,
#99415,#99416,#99417,#99418,#99419,#99420,#99421,#99422,#99423,#99424,#99425,
#99426,#99427,#99428,#99429,#99430,#99431,#99432,#99433,#99434,#99435,#99436,
#99437,#99438,#99439,#99440,#99441,#99442,#99443,#99444,#99445,#99446,#99447,
#99448,#99449,#99450,#99451,#99452,#99453,#99454,#99455,#99456,#99457,#99458,
#99459,#99460,#99461,#99462,#99463,#99464,#99465,#99466,#99467,#99468,#99469,
#99470,#99471,#99472,#99473,#99474,#99475,#99476,#99477,#99478,#99479,#99480,
#99481,#99482,#99483,#99484,#99485,#99486,#99487,#99488,#99489,#99490,#99491,
#99492,#99493,#99494,#99495,#99496,#99497,#99498,#99499,#99500,#99501,#99502,
#99503,#99504,#99505,#99506,#99507,#99508,#99509,#99510,#99511,#99512,#99513,
#99514,#99515,#99516,#99517,#99518,#99519,#99520,#99521,#99522,#99523,#99524,
#99525,#99526,#99527,#99528,#99529,#99530,#99531,#99532,#99533,#99534,#99535,
#99536,#99537,#99538,#99539,#99540,#99541,#99542,#99543,#99544,#99545,#99546,
#99547,#99548,#99549,#99550,#99551,#99552,#99553,#99554,#99555,#99556,#99557,
#99558,#99559,#99560,#99561,#99562,#99563,#99564,#99565,#99566,#99567,#99568,
#99569,#99570,#99571,#99572,#99573,#99574,#99575,#99576,#99577,#99578,#99579,
#99580,#99581,#99582,#99583,#99584,#99585,#99586,#99587,#99588,#99589,#99590,
#99591,#99592,#99593,#99594,#99595,#99596,#99597,#99598,#99599,#99600,#99601,
#99602,#99603,#99604,#99605,#99606,#99607,#99608,#99609,#99610,#99611,#99612,
#99613,#99614,#99615,#99616,#99617),.UNSPECIFIED.,.F.,.F.,(4,3,3,3,3,3,
3,3,3,3,3,3,3,3,3,3,3,3,3,3,3,3,3,3,3,3,3,3,3,3,3,3,3,3,3,3,3,3,3,3,3,3,
3,3,3,3,3,3,3,3,3,3,3,3,3,3,3,3,3,3,3,3,3,3,3,3,3,3,3,4),(51.382782865805,
51.4801713722121,51.5776322272777,51.6752689470314,51.772999404316,51.8709376684413,
51.9378970016284,52.0331261013645,52.1282237735339,52.2232195906702,52.3181468492396,
52.4130395327654,52.5079242063168,52.6028274204872,52.6978349687721,52.7929008576518,
52.88812090445,52.9367027131982,53.0319318129343,53.1270294851035,53.2220253022398,
53.3169525608094,53.4118452443351,53.5067299178866,53.601633132057,53.6966406803419,
53.7917065692213,53.8869266160196,53.935508424768,54.0307375245042,54.1258351966735,
54.2208310138099,54.3157582723794,54.4106509559052,54.5055356294566,54.6004388436268,
54.6954463919116,54.7905122807912,54.8857323275893,54.9343141363377,55.0295432360737,
55.1246409082431,55.2196367253796,55.3145639839491,55.4094566674749,55.5043413410262,
55.5992445551964,55.6942521034812,55.7893179923608,55.884538039159,55.9331198479075,
56.0283489476435,56.1234466198129,56.2184424369491,56.3133696955187,56.4082623790445,
56.503147052596,56.5980502667659,56.6930578150508,56.7881237039302,56.8833437507283,
56.9319255594773,57.0261632540803,57.1202810694238,57.2143068149925,57.3082681983479,
57.4022166769982,57.4961537969889,57.5901558500571,57.6659681729846),
 .UNSPECIFIED.);
#841=B_SPLINE_CURVE_WITH_KNOTS('',3,(#99619,#99620,#99621,#99622,#99623,
#99624,#99625,#99626,#99627,#99628,#99629,#99630,#99631,#99632,#99633,#99634,
#99635,#99636,#99637,#99638,#99639,#99640,#99641,#99642,#99643,#99644,#99645,
#99646,#99647,#99648,#99649,#99650,#99651,#99652,#99653,#99654,#99655,#99656,
#99657,#99658,#99659,#99660,#99661,#99662,#99663,#99664,#99665,#99666,#99667,
#99668,#99669,#99670,#99671,#99672,#99673,#99674,#99675,#99676,#99677,#99678,
#99679,#99680,#99681,#99682,#99683,#99684,#99685,#99686,#99687,#99688,#99689,
#99690,#99691,#99692,#99693,#99694,#99695,#99696,#99697,#99698,#99699,#99700,
#99701,#99702,#99703,#99704,#99705,#99706,#99707,#99708,#99709,#99710,#99711,
#99712,#99713,#99714,#99715,#99716,#99717,#99718,#99719,#99720,#99721,#99722,
#99723,#99724,#99725,#99726,#99727,#99728,#99729,#99730,#99731,#99732,#99733,
#99734,#99735,#99736,#99737,#99738,#99739,#99740,#99741,#99742,#99743,#99744,
#99745,#99746,#99747,#99748,#99749,#99750,#99751,#99752,#99753,#99754,#99755,
#99756,#99757,#99758,#99759,#99760,#99761,#99762,#99763,#99764,#99765,#99766,
#99767,#99768,#99769,#99770,#99771,#99772,#99773,#99774,#99775,#99776,#99777,
#99778,#99779,#99780,#99781,#99782,#99783,#99784,#99785,#99786,#99787,#99788,
#99789,#99790,#99791,#99792,#99793,#99794,#99795,#99796,#99797,#99798,#99799,
#99800,#99801,#99802,#99803,#99804,#99805,#99806,#99807,#99808,#99809,#99810,
#99811,#99812,#99813,#99814,#99815,#99816,#99817,#99818,#99819,#99820,#99821,
#99822,#99823,#99824,#99825,#99826,#99827,#99828,#99829),.UNSPECIFIED.,
 .F.,.F.,(4,3,3,3,3,3,3,3,3,3,3,3,3,3,3,3,3,3,3,3,3,3,3,3,3,3,3,3,3,3,3,
3,3,3,3,3,3,3,3,3,3,3,3,3,3,3,3,3,3,3,3,3,3,3,3,3,3,3,3,3,3,3,3,3,3,3,3,
3,3,3,4),(57.6659681731688,57.7852696288089,57.9069205713756,57.9307312710471,
58.0259603707832,58.1210580429527,58.2160538600891,58.3109811186587,58.4058738021845,
58.500758475736,58.5956616899063,58.6906692381912,58.7857351270709,58.8809551738691,
58.9295369826169,59.024766082353,59.1198637545224,59.2148595716588,59.3097868302282,
59.404679513754,59.4995641873054,59.5944674014757,59.6894749497605,59.7845408386401,
59.8797608854383,59.9283426941866,60.0235717939227,60.1186694660922,60.2136652832285,
60.308592541798,60.4034852253238,60.4983698988752,60.5932731130455,60.6882806613303,
60.78334655021,60.8785665970082,60.9271484057564,61.0223775054925,61.1174751776619,
61.2124709947983,61.3073982533678,61.4022909368936,61.497175610445,61.5920788246154,
61.6870863729002,61.7821522617799,61.8773723085781,61.9259541173262,62.0211832170623,
62.1162808892317,62.211276706368,62.3062039649375,62.4010966484633,62.4959813220147,
62.5908845361849,62.6858920844697,62.7809579733493,62.8761780201476,62.924759828896,
63.0199889286321,63.1150866008014,63.2100824179378,63.3050096765074,63.3999023600331,
63.4947870335845,63.5896902477548,63.6846977960397,63.7797636849193,63.8749837317175,
63.9235655404658,63.9491534801642),.UNSPECIFIED.);
#842=B_SPLINE_CURVE_WITH_KNOTS('',3,(#99831,#99832,#99833,#99834,#99835,
#99836,#99837,#99838,#99839,#99840,#99841,#99842,#99843,#99844,#99845,#99846,
#99847,#99848,#99849,#99850,#99851,#99852,#99853,#99854,#99855,#99856,#99857,
#99858,#99859,#99860,#99861,#99862,#99863,#99864,#99865,#99866,#99867,#99868,
#99869,#99870,#99871,#99872,#99873,#99874,#99875,#99876,#99877,#99878,#99879,
#99880,#99881,#99882,#99883,#99884,#99885,#99886,#99887,#99888,#99889,#99890,
#99891,#99892,#99893,#99894,#99895,#99896,#99897,#99898,#99899,#99900,#99901,
#99902,#99903,#99904,#99905,#99906,#99907,#99908,#99909,#99910,#99911,#99912,
#99913,#99914,#99915,#99916,#99917,#99918,#99919,#99920,#99921,#99922,#99923,
#99924,#99925,#99926,#99927,#99928,#99929,#99930,#99931,#99932,#99933,#99934,
#99935,#99936,#99937,#99938,#99939,#99940,#99941,#99942,#99943,#99944,#99945,
#99946,#99947,#99948,#99949,#99950,#99951,#99952,#99953,#99954,#99955,#99956,
#99957,#99958,#99959,#99960,#99961,#99962,#99963,#99964,#99965,#99966,#99967,
#99968,#99969,#99970,#99971,#99972,#99973,#99974,#99975,#99976,#99977,#99978,
#99979,#99980,#99981,#99982,#99983,#99984,#99985,#99986,#99987,#99988,#99989,
#99990,#99991,#99992,#99993,#99994,#99995,#99996,#99997,#99998,#99999,#100000,
#100001,#100002,#100003,#100004,#100005,#100006,#100007,#100008,#100009,
#100010,#100011,#100012,#100013,#100014,#100015,#100016,#100017,#100018,
#100019,#100020,#100021,#100022,#100023,#100024,#100025,#100026,#100027,
#100028,#100029,#100030,#100031,#100032,#100033,#100034,#100035,#100036,
#100037,#100038),.UNSPECIFIED.,.F.,.F.,(4,3,3,3,3,3,3,3,3,3,3,3,3,3,3,3,
3,3,3,3,3,3,3,3,3,3,3,3,3,3,3,3,3,3,3,3,3,3,3,3,3,3,3,3,3,3,3,3,3,3,3,3,
3,3,3,3,3,3,3,3,3,3,3,3,3,3,3,3,3,4),(63.9491534803492,64.0439714327274,
64.1386592433009,64.2366232443927,64.3311438921143,64.4256335614288,64.5201192947624,
64.6146281237261,64.7092427149105,64.8039206481598,64.8987448593486,64.9223712520355,
65.0176003517715,65.1126980239411,65.2076938410773,65.3026210996469,65.3975137831726,
65.4923984567238,65.587301670894,65.6823092191788,65.7773751080585,65.8725951548567,
65.9211769636053,66.0164060633414,66.1115037355109,66.2064995526472,66.3014268112167,
66.3963194947426,66.4912041682941,66.5861073824644,66.6811149307493,66.7761808196289,
66.8714008664272,66.9199826751751,67.0152117749112,67.1103094470804,67.2053052642169,
67.3002325227864,67.3951252063121,67.4900098798635,67.5849130940337,67.6799206423185,
67.7749865311982,67.8702065779964,67.9187883867448,68.0140174864809,68.1091151586503,
68.2041109757866,68.2990382343561,68.3939309178818,68.4888155914332,68.5837188056033,
68.6787263538881,68.7737922427677,68.8690122895659,68.9175940983146,69.0128231980508,
69.1079208702203,69.202916687357,69.2978439459265,69.3927366294522,69.4876213030037,
69.5825245171741,69.6775320654589,69.7725979543382,69.8678180011363,69.9163998098844,
70.0302968077158,70.1429109804956,70.232338577275),.UNSPECIFIED.);
#843=B_SPLINE_CURVE_WITH_KNOTS('',3,(#100040,#100041,#100042,#100043,#100044,
#100045,#100046,#100047,#100048,#100049),.UNSPECIFIED.,.F.,.F.,(4,1,1,1,
1,1,1,4),(70.2323387873437,70.9152055214542,71.9140112330239,72.9128169445937,
73.9116226561635,74.9104283677333,75.9092340793031,76.5155240945233),
 .UNSPECIFIED.);
#844=B_SPLINE_CURVE_WITH_KNOTS('',3,(#100051,#100052,#100053,#100054,#100055,
#100056,#100057,#100058,#100059,#100060),.UNSPECIFIED.,.F.,.F.,(4,1,1,1,
1,1,1,4),(76.5155240945233,76.9080397908728,77.9068455024426,78.9056512140124,
79.9044569255822,80.903262637152,81.9020683487218,82.7987004857864),
 .UNSPECIFIED.);
#845=B_SPLINE_CURVE_WITH_KNOTS('',3,(#100062,#100063,#100064,#100065,#100066,
#100067,#100068,#100069,#100070,#100071,#100072,#100073,#100074,#100075,
#100076,#100077,#100078,#100079,#100080,#100081,#100082,#100083,#100084,
#100085,#100086,#100087,#100088,#100089,#100090,#100091,#100092,#100093,
#100094,#100095,#100096,#100097,#100098,#100099,#100100,#100101,#100102,
#100103,#100104,#100105,#100106,#100107,#100108,#100109,#100110,#100111,
#100112,#100113,#100114,#100115,#100116,#100117,#100118,#100119,#100120,
#100121,#100122,#100123,#100124,#100125,#100126,#100127,#100128,#100129,
#100130,#100131,#100132,#100133,#100134,#100135,#100136,#100137,#100138,
#100139,#100140,#100141,#100142,#100143,#100144,#100145,#100146,#100147,
#100148,#100149,#100150,#100151,#100152,#100153,#100154,#100155,#100156,
#100157,#100158,#100159,#100160,#100161,#100162,#100163,#100164,#100165,
#100166,#100167,#100168,#100169,#100170,#100171,#100172,#100173,#100174,
#100175,#100176,#100177,#100178,#100179,#100180,#100181,#100182,#100183,
#100184,#100185,#100186,#100187,#100188,#100189,#100190,#100191,#100192,
#100193,#100194,#100195,#100196,#100197,#100198,#100199,#100200,#100201,
#100202,#100203,#100204,#100205,#100206,#100207,#100208,#100209,#100210,
#100211,#100212,#100213,#100214,#100215,#100216,#100217,#100218,#100219,
#100220,#100221,#100222,#100223,#100224,#100225,#100226,#100227,#100228,
#100229,#100230,#100231,#100232,#100233,#100234,#100235,#100236,#100237,
#100238,#100239,#100240,#100241,#100242,#100243,#100244,#100245,#100246,
#100247,#100248,#100249,#100250,#100251,#100252,#100253,#100254,#100255,
#100256,#100257,#100258,#100259,#100260,#100261,#100262,#100263,#100264,
#100265,#100266,#100267,#100268,#100269),.UNSPECIFIED.,.F.,.F.,(4,3,3,3,
3,3,3,3,3,3,3,3,3,3,3,3,3,3,3,3,3,3,3,3,3,3,3,3,3,3,3,3,3,3,3,3,3,3,3,3,
3,3,3,3,3,3,3,3,3,3,3,3,3,3,3,3,3,3,3,3,3,3,3,3,3,3,3,3,3,4),(82.7987094017029,
82.9008740602915,82.9961031600276,83.091200832197,83.1861966493334,83.2811239079029,
83.3760165914286,83.47090126498,83.5658044791504,83.6608120274352,83.7558779163149,
83.8510979631131,83.8996797718613,83.9949088715974,84.0900065437669,84.1850023609033,
84.2799296194728,84.3748223029986,84.46970697655,84.5646101907203,84.6596177390052,
84.7546836278848,84.8499036746831,84.8984854834311,84.9937145831671,85.0888122553365,
85.1838080724728,85.2787353310423,85.373628014568,85.4685126881194,85.5634159022897,
85.6584234505745,85.7534893394541,85.8487093862523,85.8972911950008,85.9925202947369,
86.0876179669063,86.1826137840427,86.2775410426122,86.3724337261379,86.4673183996893,
86.5622216138596,86.6572291621444,86.7522950510241,86.8475150978223,86.8960969065706,
86.9913260063067,87.0864236784762,87.1814194956125,87.276346754182,87.3712394377078,
87.4661241112593,87.5610273254296,87.6560348737144,87.7511007625941,87.8463208093923,
87.8949026181404,87.9901317178765,88.0852293900459,88.1802252071822,88.2751524657517,
88.3700451492774,88.4649298228288,88.5598330369991,88.6548405852839,88.7499064741636,
88.8451265209618,88.8937083297102,89.03459316754,89.0818947088825),
 .UNSPECIFIED.);
#846=B_SPLINE_CURVE_WITH_KNOTS('',3,(#100271,#100272,#100273,#100274,#100275,
#100276,#100277,#100278,#100279,#100280),.UNSPECIFIED.,.F.,.F.,(4,1,1,1,
1,1,1,4),(89.08189908702,89.8925140412799,90.8913197528497,91.8901254644195,
92.8889311759893,93.8877368875591,94.8865425991288,95.365078400473),
 .UNSPECIFIED.);
#847=B_SPLINE_CURVE_WITH_KNOTS('',3,(#100282,#100283,#100284,#100285,#100286,
#100287,#100288,#100289,#100290,#100291,#100292,#100293,#100294,#100295,
#100296,#100297,#100298,#100299,#100300,#100301,#100302,#100303,#100304,
#100305,#100306,#100307,#100308,#100309,#100310,#100311,#100312,#100313,
#100314,#100315,#100316,#100317,#100318,#100319,#100320,#100321,#100322,
#100323,#100324,#100325,#100326,#100327,#100328,#100329,#100330,#100331,
#100332,#100333,#100334,#100335,#100336,#100337,#100338,#100339,#100340,
#100341,#100342,#100343,#100344,#100345,#100346,#100347,#100348,#100349,
#100350,#100351,#100352,#100353,#100354,#100355,#100356,#100357,#100358,
#100359,#100360,#100361,#100362,#100363,#100364,#100365,#100366,#100367,
#100368,#100369,#100370,#100371,#100372,#100373,#100374,#100375,#100376,
#100377,#100378,#100379,#100380,#100381,#100382,#100383,#100384,#100385,
#100386,#100387,#100388,#100389,#100390,#100391,#100392,#100393,#100394,
#100395,#100396,#100397,#100398,#100399,#100400,#100401,#100402,#100403,
#100404,#100405,#100406,#100407,#100408,#100409,#100410,#100411,#100412,
#100413,#100414,#100415,#100416,#100417,#100418,#100419,#100420,#100421,
#100422,#100423,#100424,#100425,#100426,#100427,#100428,#100429,#100430,
#100431,#100432,#100433,#100434,#100435,#100436,#100437,#100438,#100439,
#100440,#100441,#100442,#100443,#100444,#100445,#100446,#100447,#100448,
#100449,#100450,#100451,#100452,#100453,#100454,#100455,#100456,#100457,
#100458,#100459,#100460,#100461,#100462,#100463,#100464,#100465,#100466,
#100467,#100468,#100469,#100470,#100471,#100472,#100473,#100474,#100475,
#100476,#100477,#100478,#100479,#100480,#100481,#100482,#100483,#100484,
#100485,#100486,#100487,#100488,#100489,#100490,#100491,#100492),
 .UNSPECIFIED.,.F.,.F.,(4,3,3,3,3,3,3,3,3,3,3,3,3,3,3,3,3,3,3,3,3,3,3,3,
3,3,3,3,3,3,3,3,3,3,3,3,3,3,3,3,3,3,3,3,3,3,3,3,3,3,3,3,3,3,3,3,3,3,3,3,
3,3,3,3,3,3,3,3,3,3,4),(95.3650800160621,95.463654469693,95.5623452628044,
95.6612541125098,95.7602864476327,95.8595327072477,95.8853483106986,95.9805774104347,
96.075675082604,96.1706708997406,96.2655981583101,96.3604908418358,96.4553755153873,
96.5502787295579,96.6452862778428,96.7403521667226,96.8355722135207,96.8841540222684,
96.9793831220044,97.0744807941739,97.1694766113103,97.2644038698798,97.3592965534056,
97.4541812269571,97.5490844411273,97.6440919894121,97.7391578782916,97.8343779250898,
97.8829597338382,97.9781888335742,98.0732865057437,98.1682823228801,98.2632095814496,
98.3581022649753,98.4529869385267,98.5478901526971,98.6428977009819,98.7379635898615,
98.8331836366598,98.881765445408,98.976994545144,99.0720922173134,99.16708803445,
99.2620152930194,99.356907976545,99.4517926500964,99.5466958642667,99.6417034125515,
99.736769301431,99.8319893482292,99.8805711569777,99.9758002567139,100.070897928884,
100.16589374602,100.26082100459,100.355713688116,100.450598361667,100.545501575838,
100.640509124123,100.735575013002,100.830795059801,100.879376868548,100.975487925385,
101.06932774662,101.163078924259,101.256769403842,101.354643383692,101.448325851882,
101.542026129326,101.635804369266,101.648265323242),.UNSPECIFIED.);
#848=B_SPLINE_CURVE_WITH_KNOTS('',3,(#100494,#100495,#100496,#100497,#100498,
#100499,#100500,#100501,#100502,#100503,#100504),.UNSPECIFIED.,.F.,.F.,
(4,1,1,1,1,1,1,1,4),(101.648265323242,101.878182580117,102.876988291687,
103.875794003257,104.874599714827,105.873405426396,106.872211137966,107.871016849536,
107.931450630421),.UNSPECIFIED.);
#849=B_SPLINE_CURVE_WITH_KNOTS('',3,(#100506,#100507,#100508,#100509,#100510,
#100511,#100512,#100513,#100514,#100515,#100516,#100517,#100518,#100519,
#100520,#100521,#100522,#100523,#100524,#100525,#100526,#100527,#100528,
#100529,#100530,#100531,#100532,#100533,#100534,#100535,#100536,#100537,
#100538,#100539,#100540,#100541,#100542,#100543,#100544,#100545,#100546,
#100547,#100548,#100549,#100550,#100551,#100552,#100553,#100554,#100555,
#100556,#100557,#100558,#100559,#100560,#100561,#100562,#100563,#100564,
#100565,#100566,#100567,#100568,#100569,#100570,#100571,#100572,#100573,
#100574,#100575,#100576,#100577,#100578,#100579,#100580,#100581,#100582,
#100583,#100584,#100585,#100586,#100587,#100588,#100589,#100590,#100591,
#100592,#100593,#100594,#100595,#100596,#100597,#100598,#100599,#100600,
#100601,#100602,#100603,#100604,#100605,#100606,#100607,#100608,#100609,
#100610,#100611,#100612,#100613,#100614,#100615,#100616,#100617,#100618,
#100619,#100620,#100621,#100622,#100623,#100624,#100625,#100626,#100627,
#100628,#100629,#100630,#100631,#100632,#100633,#100634,#100635,#100636,
#100637,#100638,#100639,#100640,#100641,#100642,#100643,#100644,#100645,
#100646,#100647,#100648,#100649,#100650,#100651,#100652,#100653,#100654,
#100655,#100656,#100657,#100658,#100659,#100660,#100661,#100662,#100663,
#100664,#100665,#100666,#100667,#100668,#100669,#100670,#100671,#100672,
#100673,#100674,#100675,#100676,#100677,#100678,#100679,#100680,#100681,
#100682,#100683,#100684,#100685,#100686,#100687,#100688,#100689,#100690,
#100691,#100692,#100693,#100694,#100695,#100696,#100697,#100698,#100699,
#100700,#100701,#100702,#100703,#100704,#100705,#100706,#100707,#100708,
#100709,#100710,#100711,#100712,#100713),.UNSPECIFIED.,.F.,.F.,(4,3,3,3,
3,3,3,3,3,3,3,3,3,3,3,3,3,3,3,3,3,3,3,3,3,3,3,3,3,3,3,3,3,3,3,3,3,3,3,3,
3,3,3,3,3,3,3,3,3,3,3,3,3,3,3,3,3,3,3,3,3,3,3,3,3,3,3,3,3,4),(107.931450630421,
108.025811128759,108.120045947231,108.214181269951,108.308262491448,108.402317130539,
108.496372674529,108.590519784193,108.684711144256,108.779067231775,108.869822561106,
108.965051660842,109.060149333012,109.155145150148,109.250072408718,109.344965092244,
109.439849765795,109.534752979965,109.62976052825,109.72482641713,109.820046463928,
109.868628272676,109.963857372412,110.058955044581,110.153950861717,110.248878120286,
110.343770803812,110.438655477363,110.533558691533,110.628566239817,110.723632128697,
110.818852175495,110.867433984245,110.962663083981,111.05776075615,111.152756573287,
111.247683831856,111.342576515382,111.437461188933,111.532364403104,111.627371951389,
111.722437840268,111.817657887066,111.866239695815,111.961468795551,112.056566467721,
112.151562284858,112.246489543427,112.341382226953,112.436266900505,112.531170114675,
112.62617766296,112.72124355184,112.816463598639,112.865045407385,112.960274507121,
113.05537217929,113.150367996427,113.245295254996,113.340187938522,113.435072612074,
113.529975826244,113.624983374529,113.720049263408,113.815269310207,113.863851118955,
113.973858328726,114.083374018364,114.192041198982,114.214635694482),
 .UNSPECIFIED.);
#850=B_SPLINE_CURVE_WITH_KNOTS('',3,(#100715,#100716,#100717,#100718,#100719,
#100720,#100721,#100722,#100723,#100724),.UNSPECIFIED.,.F.,.F.,(4,1,1,1,
1,1,1,4),(114.214635937601,114.862656830524,115.861462542094,116.860268253664,
117.859073965234,118.857879676803,119.856685388373,120.49782124478),
 .UNSPECIFIED.);
#851=B_SPLINE_CURVE_WITH_KNOTS('',3,(#100726,#100727,#100728,#100729,#100730,
#100731,#100732,#100733,#100734,#100735,#100736,#100737,#100738,#100739,
#100740,#100741,#100742,#100743,#100744,#100745,#100746,#100747,#100748,
#100749,#100750,#100751,#100752,#100753,#100754,#100755,#100756,#100757,
#100758,#100759,#100760,#100761,#100762,#100763,#100764,#100765,#100766,
#100767,#100768,#100769,#100770,#100771,#100772,#100773,#100774,#100775,
#100776,#100777,#100778,#100779,#100780,#100781,#100782,#100783,#100784,
#100785,#100786,#100787,#100788,#100789,#100790,#100791,#100792,#100793,
#100794,#100795,#100796,#100797,#100798,#100799,#100800,#100801,#100802,
#100803,#100804,#100805,#100806,#100807,#100808,#100809,#100810,#100811,
#100812,#100813,#100814,#100815,#100816,#100817,#100818,#100819,#100820,
#100821,#100822,#100823,#100824,#100825,#100826,#100827,#100828,#100829,
#100830,#100831,#100832,#100833,#100834,#100835,#100836,#100837,#100838,
#100839,#100840,#100841,#100842,#100843,#100844,#100845,#100846,#100847,
#100848,#100849,#100850,#100851,#100852,#100853,#100854,#100855,#100856,
#100857,#100858,#100859,#100860,#100861,#100862,#100863,#100864,#100865,
#100866,#100867,#100868,#100869,#100870,#100871,#100872,#100873,#100874,
#100875,#100876,#100877,#100878,#100879,#100880,#100881,#100882,#100883,
#100884,#100885,#100886,#100887,#100888,#100889,#100890,#100891,#100892,
#100893,#100894,#100895,#100896,#100897,#100898,#100899,#100900,#100901,
#100902,#100903,#100904,#100905,#100906,#100907,#100908,#100909,#100910,
#100911,#100912,#100913,#100914,#100915,#100916,#100917,#100918,#100919,
#100920,#100921,#100922,#100923,#100924,#100925,#100926,#100927,#100928,
#100929,#100930,#100931,#100932,#100933),.UNSPECIFIED.,.F.,.F.,(4,3,3,3,
3,3,3,3,3,3,3,3,3,3,3,3,3,3,3,3,3,3,3,3,3,3,3,3,3,3,3,3,3,3,3,3,3,3,3,3,
3,3,3,3,3,3,3,3,3,3,3,3,3,3,3,3,3,3,3,3,3,3,3,3,3,3,3,3,3,4),(120.497821489681,
120.606047186385,120.714828214309,120.824262399715,120.855491099943,120.950720199679,
121.045817871849,121.140813688985,121.235740947555,121.33063363108,121.425518304632,
121.520421518802,121.615429067087,121.710494955967,121.805715002765,121.854296811513,
121.949525911249,122.044623583418,122.139619400555,122.234546659124,122.32943934265,
122.424324016201,122.519227230372,122.614234778656,122.709300667536,122.804520714334,
122.853102523083,122.948331622818,123.043429294987,123.138425112122,123.233352370691,
123.328245054216,123.423129727767,123.518032941936,123.61304049022,123.708106379099,
123.803326425896,123.851908234652,123.94713733439,124.042235006561,124.137230823699,
124.232158082271,124.327050765798,124.421935439352,124.516838653524,124.61184620181,
124.706912090692,124.802132137492,124.850713946222,124.945943045957,125.041040718125,
125.13603653526,125.230963793828,125.325856477352,125.420741150902,125.515644365071,
125.610651913355,125.705717802233,125.80093784903,125.849519657792,125.943831432675,
126.038012641317,126.132086892519,126.226102626881,126.320087437328,126.414068880704,
126.508133752517,126.60223937965,126.696499648658,126.78100655196),
 .UNSPECIFIED.);
#852=B_SPLINE_CURVE_WITH_KNOTS('',3,(#100935,#100936,#100937,#100938,#100939,
#100940,#100941,#100942,#100943,#100944,#100945),.UNSPECIFIED.,.F.,.F.,
(4,1,1,1,1,1,1,1,4),(126.78100655196,126.848325369362,127.847131080932,
128.845936792501,129.844742504071,130.843548215641,131.842353927211,132.84115963878,
133.06419185914),.UNSPECIFIED.);
#853=B_SPLINE_CURVE_WITH_KNOTS('',3,(#100947,#100948,#100949,#100950,#100951,
#100952,#100953,#100954,#100955,#100956,#100957,#100958,#100959,#100960,
#100961,#100962,#100963,#100964,#100965,#100966,#100967,#100968,#100969,
#100970,#100971,#100972,#100973,#100974,#100975,#100976,#100977,#100978,
#100979,#100980,#100981,#100982,#100983,#100984,#100985,#100986,#100987,
#100988,#100989,#100990,#100991,#100992,#100993,#100994,#100995,#100996,
#100997,#100998,#100999,#101000,#101001,#101002,#101003,#101004,#101005,
#101006,#101007,#101008,#101009,#101010,#101011,#101012,#101013,#101014,
#101015,#101016,#101017,#101018,#101019,#101020,#101021,#101022,#101023,
#101024,#101025,#101026,#101027,#101028,#101029,#101030,#101031,#101032,
#101033,#101034,#101035,#101036,#101037,#101038,#101039,#101040,#101041,
#101042,#101043,#101044,#101045,#101046,#101047,#101048,#101049,#101050,
#101051,#101052,#101053,#101054,#101055,#101056,#101057,#101058,#101059,
#101060,#101061,#101062,#101063,#101064,#101065,#101066,#101067,#101068,
#101069,#101070,#101071,#101072,#101073,#101074,#101075,#101076,#101077,
#101078,#101079,#101080,#101081,#101082,#101083,#101084,#101085,#101086,
#101087,#101088,#101089,#101090,#101091,#101092,#101093,#101094,#101095,
#101096,#101097,#101098,#101099,#101100,#101101,#101102,#101103,#101104,
#101105,#101106,#101107,#101108,#101109,#101110,#101111,#101112,#101113,
#101114,#101115,#101116,#101117,#101118,#101119,#101120,#101121,#101122,
#101123,#101124,#101125,#101126,#101127,#101128,#101129,#101130,#101131,
#101132,#101133,#101134,#101135,#101136,#101137,#101138,#101139,#101140,
#101141,#101142,#101143,#101144,#101145,#101146,#101147,#101148,#101149,
#101150,#101151,#101152,#101153,#101154,#101155,#101156,#101157),
 .UNSPECIFIED.,.F.,.F.,(4,3,3,3,3,3,3,3,3,3,3,3,3,3,3,3,3,3,3,3,3,3,3,3,
3,3,3,3,3,3,3,3,3,3,3,3,3,3,3,3,3,3,3,3,3,3,3,3,3,3,3,3,3,3,3,3,3,3,3,3,
3,3,3,3,3,3,3,3,3,3,4),(133.06419185914,133.161163545541,133.254836014875,
133.348471030653,133.442096465485,133.535740176565,133.629484588454,133.723289562586,
133.817238172544,133.83996535035,133.93519444913,134.030292120345,134.125287936529,
134.220215194155,134.315107876743,134.409992549363,134.504895762609,134.599903309987,
134.694969197968,134.790189243889,134.83877106192,134.934000161428,135.02909783336,
135.124093650249,135.219020908559,135.313913591817,135.408798265093,135.503701478981,
135.598709026974,135.693774915557,135.788994962053,135.83757677349,135.932805877182,
136.027903553322,136.122899374438,136.217826636983,136.312719324482,136.407604001998,
136.502507220119,136.597514772312,136.69258066508,136.787800715699,136.836382485059,
136.931611577449,137.02670924228,137.121705052093,137.216632303392,137.311524979684,
137.406409646045,137.501312853078,137.596320394349,137.691386276274,137.786606316277,
137.835188196629,137.930417297129,138.025514969997,138.120510787766,138.21543804687,
138.310330730868,138.405215404831,138.500118619351,138.595126167891,138.690192056973,
138.785412103889,138.833993908199,138.933518394371,139.036983087358,139.136092611983,
139.235066506161,139.333886280039,139.347377166319),.UNSPECIFIED.);
#854=B_SPLINE_CURVE_WITH_KNOTS('',3,(#101159,#101160,#101161,#101162,#101163,
#101164,#101165,#101166,#101167,#101168),.UNSPECIFIED.,.F.,.F.,(4,1,1,1,
1,1,1,4),(139.347378254301,139.832799619769,140.831605331339,141.830411042908,
142.829216754478,143.828022466048,144.826828177618,145.630562473499),
 .UNSPECIFIED.);
#855=B_SPLINE_CURVE_WITH_KNOTS('',3,(#101170,#101171,#101172,#101173,#101174,
#101175,#101176,#101177,#101178,#101179),.UNSPECIFIED.,.F.,.F.,(4,1,1,1,
1,1,1,4),(145.630562473499,145.825633889187,146.824439600757,147.823245312327,
148.822051023897,149.820856735467,150.819662447036,151.160872120126),
 .UNSPECIFIED.);
#856=B_SPLINE_CURVE_WITH_KNOTS('',3,(#101183,#101184,#101185,#101186,#101187,
#101188,#101189,#101190,#101191,#101192,#101193,#101194,#101195,#101196,
#101197,#101198,#101199,#101200,#101201,#101202,#101203,#101204,#101205,
#101206,#101207,#101208,#101209,#101210,#101211,#101212,#101213,#101214,
#101215,#101216,#101217,#101218,#101219,#101220,#101221,#101222,#101223,
#101224,#101225,#101226,#101227,#101228,#101229,#101230,#101231,#101232,
#101233,#101234,#101235,#101236,#101237,#101238,#101239,#101240,#101241,
#101242,#101243,#101244,#101245,#101246,#101247,#101248,#101249,#101250,
#101251,#101252,#101253,#101254,#101255,#101256,#101257,#101258,#101259,
#101260,#101261,#101262,#101263,#101264,#101265,#101266,#101267,#101268,
#101269,#101270,#101271,#101272,#101273,#101274,#101275,#101276,#101277,
#101278,#101279,#101280,#101281,#101282,#101283,#101284,#101285,#101286,
#101287,#101288,#101289,#101290,#101291,#101292,#101293,#101294,#101295,
#101296,#101297,#101298,#101299,#101300,#101301,#101302,#101303,#101304,
#101305,#101306,#101307,#101308,#101309,#101310,#101311,#101312,#101313,
#101314,#101315,#101316,#101317,#101318,#101319,#101320,#101321,#101322,
#101323,#101324,#101325,#101326,#101327,#101328,#101329,#101330,#101331,
#101332,#101333),.UNSPECIFIED.,.F.,.F.,(4,3,3,3,3,3,3,3,3,3,3,3,3,3,3,3,
3,3,3,3,3,3,3,3,3,3,3,3,3,3,3,3,3,3,3,3,3,3,3,3,3,3,3,3,3,3,3,3,3,3,4),
(-153.229489605841,-153.13007506582,-153.030363631848,-152.930499334661,
-152.830341227169,-152.747163592623,-152.651787242391,-152.556542086082,
-152.461398768752,-152.366324659609,-152.271285582085,-152.176255164369,
-152.08120704973,-151.98605691229,-151.890849469052,-151.795491178329,-151.748816118161,
-151.653415212671,-151.558142356049,-151.462968244962,-151.367858839775,
-151.272781679139,-151.177710427419,-151.082618761718,-150.987421187822,
-150.892164024966,-150.796752931837,-150.750468643699,-150.655362433477,
-150.56038925176,-150.465519347467,-150.370719626968,-150.275955435646,
-150.181200054995,-150.086426781627,-149.991549499601,-149.896614184718,
-149.801524227629,-149.752121169238,-149.656859041422,-149.561728112202,
-149.466698857429,-149.371738058406,-149.27681177294,-149.181893478322,
-149.086956666316,-148.991915884423,-148.896816845217,-148.801564410731,
-148.753773694776,-148.606192485261),.UNSPECIFIED.);
#857=B_SPLINE_CURVE_WITH_KNOTS('',3,(#101335,#101336,#101337,#101338,#101339,
#101340,#101341,#101342,#101343,#101344),.UNSPECIFIED.,.F.,.F.,(4,1,1,1,
1,1,1,4),(-148.606185112125,-147.755426220315,-146.757078745853,-145.758731271391,
-144.76038379693,-143.762036322468,-142.763688848007,-142.323011718186),
 .UNSPECIFIED.);
#858=B_SPLINE_CURVE_WITH_KNOTS('',3,(#101346,#101347,#101348,#101349,#101350,
#101351,#101352,#101353,#101354,#101355,#101356,#101357,#101358,#101359,
#101360,#101361,#101362,#101363,#101364,#101365,#101366,#101367,#101368,
#101369,#101370,#101371,#101372,#101373,#101374,#101375,#101376,#101377,
#101378,#101379,#101380,#101381,#101382,#101383,#101384,#101385,#101386,
#101387,#101388,#101389,#101390,#101391,#101392,#101393,#101394,#101395,
#101396,#101397,#101398,#101399,#101400,#101401,#101402,#101403,#101404,
#101405,#101406,#101407,#101408,#101409,#101410,#101411,#101412,#101413,
#101414,#101415,#101416,#101417,#101418,#101419,#101420,#101421,#101422,
#101423,#101424,#101425,#101426,#101427,#101428,#101429,#101430,#101431,
#101432,#101433,#101434,#101435,#101436,#101437,#101438,#101439,#101440,
#101441,#101442,#101443,#101444,#101445,#101446,#101447,#101448,#101449,
#101450,#101451,#101452,#101453,#101454,#101455,#101456,#101457,#101458,
#101459,#101460,#101461,#101462,#101463,#101464,#101465,#101466,#101467,
#101468,#101469,#101470,#101471,#101472,#101473,#101474,#101475,#101476,
#101477,#101478,#101479,#101480,#101481,#101482,#101483,#101484,#101485,
#101486,#101487,#101488,#101489,#101490,#101491,#101492,#101493,#101494,
#101495,#101496,#101497,#101498,#101499,#101500,#101501,#101502,#101503,
#101504,#101505,#101506,#101507,#101508,#101509,#101510,#101511,#101512,
#101513,#101514,#101515,#101516,#101517,#101518,#101519,#101520,#101521,
#101522,#101523,#101524,#101525,#101526,#101527,#101528,#101529,#101530,
#101531,#101532,#101533,#101534,#101535,#101536,#101537,#101538,#101539,
#101540,#101541,#101542,#101543,#101544,#101545,#101546,#101547,#101548,
#101549,#101550,#101551,#101552,#101553),.UNSPECIFIED.,.F.,.F.,(4,3,3,3,
3,3,3,3,3,3,3,3,3,3,3,3,3,3,3,3,3,3,3,3,3,3,3,3,3,3,3,3,3,3,3,3,3,3,3,3,
3,3,3,3,3,3,3,3,3,3,3,3,3,3,3,3,3,3,3,3,3,3,3,3,3,3,3,3,3,4),(-142.323007178082,
-142.225700249726,-142.128324098792,-142.030775269004,-141.933134923198,
-141.835287450591,-141.765341373545,-141.670107095845,-141.575004137981,
-141.480002935616,-141.385070189996,-141.290171947565,-141.195281650218,
-141.10037275427,-141.005359593337,-140.910288048079,-140.815062640428,
-140.766993899084,-140.671759096531,-140.576655606462,-140.481653865323,
-140.386720573393,-140.291821780179,-140.196930928246,-140.102021474583,
-140.007007754557,-139.911935648591,-139.816709683177,-139.768646424622,
-139.673411759562,-139.57830840789,-139.48330680585,-139.388373653479,-139.293475000054,
-139.198584287968,-139.103674974034,-139.008661392702,-138.913589425047,
-138.818363595997,-138.77029895016,-138.675064351112,-138.579961066957,
-138.484959533839,-138.390026452196,-138.295127870597,-138.200237231348,
-138.105327991176,-138.010314484572,-137.915242592306,-137.820016838941,
-137.771951475699,-137.67671680145,-137.581613440991,-137.486611830579,
-137.391678670491,-137.296780009761,-137.201889290791,-137.106979970405,
-137.011966383323,-136.916894410309,-136.821668576563,-136.773604001237,
-136.679360684964,-136.585237144751,-136.491205576827,-136.397238279117,
-136.303283812116,-136.209340629697,-136.115332569317,-136.039821870902),
 .UNSPECIFIED.);
#859=B_SPLINE_CURVE_WITH_KNOTS('',3,(#101555,#101556,#101557,#101558,#101559,
#101560,#101561,#101562,#101563,#101564,#101565,#101566,#101567,#101568,
#101569,#101570,#101571,#101572,#101573,#101574,#101575,#101576,#101577,
#101578,#101579,#101580,#101581,#101582,#101583,#101584,#101585,#101586,
#101587,#101588,#101589,#101590,#101591,#101592,#101593,#101594,#101595,
#101596,#101597,#101598,#101599,#101600,#101601,#101602,#101603,#101604,
#101605,#101606,#101607,#101608,#101609,#101610,#101611,#101612,#101613,
#101614,#101615,#101616,#101617,#101618,#101619,#101620,#101621,#101622,
#101623,#101624,#101625,#101626,#101627,#101628,#101629,#101630,#101631,
#101632,#101633,#101634,#101635,#101636,#101637,#101638,#101639,#101640,
#101641,#101642,#101643,#101644,#101645,#101646,#101647,#101648,#101649,
#101650,#101651,#101652,#101653,#101654,#101655,#101656,#101657,#101658,
#101659,#101660,#101661,#101662,#101663,#101664,#101665,#101666,#101667,
#101668,#101669,#101670,#101671,#101672,#101673,#101674,#101675,#101676,
#101677,#101678,#101679,#101680,#101681,#101682,#101683,#101684,#101685,
#101686,#101687,#101688,#101689,#101690,#101691,#101692,#101693,#101694,
#101695,#101696,#101697,#101698,#101699,#101700,#101701,#101702,#101703,
#101704,#101705,#101706,#101707,#101708,#101709,#101710,#101711,#101712,
#101713,#101714,#101715,#101716,#101717,#101718,#101719,#101720,#101721,
#101722,#101723,#101724,#101725,#101726,#101727,#101728,#101729,#101730,
#101731,#101732,#101733,#101734,#101735,#101736,#101737,#101738,#101739,
#101740,#101741,#101742,#101743,#101744,#101745,#101746,#101747,#101748,
#101749,#101750,#101751,#101752,#101753,#101754,#101755,#101756,#101757,
#101758,#101759,#101760,#101761,#101762,#101763,#101764,#101765),
 .UNSPECIFIED.,.F.,.F.,(4,3,3,3,3,3,3,3,3,3,3,3,3,3,3,3,3,3,3,3,3,3,3,3,
3,3,3,3,3,3,3,3,3,3,3,3,3,3,3,3,3,3,3,3,3,3,3,3,3,3,3,3,3,3,3,3,3,3,3,3,
3,3,3,3,3,3,3,3,3,3,4),(-136.039821870719,-135.920529986285,-135.79889642772,
-135.775256526776,-135.680021883788,-135.584918554985,-135.489916976577,
-135.394983848877,-135.300085220761,-135.205194534592,-135.110285247153,
-135.015271693041,-134.920199753059,-134.824973952119,-134.776909052314,
-134.681674398784,-134.586571059276,-134.491569470019,-134.396636331297,
-134.301737692057,-134.206846994674,-134.111937695947,-134.016924130499,
-133.921852179138,-133.826626366862,-133.778561577852,-133.683326928468,
-133.588223593148,-133.493222008114,-133.398288873651,-133.303390238691,
-133.208499545602,-133.113590251179,-133.018576690024,-132.923504742956,
-132.82827893493,-132.780214103391,-132.684979454547,-132.589876119788,
-132.494874535335,-132.399941401479,-132.305042767143,-132.210152074695,
-132.115242780927,-132.020229220446,-131.925157274065,-131.829931466738,
-131.781866628929,-131.686631978641,-131.591528642414,-131.496527056472,
-131.401593921103,-131.306695285238,-131.211804591248,-131.116895295927,
-131.021881733886,-130.926809785936,-130.831583977046,-130.783519154468,
-130.688284504851,-130.593181169304,-130.498179584047,-130.403246449371,
-130.308347814202,-130.213457120912,-130.118547826292,-130.023534264952,
-129.928462317704,-129.83323650951,-129.785171680006,-129.756636563722),
 .UNSPECIFIED.);
#860=B_SPLINE_CURVE_WITH_KNOTS('',3,(#101767,#101768,#101769,#101770,#101771,
#101772,#101773,#101774,#101775,#101776,#101777,#101778,#101779,#101780,
#101781,#101782,#101783,#101784,#101785,#101786,#101787,#101788,#101789,
#101790,#101791,#101792,#101793,#101794,#101795,#101796,#101797,#101798,
#101799,#101800,#101801,#101802,#101803,#101804,#101805,#101806,#101807,
#101808,#101809,#101810,#101811,#101812,#101813,#101814,#101815,#101816,
#101817,#101818,#101819,#101820,#101821,#101822,#101823,#101824,#101825,
#101826,#101827,#101828,#101829,#101830,#101831,#101832,#101833,#101834,
#101835,#101836,#101837,#101838,#101839,#101840,#101841,#101842,#101843,
#101844,#101845,#101846,#101847,#101848,#101849,#101850,#101851,#101852,
#101853,#101854,#101855,#101856,#101857,#101858,#101859,#101860,#101861,
#101862,#101863,#101864,#101865,#101866,#101867,#101868,#101869,#101870,
#101871,#101872,#101873,#101874,#101875,#101876,#101877,#101878,#101879,
#101880,#101881,#101882,#101883,#101884,#101885,#101886,#101887,#101888,
#101889,#101890,#101891,#101892,#101893,#101894,#101895,#101896,#101897,
#101898,#101899,#101900,#101901,#101902,#101903,#101904,#101905,#101906,
#101907,#101908,#101909,#101910,#101911,#101912,#101913,#101914,#101915,
#101916,#101917,#101918,#101919,#101920,#101921,#101922,#101923,#101924,
#101925,#101926,#101927,#101928,#101929,#101930,#101931,#101932,#101933,
#101934,#101935,#101936,#101937,#101938,#101939,#101940,#101941,#101942,
#101943,#101944,#101945,#101946,#101947,#101948,#101949,#101950,#101951,
#101952,#101953,#101954,#101955,#101956,#101957,#101958,#101959,#101960,
#101961,#101962,#101963,#101964,#101965,#101966,#101967,#101968,#101969,
#101970,#101971,#101972,#101973,#101974),.UNSPECIFIED.,.F.,.F.,(4,3,3,3,
3,3,3,3,3,3,3,3,3,3,3,3,3,3,3,3,3,3,3,3,3,3,3,3,3,3,3,3,3,3,3,3,3,3,3,3,
3,3,3,3,3,3,3,3,3,3,3,3,3,3,3,3,3,3,3,3,3,3,3,3,3,3,3,3,3,4),(-129.756636563519,
-129.661856131417,-129.567205464658,-129.469657807268,-129.375173110179,
-129.280719043156,-129.186268524364,-129.091794482415,-128.997214655407,
-128.902571022647,-128.807782068836,-128.786824205545,-128.69158955575,
-128.596486220024,-128.501484634587,-128.40655149973,-128.311652864381,
-128.21676217091,-128.121852876109,-128.02683931459,-127.931767367163,-127.836541558792,
-127.788476731083,-127.693242081393,-127.598138745774,-127.503137160445,
-127.408204025697,-127.313305390457,-127.218414697095,-127.123505402406,
-127.028491840997,-126.93341989368,-126.83819408542,-126.790129256621,-126.694894606925,
-126.599791271299,-126.504789685965,-126.409856551211,-126.314957915965,
-126.220067222599,-126.125157927904,-126.03014436649,-125.93507241917,-125.839846610905,
-125.79178178216,-125.696547132439,-125.601443796787,-125.506442211426,
-125.411509076645,-125.316610441373,-125.221719747979,-125.126810453257,
-125.031796891815,-124.936724944467,-124.841499136174,-124.793434307698,
-124.698199657993,-124.603096322357,-124.508094737013,-124.413161602249,
-124.318262966993,-124.223372273616,-124.12846297891,-124.033449417486,
-123.938377470154,-123.843151661878,-123.795086833237,-123.681923502067,
-123.569966114734,-123.473451256749),.UNSPECIFIED.);
#861=B_SPLINE_CURVE_WITH_KNOTS('',3,(#101976,#101977,#101978,#101979,#101980,
#101981,#101982,#101983,#101984,#101985,#101986,#101987,#101988,#101989,
#101990,#101991,#101992,#101993,#101994,#101995,#101996,#101997,#101998,
#101999,#102000,#102001,#102002,#102003,#102004,#102005,#102006,#102007,
#102008,#102009,#102010,#102011,#102012,#102013,#102014,#102015,#102016,
#102017,#102018,#102019,#102020,#102021,#102022,#102023,#102024,#102025,
#102026,#102027,#102028,#102029,#102030,#102031,#102032,#102033,#102034,
#102035,#102036,#102037,#102038,#102039,#102040,#102041,#102042,#102043,
#102044,#102045,#102046,#102047,#102048,#102049,#102050,#102051,#102052,
#102053,#102054,#102055,#102056,#102057,#102058,#102059,#102060,#102061,
#102062,#102063,#102064,#102065,#102066,#102067,#102068,#102069,#102070,
#102071,#102072,#102073,#102074,#102075,#102076,#102077,#102078,#102079,
#102080,#102081,#102082,#102083,#102084,#102085,#102086,#102087,#102088,
#102089,#102090,#102091,#102092,#102093,#102094,#102095,#102096,#102097,
#102098,#102099,#102100,#102101,#102102,#102103,#102104,#102105,#102106,
#102107,#102108,#102109,#102110,#102111,#102112,#102113,#102114,#102115,
#102116,#102117,#102118,#102119,#102120,#102121,#102122,#102123,#102124,
#102125,#102126,#102127,#102128,#102129,#102130,#102131,#102132,#102133,
#102134,#102135,#102136,#102137,#102138,#102139,#102140,#102141,#102142,
#102143,#102144,#102145,#102146,#102147,#102148,#102149,#102150,#102151,
#102152,#102153,#102154,#102155,#102156,#102157,#102158,#102159,#102160,
#102161,#102162,#102163,#102164,#102165,#102166,#102167,#102168,#102169,
#102170,#102171,#102172,#102173,#102174,#102175,#102176,#102177,#102178,
#102179,#102180,#102181,#102182,#102183,#102184,#102185,#102186),
 .UNSPECIFIED.,.F.,.F.,(4,3,3,3,3,3,3,3,3,3,3,3,3,3,3,3,3,3,3,3,3,3,3,3,
3,3,3,3,3,3,3,3,3,3,3,3,3,3,3,3,3,3,3,3,3,3,3,3,3,3,3,3,3,3,3,3,3,3,3,3,
3,3,3,3,3,3,3,3,3,3,4),(-123.473451256543,-123.37878647411,-123.284143660694,
-123.189496038614,-123.091306868655,-122.996510725647,-122.901643366946,
-122.806627936808,-122.796739358775,-122.701504709064,-122.606401373423,
-122.511399788073,-122.416466653303,-122.321568018042,-122.226677324659,
-122.131768029948,-122.036754468518,-121.941682521181,-121.846456712899,
-121.798391884313,-121.703157234605,-121.608053898967,-121.51305231362,
-121.418119178853,-121.323220543594,-121.228329850215,-121.133420555507,
-121.038406994079,-120.943335046745,-120.848109238466,-120.800044409852,
-120.704809760143,-120.609706424505,-120.514704839156,-120.419771704389,
-120.32487306913,-120.229982375749,-120.13507308104,-120.040059519612,-119.944987572277,
-119.849761763998,-119.80169693539,-119.706462285681,-119.611358950042,
-119.516357364693,-119.421424229925,-119.326525594666,-119.231634901285,
-119.136725606576,-119.041712045147,-118.946640097812,-118.851414289532,
-118.803349460929,-118.708114811221,-118.613011475582,-118.518009890234,
-118.423076755466,-118.328178120207,-118.233287426827,-118.138378132118,
-118.04336457069,-117.948292623355,-117.853066815076,-117.805001986467,
-117.708768823806,-117.612674740797,-117.516694597092,-117.420813827615,
-117.324990934663,-117.229194871666,-117.190265949363),.UNSPECIFIED.);
#862=B_SPLINE_CURVE_WITH_KNOTS('',3,(#102188,#102189,#102190,#102191,#102192,
#102193,#102194,#102195,#102196,#102197),.UNSPECIFIED.,.F.,.F.,(4,1,1,1,
1,1,1,4),(-117.190258575718,-116.806654512005,-115.808307037544,-114.809959563082,
-113.811612088621,-112.813264614159,-111.814917139698,-110.907089376591),
 .UNSPECIFIED.);
#863=B_SPLINE_CURVE_WITH_KNOTS('',3,(#102199,#102200,#102201,#102202,#102203,
#102204,#102205,#102206,#102207,#102208,#102209,#102210,#102211,#102212,
#102213,#102214,#102215,#102216,#102217,#102218,#102219,#102220,#102221,
#102222,#102223,#102224,#102225,#102226,#102227,#102228,#102229,#102230,
#102231,#102232,#102233,#102234,#102235,#102236,#102237,#102238,#102239,
#102240,#102241,#102242,#102243,#102244,#102245,#102246,#102247,#102248,
#102249,#102250,#102251,#102252,#102253,#102254,#102255,#102256,#102257,
#102258,#102259,#102260,#102261,#102262,#102263,#102264,#102265,#102266,
#102267,#102268,#102269,#102270,#102271,#102272,#102273,#102274,#102275,
#102276,#102277,#102278,#102279,#102280,#102281,#102282,#102283,#102284,
#102285,#102286,#102287,#102288,#102289,#102290,#102291,#102292,#102293,
#102294,#102295,#102296,#102297,#102298,#102299,#102300,#102301,#102302,
#102303,#102304,#102305,#102306,#102307,#102308,#102309,#102310,#102311,
#102312,#102313,#102314,#102315,#102316,#102317,#102318,#102319,#102320,
#102321,#102322,#102323,#102324,#102325,#102326,#102327,#102328,#102329,
#102330,#102331,#102332,#102333,#102334,#102335,#102336,#102337,#102338,
#102339,#102340,#102341,#102342,#102343,#102344,#102345,#102346,#102347,
#102348,#102349,#102350,#102351,#102352,#102353,#102354,#102355,#102356,
#102357,#102358,#102359,#102360,#102361,#102362,#102363,#102364,#102365,
#102366,#102367,#102368,#102369,#102370,#102371,#102372,#102373,#102374,
#102375,#102376,#102377,#102378,#102379,#102380,#102381,#102382,#102383,
#102384,#102385,#102386,#102387,#102388,#102389,#102390,#102391,#102392,
#102393,#102394,#102395,#102396,#102397,#102398,#102399,#102400,#102401,
#102402,#102403,#102404,#102405,#102406),.UNSPECIFIED.,.F.,.F.,(4,3,3,3,
3,3,3,3,3,3,3,3,3,3,3,3,3,3,3,3,3,3,3,3,3,3,3,3,3,3,3,3,3,3,3,3,3,3,3,3,
3,3,3,3,3,3,3,3,3,3,3,3,3,3,3,3,3,3,3,3,3,3,3,3,3,3,3,3,3,4),(-110.907080642184,
-110.816569665236,-110.721335015528,-110.62623167989,-110.531230094543,
-110.436296959776,-110.341398324518,-110.246507631139,-110.151598336431,
-110.056584775004,-109.96151282767,-109.866287019391,-109.818222190774,
-109.722987541065,-109.627884205426,-109.532882620078,-109.43794948531,
-109.343050850051,-109.24816015667,-109.153250861961,-109.058237300533,
-108.963165353198,-108.867939544919,-108.819874716313,-108.724640066604,
-108.629536730965,-108.534535145616,-108.439602010848,-108.344703375589,
-108.249812682208,-108.154903387499,-108.05988982607,-107.964817878735,
-107.869592070455,-107.821527241851,-107.726292592142,-107.631189256504,
-107.536187671156,-107.441254536388,-107.346355901129,-107.251465207749,
-107.15655591304,-107.061542351612,-106.966470404277,-106.871244595998,
-106.82317976739,-106.727945117681,-106.632841782042,-106.537840196694,
-106.442907061927,-106.348008426667,-106.253117733287,-106.158208438578,
-106.06319487715,-105.968122929814,-105.872897121535,-105.824832292928,
-105.729597643219,-105.63449430758,-105.539492722231,-105.444559587463,
-105.349660952204,-105.254770258823,-105.159860964113,-105.064847402685,
-104.96977545535,-104.87454964707,-104.826484818466,-104.69097746786,-104.623895335004),
 .UNSPECIFIED.);
#864=B_SPLINE_CURVE_WITH_KNOTS('',3,(#102408,#102409,#102410,#102411,#102412,
#102413,#102414,#102415,#102416,#102417),.UNSPECIFIED.,.F.,.F.,(4,1,1,1,
1,1,1,4),(-104.623892444637,-103.828137344005,-102.829789869543,-101.831442395082,
-100.83309492062,-99.8347474461585,-98.8363999716969,-98.3407100278245),
 .UNSPECIFIED.);
#865=B_SPLINE_CURVE_WITH_KNOTS('',3,(#102419,#102420,#102421,#102422,#102423,
#102424,#102425,#102426,#102427,#102428),.UNSPECIFIED.,.F.,.F.,(4,1,1,1,
1,1,1,4),(-98.3407100278245,-97.8380524972354,-96.8397050227738,-95.8413575483122,
-94.8430100738506,-93.844662599389,-92.8463151249274,-92.0575269460171),
 .UNSPECIFIED.);
#866=B_SPLINE_CURVE_WITH_KNOTS('',3,(#102430,#102431,#102432,#102433,#102434,
#102435,#102436,#102437,#102438,#102439,#102440,#102441,#102442,#102443,
#102444,#102445,#102446,#102447,#102448,#102449,#102450,#102451,#102452,
#102453,#102454,#102455,#102456,#102457,#102458,#102459,#102460,#102461,
#102462,#102463,#102464,#102465,#102466,#102467,#102468,#102469,#102470,
#102471,#102472,#102473,#102474,#102475,#102476,#102477,#102478,#102479,
#102480,#102481,#102482,#102483,#102484,#102485,#102486,#102487,#102488,
#102489,#102490,#102491,#102492,#102493,#102494,#102495,#102496,#102497,
#102498,#102499,#102500,#102501,#102502,#102503,#102504,#102505,#102506,
#102507,#102508,#102509,#102510,#102511,#102512,#102513,#102514,#102515,
#102516,#102517,#102518,#102519,#102520,#102521,#102522,#102523,#102524,
#102525,#102526,#102527,#102528,#102529,#102530,#102531,#102532,#102533,
#102534,#102535,#102536,#102537,#102538,#102539,#102540,#102541,#102542,
#102543,#102544,#102545,#102546,#102547,#102548,#102549,#102550,#102551,
#102552,#102553,#102554,#102555,#102556,#102557,#102558,#102559,#102560,
#102561,#102562,#102563,#102564,#102565,#102566,#102567,#102568,#102569,
#102570,#102571,#102572,#102573,#102574,#102575,#102576,#102577,#102578,
#102579,#102580,#102581,#102582,#102583,#102584,#102585,#102586,#102587,
#102588,#102589,#102590,#102591,#102592,#102593,#102594,#102595,#102596,
#102597,#102598,#102599,#102600,#102601,#102602,#102603,#102604,#102605,
#102606,#102607,#102608,#102609,#102610,#102611,#102612,#102613,#102614,
#102615,#102616,#102617,#102618,#102619,#102620,#102621,#102622,#102623,
#102624,#102625,#102626,#102627,#102628,#102629,#102630,#102631,#102632,
#102633,#102634,#102635,#102636,#102637),.UNSPECIFIED.,.F.,.F.,(4,3,3,3,
3,3,3,3,3,3,3,3,3,3,3,3,3,3,3,3,3,3,3,3,3,3,3,3,3,3,3,3,3,3,3,3,3,3,3,3,
3,3,3,3,3,3,3,3,3,3,3,3,3,3,3,3,3,3,3,3,3,3,3,3,3,3,3,3,3,4),(-92.0575247206449,
-91.9242393989711,-91.8479676504659,-91.7527330007571,-91.6576296651182,
-91.5626280797698,-91.467694945002,-91.3727963097427,-91.277905616362,-91.182996321653,
-91.0879827602248,-90.9929108128895,-90.8976850046099,-90.8496201760043,
-90.7543855262956,-90.6592821906567,-90.5642806053084,-90.4693474705408,
-90.3744488352815,-90.2795581419008,-90.1846488471919,-90.0896352857637,
-89.9945633384285,-89.899337530149,-89.8512727015427,-89.756038051834,-89.6609347161951,
-89.5659331308468,-89.4709999960792,-89.3761013608199,-89.2812106674393,
-89.1863013727303,-89.0912878113021,-88.996215863967,-88.9009900556875,
-88.8529252270811,-88.7576905773724,-88.6625872417335,-88.5675856563851,
-88.4726525216175,-88.3777538863582,-88.2828631929775,-88.1879538982686,
-88.0929403368404,-87.9978683895053,-87.9026425812257,-87.8545777526195,
-87.7593431029108,-87.6642397672719,-87.5692381819235,-87.4743050471559,
-87.3794064118966,-87.2845157185159,-87.1896064238069,-87.0945928623787,
-86.9995209150436,-86.904295106764,-86.8562302781579,-86.7609956284492,
-86.6658922928102,-86.5708907074618,-86.4759575726941,-86.3810589374349,
-86.2861682440542,-86.1912589493452,-86.096245387917,-86.0011734405818,
-85.9059476323023,-85.8578828036963,-85.7743394134653),.UNSPECIFIED.);
#867=B_SPLINE_CURVE_WITH_KNOTS('',3,(#102639,#102640,#102641,#102642,#102643,
#102644,#102645,#102646,#102647,#102648),.UNSPECIFIED.,.F.,.F.,(4,1,1,1,
1,1,1,4),(-85.7743308767921,-84.8595353292348,-83.8611878547732,-82.8628403803116,
-81.86449290585,-80.8661454313884,-79.8677979569268,-79.4911616095461),
 .UNSPECIFIED.);
#868=B_SPLINE_CURVE_WITH_KNOTS('',3,(#102650,#102651,#102652,#102653,#102654,
#102655,#102656,#102657,#102658,#102659,#102660,#102661,#102662,#102663,
#102664,#102665,#102666,#102667,#102668,#102669,#102670,#102671,#102672,
#102673,#102674,#102675,#102676,#102677,#102678,#102679,#102680,#102681,
#102682,#102683,#102684,#102685,#102686,#102687,#102688,#102689,#102690,
#102691,#102692,#102693,#102694,#102695,#102696,#102697,#102698,#102699,
#102700,#102701,#102702,#102703,#102704,#102705,#102706,#102707,#102708,
#102709,#102710,#102711,#102712,#102713,#102714,#102715,#102716,#102717,
#102718,#102719,#102720,#102721,#102722,#102723,#102724,#102725,#102726,
#102727,#102728,#102729,#102730,#102731,#102732,#102733,#102734,#102735,
#102736,#102737,#102738,#102739,#102740,#102741,#102742,#102743,#102744,
#102745,#102746,#102747,#102748,#102749,#102750,#102751,#102752,#102753,
#102754,#102755,#102756,#102757,#102758,#102759,#102760,#102761,#102762,
#102763,#102764,#102765,#102766,#102767,#102768,#102769,#102770,#102771,
#102772,#102773,#102774,#102775,#102776,#102777,#102778,#102779,#102780,
#102781,#102782,#102783,#102784,#102785,#102786,#102787,#102788,#102789,
#102790,#102791,#102792,#102793,#102794,#102795,#102796,#102797,#102798,
#102799,#102800,#102801,#102802,#102803,#102804,#102805,#102806,#102807,
#102808,#102809,#102810,#102811,#102812,#102813,#102814,#102815,#102816,
#102817,#102818,#102819,#102820,#102821,#102822,#102823,#102824,#102825,
#102826,#102827,#102828,#102829,#102830,#102831,#102832,#102833,#102834,
#102835,#102836,#102837,#102838,#102839,#102840,#102841,#102842,#102843,
#102844,#102845,#102846,#102847,#102848,#102849,#102850,#102851,#102852,
#102853,#102854,#102855,#102856,#102857),.UNSPECIFIED.,.F.,.F.,(4,3,3,3,
3,3,3,3,3,3,3,3,3,3,3,3,3,3,3,3,3,3,3,3,3,3,3,3,3,3,3,3,3,3,3,3,3,3,3,3,
3,3,3,3,3,3,3,3,3,3,3,3,3,3,3,3,3,3,3,3,3,3,3,3,3,3,3,3,3,4),(-79.4911541062857,
-79.3955028226438,-79.2998389542877,-79.2041373614416,-79.108306823325,
-79.012403860413,-78.9163300256675,-78.8694504824652,-78.7742158327565,
-78.6791124971176,-78.5841109117691,-78.4891777770015,-78.3942791417422,
-78.2993884483615,-78.2044791536523,-78.1094655922242,-78.014393644889,
-77.9191678366095,-77.8711030080037,-77.7758683582949,-77.680765022656,
-77.5857634373076,-77.4908303025399,-77.3959316672807,-77.3010409739002,
-77.2061316791911,-77.111118117763,-77.0160461704278,-76.9208203621483,
-76.8727555335421,-76.7775208838335,-76.6824175481943,-76.5874159628459,
-76.4924828280783,-76.397584192819,-76.3026934994381,-76.2077842047291,
-76.1127706433009,-76.0176986959657,-75.9224728876861,-75.8744080590805,
-75.7791734093716,-75.684070073733,-75.5890684883847,-75.4941353536171,
-75.3992367183578,-75.3043460249771,-75.2094367302681,-75.1144231688399,
-75.0193512215048,-74.9241254132253,-74.8760605846189,-74.78082593491,-74.6857225992712,
-74.5907210139224,-74.4957878791548,-74.4008892438955,-74.3059985505149,
-74.2110892558056,-74.1160756943774,-74.0210037470425,-73.925777938763,
-73.8777131101573,-73.7826130999192,-73.6876406133148,-73.5927687779015,
-73.4965687832027,-73.4018105821085,-73.3048896906073,-73.2079687991061),
 .UNSPECIFIED.);
#869=B_SPLINE_CURVE_WITH_KNOTS('',3,(#102859,#102860,#102861,#102862,#102863,
#102864,#102865,#102866,#102867,#102868),.UNSPECIFIED.,.F.,.F.,(4,1,1,1,
1,1,1,4),(-73.2079617521312,-72.8793656356957,-71.8810181612341,-70.8826706867726,
-69.884323212311,-68.8859757378494,-67.8876282633878,-66.9247882546445),
 .UNSPECIFIED.);
#870=B_SPLINE_CURVE_WITH_KNOTS('',3,(#102870,#102871,#102872,#102873,#102874,
#102875,#102876,#102877,#102878,#102879,#102880,#102881,#102882,#102883,
#102884,#102885,#102886,#102887,#102888,#102889,#102890,#102891,#102892,
#102893,#102894,#102895,#102896,#102897,#102898,#102899,#102900,#102901,
#102902,#102903,#102904,#102905,#102906,#102907,#102908,#102909,#102910,
#102911,#102912,#102913,#102914,#102915,#102916,#102917,#102918,#102919,
#102920,#102921,#102922,#102923,#102924,#102925,#102926,#102927,#102928,
#102929,#102930,#102931,#102932,#102933,#102934,#102935,#102936,#102937,
#102938,#102939,#102940,#102941,#102942,#102943,#102944,#102945,#102946,
#102947,#102948,#102949,#102950,#102951,#102952,#102953,#102954,#102955,
#102956,#102957,#102958,#102959,#102960,#102961,#102962,#102963,#102964,
#102965,#102966,#102967,#102968,#102969,#102970,#102971,#102972,#102973,
#102974,#102975,#102976,#102977,#102978,#102979,#102980,#102981,#102982,
#102983,#102984,#102985,#102986,#102987,#102988,#102989,#102990,#102991,
#102992,#102993,#102994,#102995,#102996,#102997,#102998,#102999,#103000,
#103001,#103002,#103003,#103004,#103005,#103006,#103007,#103008,#103009,
#103010,#103011,#103012,#103013,#103014,#103015,#103016,#103017,#103018,
#103019,#103020,#103021,#103022,#103023,#103024,#103025,#103026,#103027,
#103028,#103029,#103030,#103031,#103032,#103033,#103034,#103035,#103036,
#103037,#103038,#103039,#103040,#103041,#103042,#103043,#103044,#103045,
#103046,#103047,#103048,#103049,#103050,#103051,#103052,#103053,#103054,
#103055,#103056,#103057,#103058,#103059,#103060,#103061,#103062,#103063,
#103064,#103065,#103066,#103067,#103068,#103069,#103070,#103071,#103072,
#103073,#103074,#103075,#103076,#103077,#103078,#103079,#103080),
 .UNSPECIFIED.,.F.,.F.,(4,3,3,3,3,3,3,3,3,3,3,3,3,3,3,3,3,3,3,3,3,3,3,3,
3,3,3,3,3,3,3,3,3,3,3,3,3,3,3,3,3,3,3,3,3,3,3,3,3,3,3,3,3,3,3,3,3,3,3,3,
3,3,3,3,3,3,3,3,3,3,4),(-66.9247834919265,-66.8892807889262,-66.7940461392173,
-66.6989428035783,-66.6039412182297,-66.5090080834618,-66.4141094482023,
-66.3192187548215,-66.2243094601123,-66.1292958986839,-66.0342239513486,
-65.9389981430689,-65.8909333144646,-65.7956986647559,-65.700595329117,
-65.6055937437686,-65.510660609001,-65.4157619737417,-65.3208712803611,
-65.2259619856521,-65.1309484242239,-65.0358764768888,-64.9406506686093,
-64.892585840003,-64.7973511902943,-64.7022478546555,-64.6072462693071,
-64.5123131345395,-64.4174144992803,-64.3225238058997,-64.2276145111908,
-64.1326009497626,-64.0375290024275,-63.942303194148,-63.8942383655415,
-63.7990037158327,-63.7039003801939,-63.6088987948455,-63.5139656600778,
-63.4190670248185,-63.3241763314379,-63.2292670367289,-63.1342534753007,
-63.0391815279656,-62.943955719686,-62.8958908910799,-62.8006562413711,
-62.7055529057322,-62.6105513203839,-62.5156181856163,-62.420719550357,
-62.3258288569763,-62.2309195622674,-62.1359060008392,-62.0408340535041,
-61.9456082452245,-61.8975434166183,-61.8023087669095,-61.7072054312706,
-61.6122038459222,-61.5172707111546,-61.4223720758953,-61.3274813825147,
-61.2325720878058,-61.1375585263776,-61.0424865790424,-60.9472607707629,
-60.8991959421567,-60.7703971397938,-60.6499426268912,-60.641598337431),
 .UNSPECIFIED.);
#871=B_SPLINE_CURVE_WITH_KNOTS('',3,(#103082,#103083,#103084,#103085,#103086,
#103087,#103088,#103089,#103090,#103091),.UNSPECIFIED.,.F.,.F.,(4,1,1,1,
1,1,1,4),(-60.6415981847469,-59.9008484676951,-58.9025009932335,-57.9041535187719,
-56.9058060443104,-55.9074585698488,-54.9091110953872,-54.3584128775673),
 .UNSPECIFIED.);
#872=B_SPLINE_CURVE_WITH_KNOTS('',3,(#103093,#103094,#103095,#103096,#103097,
#103098,#103099,#103100,#103101,#103102),.UNSPECIFIED.,.F.,.F.,(4,1,1,1,
1,1,1,4),(-54.3584128775673,-53.9107636209256,-52.912416146464,-51.9140686720024,
-50.9157211975409,-49.9173737230793,-48.9190262486177,-48.0752346473835),
 .UNSPECIFIED.);
#873=B_SPLINE_CURVE_WITH_KNOTS('',3,(#103104,#103105,#103106,#103107,#103108,
#103109,#103110,#103111,#103112,#103113,#103114,#103115,#103116,#103117,
#103118,#103119,#103120,#103121,#103122,#103123,#103124,#103125,#103126,
#103127,#103128,#103129,#103130,#103131,#103132,#103133,#103134,#103135,
#103136,#103137,#103138,#103139,#103140,#103141,#103142,#103143,#103144,
#103145,#103146,#103147,#103148,#103149,#103150,#103151,#103152,#103153,
#103154,#103155,#103156,#103157,#103158,#103159,#103160,#103161,#103162,
#103163,#103164,#103165,#103166,#103167,#103168,#103169,#103170,#103171,
#103172,#103173,#103174,#103175,#103176,#103177,#103178,#103179,#103180,
#103181,#103182,#103183,#103184,#103185,#103186,#103187,#103188,#103189,
#103190,#103191,#103192,#103193,#103194,#103195,#103196,#103197,#103198,
#103199,#103200,#103201,#103202,#103203,#103204,#103205,#103206,#103207,
#103208,#103209,#103210,#103211,#103212,#103213,#103214,#103215,#103216,
#103217,#103218,#103219,#103220,#103221,#103222,#103223,#103224,#103225,
#103226,#103227,#103228,#103229,#103230,#103231,#103232,#103233,#103234,
#103235,#103236,#103237,#103238,#103239,#103240,#103241,#103242,#103243,
#103244,#103245,#103246,#103247,#103248,#103249,#103250,#103251,#103252,
#103253,#103254,#103255,#103256,#103257,#103258,#103259,#103260,#103261,
#103262,#103263,#103264,#103265,#103266,#103267,#103268,#103269,#103270,
#103271,#103272,#103273,#103274,#103275,#103276,#103277,#103278,#103279,
#103280,#103281,#103282,#103283,#103284,#103285,#103286,#103287,#103288,
#103289,#103290,#103291,#103292,#103293,#103294,#103295,#103296,#103297,
#103298,#103299,#103300,#103301,#103302,#103303,#103304,#103305,#103306,
#103307,#103308),.UNSPECIFIED.,.F.,.F.,(4,3,3,3,3,3,3,3,3,3,3,3,3,3,3,3,
3,3,3,3,3,3,3,3,3,3,3,3,3,3,3,3,3,3,3,3,3,3,3,3,3,3,3,3,3,3,3,3,3,3,3,3,
3,3,3,3,3,3,3,3,3,3,3,3,3,3,3,3,4),(-48.0752275703878,-47.9206787741561,
-47.8254441244474,-47.7303407888087,-47.6353392034605,-47.540406068693,
-47.4455074334337,-47.3506167400531,-47.2557074453443,-47.1606938839162,
-47.0656219365811,-46.9703961283017,-46.9223312996945,-46.8270966499857,
-46.7319933143469,-46.6369917289985,-46.5420585942308,-46.4471599589715,
-46.3522692655909,-46.257359970882,-46.1623464094538,-46.0672744621186,
-45.9720486538391,-45.9239838252329,-45.8287491755241,-45.7336458398853,
-45.6386442545369,-45.5437111197692,-45.4488124845099,-45.3539217911292,
-45.2590124964203,-45.163998934992,-45.0689269876569,-44.9737011793773,
-44.9256363507713,-44.8304017010626,-44.7352983654238,-44.6402967800754,
-44.5453636453078,-44.4504650100485,-44.3555743166679,-44.260665021959,
-44.1656514605309,-44.0705795131957,-43.9753537049162,-43.9272888763098,
-43.832054226601,-43.7369508909622,-43.6419493056139,-43.5470161708462,
-43.4521175355869,-43.3572268422062,-43.2623175474973,-43.1673039860691,
-43.072232038734,-42.9770062304545,-42.9289414018482,-42.8337067521394,
-42.7386034165005,-42.6436018311521,-42.5486686963844,-42.4537700611251,
-42.3588793677445,-42.2639700730357,-42.1689565116075,-42.0738845642722,
-41.9786587559927,-41.9305939273866,-41.7920422632082),.UNSPECIFIED.);
#874=B_SPLINE_CURVE_WITH_KNOTS('',3,(#103310,#103311,#103312,#103313,#103314,
#103315,#103316,#103317,#103318,#103319),.UNSPECIFIED.,.F.,.F.,(4,1,1,1,
1,1,1,4),(-41.7920342547179,-40.932246452925,-39.9338989784634,-38.9355515040018,
-37.9372040295402,-36.9388565550787,-35.9405090806171,-35.5088620686574),
 .UNSPECIFIED.);
#875=B_SPLINE_CURVE_WITH_KNOTS('',3,(#103321,#103322,#103323,#103324,#103325,
#103326,#103327,#103328,#103329,#103330,#103331,#103332,#103333,#103334,
#103335,#103336,#103337,#103338,#103339,#103340,#103341,#103342,#103343,
#103344,#103345,#103346,#103347,#103348,#103349,#103350,#103351,#103352,
#103353,#103354,#103355,#103356,#103357,#103358,#103359,#103360,#103361,
#103362,#103363,#103364,#103365,#103366,#103367,#103368,#103369,#103370,
#103371,#103372,#103373,#103374,#103375,#103376,#103377,#103378,#103379,
#103380,#103381,#103382,#103383,#103384,#103385,#103386,#103387,#103388,
#103389,#103390,#103391,#103392,#103393,#103394,#103395,#103396,#103397,
#103398,#103399,#103400,#103401,#103402,#103403,#103404,#103405,#103406,
#103407,#103408,#103409,#103410,#103411,#103412,#103413,#103414,#103415,
#103416,#103417,#103418,#103419,#103420,#103421,#103422,#103423,#103424,
#103425,#103426,#103427,#103428,#103429,#103430,#103431,#103432,#103433,
#103434,#103435,#103436,#103437,#103438,#103439,#103440,#103441,#103442,
#103443,#103444,#103445,#103446,#103447,#103448,#103449,#103450,#103451,
#103452,#103453,#103454,#103455,#103456,#103457,#103458,#103459,#103460,
#103461,#103462,#103463,#103464,#103465,#103466,#103467,#103468,#103469,
#103470,#103471,#103472,#103473,#103474,#103475,#103476,#103477,#103478,
#103479,#103480,#103481,#103482,#103483,#103484,#103485,#103486,#103487,
#103488,#103489,#103490,#103491,#103492,#103493,#103494,#103495,#103496,
#103497,#103498,#103499,#103500,#103501,#103502,#103503,#103504,#103505,
#103506,#103507,#103508,#103509,#103510,#103511,#103512,#103513,#103514,
#103515,#103516,#103517,#103518,#103519,#103520,#103521,#103522,#103523,
#103524,#103525,#103526,#103527,#103528),.UNSPECIFIED.,.F.,.F.,(4,3,3,3,
3,3,3,3,3,3,3,3,3,3,3,3,3,3,3,3,3,3,3,3,3,3,3,3,3,3,3,3,3,3,3,3,3,3,3,3,
3,3,3,3,3,3,3,3,3,3,3,3,3,3,3,3,3,3,3,3,3,3,3,3,3,3,3,3,3,4),(-35.5088569560286,
-35.4118208844685,-35.3147250894648,-35.2174658762113,-35.1201218755024,
-35.0225716951327,-34.9421616061555,-34.8469269564469,-34.751823620808,
-34.6568220354598,-34.5618889006923,-34.4669902654331,-34.3720995720527,
-34.277190277344,-34.182176715916,-34.0871047685808,-33.9918789603015,-33.9438141316939,
-33.8485794819858,-33.7534761463474,-33.6584745609995,-33.5635414262326,
-33.468642790974,-33.373752097594,-33.2788428028856,-33.1838292414581,-33.0887572941236,
-32.9935314858447,-32.9454666572323,-32.8502320075217,-32.7551286718808,
-32.6601270865306,-32.5651939517611,-32.4702953164998,-32.3754046231173,
-32.280495328406,-32.185481766976,-32.0904098196392,-31.995184011358,-31.9471191827707,
-31.8518845330635,-31.756781197426,-31.6617796120795,-31.5668464773133,
-31.4719478420554,-31.3770571486762,-31.282147853969,-31.1871342925423,
-31.0920623452084,-30.9968365369302,-30.9487717083091,-30.853537058604,
-30.7584337229687,-30.6634321376237,-30.5684990028597,-30.4736003676041,
-30.378709674227,-30.2838003795219,-30.1887868180976,-30.0937148707661,
-29.9984890624903,-29.9504242338476,-29.8560879209494,-29.7618722070048,
-29.6677493757309,-29.5736918118656,-29.4796504770907,-29.3856213085643,
-29.291533789037,-29.225671648849),.UNSPECIFIED.);
#876=B_SPLINE_CURVE_WITH_KNOTS('',3,(#103530,#103531,#103532,#103533,#103534,
#103535,#103536,#103537,#103538,#103539,#103540),.UNSPECIFIED.,.F.,.F.,
(4,1,1,1,1,1,1,1,4),(-29.2256678766635,-28.952076759386,-27.9537292849244,
-26.9553818104628,-25.9570343360012,-24.9586868615396,-23.960339387078,
-22.9619919126165,-22.9424863416694),.UNSPECIFIED.);
#877=B_SPLINE_CURVE_WITH_KNOTS('',3,(#103542,#103543,#103544,#103545,#103546,
#103547,#103548,#103549,#103550,#103551,#103552,#103553,#103554,#103555,
#103556,#103557,#103558,#103559,#103560,#103561,#103562,#103563,#103564,
#103565,#103566,#103567,#103568,#103569,#103570,#103571,#103572,#103573,
#103574,#103575,#103576,#103577,#103578,#103579,#103580,#103581,#103582,
#103583,#103584,#103585,#103586,#103587,#103588,#103589,#103590,#103591,
#103592,#103593,#103594,#103595,#103596,#103597,#103598,#103599,#103600,
#103601,#103602,#103603,#103604,#103605,#103606,#103607,#103608,#103609,
#103610,#103611,#103612,#103613,#103614,#103615,#103616,#103617,#103618,
#103619,#103620,#103621,#103622,#103623,#103624,#103625,#103626,#103627,
#103628,#103629,#103630,#103631,#103632,#103633,#103634,#103635,#103636,
#103637,#103638,#103639,#103640,#103641,#103642,#103643,#103644,#103645,
#103646,#103647,#103648,#103649,#103650,#103651,#103652,#103653,#103654,
#103655,#103656,#103657,#103658,#103659,#103660,#103661,#103662,#103663,
#103664,#103665,#103666,#103667,#103668,#103669,#103670,#103671,#103672,
#103673,#103674,#103675,#103676,#103677,#103678,#103679,#103680,#103681,
#103682,#103683,#103684,#103685,#103686,#103687,#103688,#103689,#103690,
#103691,#103692,#103693,#103694,#103695,#103696,#103697,#103698,#103699,
#103700,#103701,#103702,#103703,#103704,#103705,#103706,#103707,#103708,
#103709,#103710,#103711,#103712,#103713,#103714,#103715,#103716,#103717,
#103718,#103719,#103720,#103721,#103722,#103723,#103724,#103725,#103726,
#103727,#103728,#103729,#103730,#103731,#103732,#103733,#103734,#103735,
#103736,#103737,#103738,#103739,#103740,#103741,#103742,#103743,#103744,
#103745,#103746,#103747,#103748,#103749),.UNSPECIFIED.,.F.,.F.,(4,3,3,3,
3,3,3,3,3,3,3,3,3,3,3,3,3,3,3,3,3,3,3,3,3,3,3,3,3,3,3,3,3,3,3,3,3,3,3,3,
3,3,3,3,3,3,3,3,3,3,3,3,3,3,3,3,3,3,3,3,3,3,3,3,3,3,3,3,3,4),(-22.9424863416694,
-22.8475708151219,-22.7527857967021,-22.6541431268837,-22.5595268545539,
-22.4649420606623,-22.3703618097769,-22.2757591778819,-22.1810510326589,
-22.0862803854588,-21.9913622734999,-21.9636444381549,-21.8684097886978,
-21.7733064533207,-21.6783048682431,-21.5833717337592,-21.4884730987915,
-21.3935824057097,-21.2986731113068,-21.203659550193,-21.1085876031777,
-21.013361795223,-20.9652969636933,-20.8700623100051,-20.7749589703722,
-20.6799573810214,-20.5850242422547,-20.4901256029999,-20.3952349056325,
-20.3003256069498,-20.2053120415923,-20.110240090347,-20.0150142782255,
-19.9669494892317,-19.8717148468358,-19.7766115185031,-19.6816099404442,
-19.5866768129127,-19.4917781848538,-19.3968874986289,-19.301978211023,
-19.2069646565748,-19.1118927161601,-19.0166669146419,-18.9686020147701,
-18.8733673644384,-18.7782640282422,-18.683262442402,-18.588329307241,-18.4934306716492,
-18.3985399779968,-18.3036306830774,-18.2086171215313,-18.1135451741308,
-18.0183193658673,-17.9702545403085,-17.8750198652429,-17.7799165041353,
-17.684914893242,-17.5899817329218,-17.4950830721146,-17.4001923532219,
-17.3052830330679,-17.2102694464511,-17.115197474035,-17.019971641087,-16.9719070658469,
-16.8576236664657,-16.7446612540388,-16.6593012388575),.UNSPECIFIED.);
#878=B_SPLINE_CURVE_WITH_KNOTS('',3,(#103751,#103752,#103753,#103754,#103755,
#103756,#103757,#103758,#103759,#103760),.UNSPECIFIED.,.F.,.F.,(4,1,1,1,
1,1,1,4),(-16.6593010344898,-15.9735595913854,-14.9752121169238,-13.9768646424622,
-12.9785171680006,-11.980169693539,-10.9818222190774,-10.3761157273102),
 .UNSPECIFIED.);
#879=B_SPLINE_CURVE_WITH_KNOTS('',3,(#103761,#103762,#103763,#103764,#103765,
#103766,#103767,#103768,#103769,#103770),.UNSPECIFIED.,.F.,.F.,(4,1,1,1,
1,1,1,4),(-10.3761157273102,-9.98347474461585,-8.98512727015427,-7.98677979569268,
-6.9884323212311,-5.99008484676951,-4.99173737230793,-4.09293042013064),
 .UNSPECIFIED.);
#880=B_SPLINE_CURVE_WITH_KNOTS('',3,(#103773,#103774,#103775,#103776),
 .UNSPECIFIED.,.F.,.F.,(4,4),(-0.0182935576830915,-0.000735173289463335),
 .UNSPECIFIED.);
#881=B_SPLINE_CURVE_WITH_KNOTS('',3,(#103778,#103779,#103780,#103781,#103782,
#103783,#103784,#103785,#103786,#103787,#103788,#103789,#103790,#103791,
#103792,#103793,#103794,#103795,#103796,#103797,#103798,#103799,#103800,
#103801,#103802,#103803,#103804,#103805,#103806,#103807,#103808,#103809,
#103810,#103811,#103812,#103813,#103814,#103815,#103816,#103817,#103818,
#103819,#103820,#103821,#103822,#103823,#103824,#103825,#103826,#103827,
#103828,#103829,#103830,#103831,#103832,#103833,#103834,#103835,#103836,
#103837,#103838,#103839,#103840,#103841,#103842,#103843,#103844,#103845,
#103846,#103847,#103848,#103849,#103850,#103851,#103852,#103853,#103854,
#103855,#103856,#103857,#103858,#103859,#103860,#103861,#103862,#103863,
#103864,#103865,#103866,#103867,#103868,#103869,#103870,#103871,#103872,
#103873,#103874,#103875,#103876,#103877,#103878,#103879,#103880,#103881,
#103882,#103883,#103884,#103885,#103886,#103887,#103888,#103889,#103890,
#103891,#103892,#103893,#103894,#103895,#103896,#103897,#103898,#103899,
#103900,#103901,#103902,#103903,#103904,#103905,#103906,#103907,#103908,
#103909,#103910,#103911,#103912,#103913,#103914,#103915,#103916,#103917,
#103918,#103919,#103920,#103921,#103922,#103923,#103924,#103925,#103926,
#103927,#103928,#103929,#103930,#103931,#103932,#103933,#103934,#103935,
#103936,#103937,#103938,#103939,#103940,#103941,#103942,#103943,#103944,
#103945,#103946,#103947,#103948,#103949,#103950,#103951,#103952,#103953,
#103954,#103955,#103956,#103957,#103958,#103959,#103960,#103961),
 .UNSPECIFIED.,.F.,.F.,(4,3,3,3,3,3,3,3,3,3,3,3,3,3,3,3,3,3,3,3,3,3,3,3,
3,3,3,3,3,3,3,3,3,3,3,3,3,3,3,3,3,3,3,3,3,3,3,3,3,3,3,3,3,3,3,3,3,3,3,3,
3,4),(160.221225333079,160.368806542595,160.469339670852,160.569727809779,
160.669999441629,160.770207358655,160.870382770703,160.970556846841,161.070830871274,
161.171152974707,161.27165768423,161.367154017056,161.467516405285,161.567733113192,
161.66783306709,161.767869225672,161.867873027848,161.967875871739,162.067980449723,
162.168133797921,162.268472935545,162.365501491518,162.466201520456,162.56675562374,
162.667191045365,162.767561354686,162.867897546487,162.968230573328,163.068659575677,
163.169134733737,163.269787443802,163.363848965979,163.464493158123,163.564994418424,
163.665381690691,163.76570671933,163.866000534004,163.966294124919,164.066688533638,
164.167131688191,164.267757109287,164.362196440441,164.461610403654,164.560878328294,
164.66083652662,164.759929309251,164.858993337879,164.958061073645,165.05868178396,
165.157920089979,165.259232002441,165.360543914903,165.463867173735,165.567024747684,
165.670017169689,165.772912391584,165.875735823741,165.978512792525,166.081298147787,
166.184082570356,166.286939951846,166.358891389364),.UNSPECIFIED.);
#882=B_SPLINE_CURVE_WITH_KNOTS('',3,(#103965,#103966,#103967,#103968,#103969,
#103970,#103971,#103972,#103973,#103974,#103975,#103976,#103977,#103978,
#103979,#103980,#103981,#103982,#103983,#103984,#103985,#103986,#103987,
#103988,#103989,#103990,#103991,#103992,#103993,#103994,#103995,#103996,
#103997,#103998,#103999,#104000,#104001,#104002,#104003,#104004,#104005,
#104006,#104007,#104008,#104009,#104010,#104011,#104012,#104013,#104014,
#104015,#104016,#104017,#104018,#104019,#104020,#104021,#104022,#104023,
#104024,#104025,#104026,#104027,#104028,#104029,#104030,#104031,#104032,
#104033,#104034,#104035,#104036,#104037,#104038,#104039,#104040,#104041,
#104042,#104043,#104044,#104045,#104046,#104047,#104048,#104049,#104050,
#104051,#104052,#104053,#104054,#104055,#104056,#104057,#104058,#104059,
#104060,#104061,#104062,#104063,#104064,#104065,#104066,#104067,#104068,
#104069,#104070,#104071,#104072,#104073,#104074,#104075,#104076,#104077,
#104078,#104079,#104080,#104081,#104082,#104083,#104084,#104085,#104086,
#104087,#104088,#104089,#104090,#104091,#104092,#104093,#104094,#104095,
#104096,#104097,#104098,#104099,#104100,#104101,#104102,#104103,#104104,
#104105,#104106,#104107,#104108,#104109,#104110,#104111,#104112),
 .UNSPECIFIED.,.F.,.F.,(4,3,3,3,3,3,3,3,3,3,3,3,3,3,3,3,3,3,3,3,3,3,3,3,
3,3,3,3,3,3,3,3,3,3,3,3,3,3,3,3,3,3,3,3,3,3,3,3,3,4),(160.221225333356,
160.320301206291,160.420857483327,160.519706082362,160.618507137317,160.717293427671,
160.819157926397,160.918073596558,161.021412509567,161.124751422577,161.225446048277,
161.325994622524,161.426424373396,161.526788920669,161.627119267854,161.727446376164,
161.827869516093,161.928338756658,162.028985881907,162.123557134147,162.224194799688,
162.32468940722,162.425069890594,162.525388042217,162.625674901913,162.725961469978,
162.826348931459,162.926785091202,163.027403880915,163.122362845717,163.221770660997,
163.321032315316,163.421049345562,163.520135597098,163.619193029126,163.718254109008,
163.818982721077,163.918214476708,164.019691516997,164.121168557286,164.224488491831,
164.327642572721,164.430631285823,164.533522676262,164.636342167034,164.739115097018,
164.841896378103,164.944676659303,165.047530054968,165.119974268856),
 .UNSPECIFIED.);
#883=B_SPLINE_CURVE_WITH_KNOTS('',3,(#104113,#104114,#104115,#104116,#104117,
#104118),.UNSPECIFIED.,.F.,.F.,(4,2,4),(-2.98959515967248,-2.97760081308363,
-2.9723526798557),.UNSPECIFIED.);
#884=B_SPLINE_CURVE_WITH_KNOTS('',3,(#104121,#104122,#104123,#104124,#104125,
#104126,#104127,#104128,#104129,#104130,#104131,#104132,#104133,#104134,
#104135,#104136,#104137,#104138,#104139,#104140,#104141,#104142,#104143,
#104144,#104145,#104146,#104147,#104148,#104149,#104150,#104151,#104152),
 .UNSPECIFIED.,.F.,.F.,(4,2,2,2,2,2,2,2,2,2,2,2,2,2,2,4),(-1.69880658936105,
-1.64118631745314,-1.58114877567363,-1.48716057166322,-1.37259659624477,
-1.23655075175843,-1.07630244975344,-0.917316760995069,-0.841499276240901,
-0.674438906112136,-0.53603761134625,-0.366273268631182,-0.24012056206555,
-0.139018770734191,-0.0749773698883539,-0.000229398401183072),
 .UNSPECIFIED.);
#885=B_SPLINE_CURVE_WITH_KNOTS('',3,(#104153,#104154,#104155,#104156,#104157,
#104158,#104159,#104160,#104161,#104162,#104163,#104164,#104165,#104166,
#104167,#104168,#104169,#104170,#104171,#104172,#104173,#104174,#104175,
#104176,#104177,#104178,#104179,#104180,#104181,#104182,#104183,#104184,
#104185,#104186,#104187,#104188,#104189,#104190,#104191,#104192,#104193,
#104194,#104195,#104196,#104197,#104198,#104199,#104200,#104201,#104202,
#104203,#104204,#104205,#104206,#104207,#104208,#104209,#104210,#104211,
#104212,#104213,#104214,#104215,#104216),.UNSPECIFIED.,.F.,.F.,(4,3,3,3,
3,3,3,3,3,3,3,3,3,3,3,3,3,3,3,3,3,4),(-0.410648750432886,-0.38129858226722,
-0.351337992790239,-0.323268054558464,-0.314071396249984,-0.306968635230723,
-0.302737007688542,-0.275182991632929,-0.261456224359294,-0.23321386673853,
-0.204062133396214,-0.199389510033103,-0.195719588682917,-0.168524343679287,
-0.141432694273413,-0.114802283736653,-0.100451998269572,-0.0961034389970428,
-0.0703282844310466,-0.0449344423665578,-0.0202868318695185,0.),
 .UNSPECIFIED.);
#886=B_SPLINE_CURVE_WITH_KNOTS('',3,(#104218,#104219,#104220,#104221,#104222,
#104223,#104224,#104225,#104226,#104227,#104228,#104229,#104230,#104231,
#104232,#104233,#104234,#104235,#104236,#104237,#104238,#104239,#104240,
#104241,#104242,#104243,#104244,#104245,#104246,#104247,#104248),
 .UNSPECIFIED.,.F.,.F.,(4,3,3,3,3,3,3,3,3,3,4),(-0.219677966287973,-0.192200047075235,
-0.164960141568471,-0.163244232429979,-0.133734144811955,-0.116159664156593,
-0.111352235849027,-0.0817226425906419,-0.0517048216881644,-0.0217334754545278,
-7.02415695071034E-6),.UNSPECIFIED.);
#887=B_SPLINE_CURVE_WITH_KNOTS('',3,(#104249,#104250,#104251,#104252),
 .UNSPECIFIED.,.F.,.F.,(4,4),(-0.000229398401183072,-6.51013309275102E-5),
 .UNSPECIFIED.);
#888=B_SPLINE_CURVE_WITH_KNOTS('',3,(#104888,#104889,#104890,#104891,#104892,
#104893,#104894,#104895,#104896,#104897,#104898,#104899,#104900,#104901,
#104902,#104903,#104904,#104905,#104906,#104907,#104908,#104909,#104910,
#104911,#104912,#104913,#104914,#104915,#104916,#104917,#104918,#104919,
#104920,#104921,#104922,#104923,#104924,#104925,#104926,#104927,#104928,
#104929,#104930,#104931,#104932,#104933,#104934,#104935,#104936,#104937,
#104938,#104939,#104940,#104941,#104942,#104943,#104944,#104945,#104946,
#104947,#104948,#104949,#104950,#104951,#104952,#104953,#104954,#104955,
#104956,#104957,#104958,#104959,#104960,#104961,#104962,#104963,#104964,
#104965,#104966,#104967,#104968,#104969,#104970,#104971,#104972,#104973,
#104974,#104975,#104976,#104977,#104978),.UNSPECIFIED.,.F.,.F.,(4,3,3,3,
3,3,3,3,3,3,3,3,3,3,3,3,3,3,3,3,3,3,3,3,3,3,3,3,3,3,4),(-0.55274537837504,
-0.531622029508336,-0.502168749051018,-0.486643707191791,-0.477816865703623,
-0.472110472955742,-0.443081444772573,-0.414132449696304,-0.402724598745165,
-0.39668011484503,-0.368410079973193,-0.34044453265584,-0.313301444273823,
-0.297447725699577,-0.291428269583587,-0.264625124759166,-0.252536542129385,
-0.224781440291452,-0.197026338453519,-0.192163335093477,-0.188174560077401,
-0.161544510496889,-0.134901746785557,-0.108748508340938,-0.0997156910642904,
-0.0945974717680295,-0.0905458946870925,-0.0649973519765065,-0.0398488838857292,
-0.0154859190233527,-2.23248444130412E-15),.UNSPECIFIED.);
#889=B_SPLINE_CURVE_WITH_KNOTS('',3,(#105620,#105621,#105622,#105623,#105624,
#105625,#105626,#105627,#105628,#105629,#105630,#105631,#105632,#105633,
#105634,#105635,#105636,#105637,#105638,#105639,#105640,#105641,#105642,
#105643,#105644,#105645,#105646,#105647,#105648,#105649,#105650,#105651,
#105652,#105653,#105654,#105655,#105656,#105657,#105658,#105659,#105660,
#105661,#105662,#105663,#105664,#105665,#105666,#105667,#105668,#105669,
#105670,#105671,#105672,#105673,#105674,#105675,#105676,#105677,#105678,
#105679,#105680,#105681,#105682,#105683,#105684,#105685,#105686,#105687,
#105688,#105689,#105690,#105691,#105692,#105693,#105694,#105695,#105696,
#105697,#105698,#105699,#105700,#105701,#105702,#105703,#105704,#105705,
#105706,#105707),.UNSPECIFIED.,.F.,.F.,(4,3,3,3,3,3,3,3,3,3,3,3,3,3,3,3,
3,3,3,3,3,3,3,3,3,3,3,3,3,4),(-0.555272788399368,-0.538161110412913,-0.513269663833761,
-0.491669801821604,-0.486294250181284,-0.460760853903715,-0.434570412970994,
-0.426707251754789,-0.422174147549878,-0.395448584781258,-0.368380105141822,
-0.341395216874052,-0.330298718755938,-0.32518015111859,-0.321082990951348,
-0.293166557766596,-0.28265706582854,-0.255451682715235,-0.22824629960193,
-0.222182340122818,-0.217930129258396,-0.190046398040851,-0.161669107568982,
-0.132937855371596,-0.116194762555652,-0.111789614273972,-0.0823323644615424,
-0.0527795159223115,-0.0237791283446704,0.),.UNSPECIFIED.);
#890=B_SPLINE_CURVE_WITH_KNOTS('',3,(#105708,#105709,#105710,#105711),
 .UNSPECIFIED.,.F.,.F.,(4,4),(-0.0132953779643571,0.),.UNSPECIFIED.);
#891=SHAPE_REPRESENTATION_RELATIONSHIP('SRR','None',#105859,#903);
#892=SHAPE_REPRESENTATION_RELATIONSHIP('SRR','None',#105860,#904);
#893=SHAPE_REPRESENTATION_RELATIONSHIP('SRR','None',#105861,#905);
#894=SHAPE_REPRESENTATION_RELATIONSHIP('SRR','None',#105862,#906);
#895=SHAPE_REPRESENTATION_RELATIONSHIP('SRR','None',#105863,#907);
#896=SHAPE_REPRESENTATION_RELATIONSHIP('SRR','None',#105864,#908);
#897=SHAPE_REPRESENTATION_RELATIONSHIP('SRR','None',#105865,#909);
#898=SHAPE_REPRESENTATION_RELATIONSHIP('SRR','None',#105866,#910);
#899=SHAPE_REPRESENTATION_RELATIONSHIP('SRR','None',#105867,#911);
#900=SHAPE_REPRESENTATION_RELATIONSHIP('SRR','None',#105868,#912);
#901=SHAPE_REPRESENTATION_RELATIONSHIP('SRR','None',#105869,#913);
#902=SHAPE_REPRESENTATION_RELATIONSHIP('SRR','None',#105870,#914);
#903=ADVANCED_BREP_SHAPE_REPRESENTATION('',(#927),#105794);
#904=ADVANCED_BREP_SHAPE_REPRESENTATION('',(#928),#105795);
#905=ADVANCED_BREP_SHAPE_REPRESENTATION('',(#929),#105796);
#906=ADVANCED_BREP_SHAPE_REPRESENTATION('',(#930),#105797);
#907=ADVANCED_BREP_SHAPE_REPRESENTATION('',(#931),#105798);
#908=ADVANCED_BREP_SHAPE_REPRESENTATION('',(#932),#105799);
#909=ADVANCED_BREP_SHAPE_REPRESENTATION('',(#933),#105800);
#910=ADVANCED_BREP_SHAPE_REPRESENTATION('',(#934),#105801);
#911=ADVANCED_BREP_SHAPE_REPRESENTATION('',(#935),#105802);
#912=ADVANCED_BREP_SHAPE_REPRESENTATION('',(#936),#105803);
#913=ADVANCED_BREP_SHAPE_REPRESENTATION('',(#937),#105804);
#914=ADVANCED_BREP_SHAPE_REPRESENTATION('',(#938),#105805);
#915=STYLED_ITEM('',(#105928),#927);
#916=STYLED_ITEM('',(#105929),#928);
#917=STYLED_ITEM('',(#105930),#929);
#918=STYLED_ITEM('',(#105931),#930);
#919=STYLED_ITEM('',(#105932),#931);
#920=STYLED_ITEM('',(#105931),#932);
#921=STYLED_ITEM('',(#105930),#933);
#922=STYLED_ITEM('',(#105928),#934);
#923=STYLED_ITEM('',(#105932),#935);
#924=STYLED_ITEM('',(#105930),#936);
#925=STYLED_ITEM('',(#105930),#937);
#926=STYLED_ITEM('',(#105932),#938);
#927=MANIFOLD_SOLID_BREP('Body1',#7202);
#928=MANIFOLD_SOLID_BREP('Body1',#7203);
#929=MANIFOLD_SOLID_BREP('Body1',#7204);
#930=MANIFOLD_SOLID_BREP('Body1',#7205);
#931=MANIFOLD_SOLID_BREP('Body1',#7206);
#932=MANIFOLD_SOLID_BREP('Body1',#7207);
#933=MANIFOLD_SOLID_BREP('Body1',#7208);
#934=MANIFOLD_SOLID_BREP('Body1',#7209);
#935=MANIFOLD_SOLID_BREP('Body1',#7210);
#936=MANIFOLD_SOLID_BREP('Body1',#7211);
#937=MANIFOLD_SOLID_BREP('Body1',#7212);
#938=MANIFOLD_SOLID_BREP('Body1',#7213);
#939=FACE_BOUND('',#1346,.T.);
#940=FACE_BOUND('',#1347,.T.);
#941=FACE_BOUND('',#1348,.T.);
#942=FACE_BOUND('',#1349,.T.);
#943=FACE_BOUND('',#1351,.T.);
#944=FACE_BOUND('',#1352,.T.);
#945=FACE_BOUND('',#1353,.T.);
#946=FACE_BOUND('',#1354,.T.);
#947=FACE_BOUND('',#1365,.T.);
#948=FACE_BOUND('',#1366,.T.);
#949=FACE_BOUND('',#1367,.T.);
#950=FACE_BOUND('',#1368,.T.);
#951=FACE_BOUND('',#1369,.T.);
#952=FACE_BOUND('',#1371,.T.);
#953=FACE_BOUND('',#1372,.T.);
#954=FACE_BOUND('',#1373,.T.);
#955=FACE_BOUND('',#1374,.T.);
#956=FACE_BOUND('',#1375,.T.);
#957=FACE_BOUND('',#1379,.T.);
#958=FACE_BOUND('',#1381,.T.);
#959=FACE_BOUND('',#1463,.T.);
#960=FACE_BOUND('',#1465,.T.);
#961=FACE_BOUND('',#1470,.T.);
#962=FACE_BOUND('',#1473,.T.);
#963=FACE_BOUND('',#1489,.T.);
#964=FACE_BOUND('',#1490,.T.);
#965=FACE_BOUND('',#1491,.T.);
#966=FACE_BOUND('',#1492,.T.);
#967=FACE_BOUND('',#1493,.T.);
#968=FACE_BOUND('',#1496,.T.);
#969=FACE_BOUND('',#1497,.T.);
#970=FACE_BOUND('',#1498,.T.);
#971=FACE_BOUND('',#1499,.T.);
#972=FACE_BOUND('',#1500,.T.);
#973=FACE_BOUND('',#1534,.T.);
#974=FACE_BOUND('',#1535,.T.);
#975=FACE_BOUND('',#1536,.T.);
#976=FACE_BOUND('',#1537,.T.);
#977=FACE_BOUND('',#1538,.T.);
#978=FACE_BOUND('',#1546,.T.);
#979=FACE_BOUND('',#1547,.T.);
#980=FACE_BOUND('',#1548,.T.);
#981=FACE_BOUND('',#1549,.T.);
#982=FACE_BOUND('',#1550,.T.);
#983=FACE_BOUND('',#1582,.T.);
#984=FACE_BOUND('',#1583,.T.);
#985=FACE_BOUND('',#1584,.T.);
#986=FACE_BOUND('',#1593,.T.);
#987=FACE_BOUND('',#1594,.T.);
#988=FACE_BOUND('',#1595,.T.);
#989=FACE_BOUND('',#1598,.T.);
#990=FACE_BOUND('',#1600,.T.);
#991=FACE_BOUND('',#1603,.T.);
#992=FACE_BOUND('',#1617,.T.);
#993=FACE_BOUND('',#1619,.T.);
#994=FACE_BOUND('',#1623,.T.);
#995=FACE_BOUND('',#1625,.T.);
#996=FACE_BOUND('',#1663,.T.);
#997=FACE_BOUND('',#1666,.T.);
#998=PLANE('',#7361);
#999=PLANE('',#7362);
#1000=PLANE('',#7363);
#1001=PLANE('',#7364);
#1002=PLANE('',#7365);
#1003=PLANE('',#7366);
#1004=PLANE('',#7383);
#1005=PLANE('',#7384);
#1006=PLANE('',#7385);
#1007=PLANE('',#7386);
#1008=PLANE('',#7387);
#1009=PLANE('',#7388);
#1010=PLANE('',#7396);
#1011=PLANE('',#7397);
#1012=PLANE('',#7485);
#1013=PLANE('',#7487);
#1014=PLANE('',#7493);
#1015=PLANE('',#7494);
#1016=PLANE('',#7501);
#1017=PLANE('',#7515);
#1018=PLANE('',#7516);
#1019=PLANE('',#7517);
#1020=PLANE('',#7518);
#1021=PLANE('',#7519);
#1022=PLANE('',#7520);
#1023=PLANE('',#7521);
#1024=PLANE('',#7522);
#1025=PLANE('',#7526);
#1026=PLANE('',#7528);
#1027=PLANE('',#7529);
#1028=PLANE('',#7530);
#1029=PLANE('',#7537);
#1030=PLANE('',#7571);
#1031=PLANE('',#7578);
#1032=PLANE('',#7579);
#1033=PLANE('',#7580);
#1034=PLANE('',#7581);
#1035=PLANE('',#7582);
#1036=PLANE('',#7620);
#1037=PLANE('',#7624);
#1038=PLANE('',#7625);
#1039=PLANE('',#7626);
#1040=PLANE('',#7627);
#1041=PLANE('',#7628);
#1042=PLANE('',#7633);
#1043=PLANE('',#7635);
#1044=PLANE('',#7639);
#1045=PLANE('',#7644);
#1046=PLANE('',#7646);
#1047=PLANE('',#7648);
#1048=PLANE('',#7649);
#1049=PLANE('',#7650);
#1050=PLANE('',#7657);
#1051=PLANE('',#7665);
#1052=PLANE('',#7666);
#1053=PLANE('',#7674);
#1054=PLANE('',#7675);
#1055=PLANE('',#7709);
#1056=PLANE('',#7710);
#1057=PLANE('',#7711);
#1058=PLANE('',#7712);
#1059=PLANE('',#7713);
#1060=PLANE('',#7714);
#1061=PLANE('',#7715);
#1062=PLANE('',#7716);
#1063=PLANE('',#7720);
#1064=PLANE('',#7721);
#1065=FACE_OUTER_BOUND('',#1337,.T.);
#1066=FACE_OUTER_BOUND('',#1338,.T.);
#1067=FACE_OUTER_BOUND('',#1339,.T.);
#1068=FACE_OUTER_BOUND('',#1340,.T.);
#1069=FACE_OUTER_BOUND('',#1341,.T.);
#1070=FACE_OUTER_BOUND('',#1342,.T.);
#1071=FACE_OUTER_BOUND('',#1343,.T.);
#1072=FACE_OUTER_BOUND('',#1344,.T.);
#1073=FACE_OUTER_BOUND('',#1345,.T.);
#1074=FACE_OUTER_BOUND('',#1350,.T.);
#1075=FACE_OUTER_BOUND('',#1355,.T.);
#1076=FACE_OUTER_BOUND('',#1356,.T.);
#1077=FACE_OUTER_BOUND('',#1357,.T.);
#1078=FACE_OUTER_BOUND('',#1358,.T.);
#1079=FACE_OUTER_BOUND('',#1359,.T.);
#1080=FACE_OUTER_BOUND('',#1360,.T.);
#1081=FACE_OUTER_BOUND('',#1361,.T.);
#1082=FACE_OUTER_BOUND('',#1362,.T.);
#1083=FACE_OUTER_BOUND('',#1363,.T.);
#1084=FACE_OUTER_BOUND('',#1364,.T.);
#1085=FACE_OUTER_BOUND('',#1370,.T.);
#1086=FACE_OUTER_BOUND('',#1376,.T.);
#1087=FACE_OUTER_BOUND('',#1377,.T.);
#1088=FACE_OUTER_BOUND('',#1378,.T.);
#1089=FACE_OUTER_BOUND('',#1380,.T.);
#1090=FACE_OUTER_BOUND('',#1382,.T.);
#1091=FACE_OUTER_BOUND('',#1383,.T.);
#1092=FACE_OUTER_BOUND('',#1384,.T.);
#1093=FACE_OUTER_BOUND('',#1385,.T.);
#1094=FACE_OUTER_BOUND('',#1386,.T.);
#1095=FACE_OUTER_BOUND('',#1387,.T.);
#1096=FACE_OUTER_BOUND('',#1388,.T.);
#1097=FACE_OUTER_BOUND('',#1389,.T.);
#1098=FACE_OUTER_BOUND('',#1390,.T.);
#1099=FACE_OUTER_BOUND('',#1391,.T.);
#1100=FACE_OUTER_BOUND('',#1392,.T.);
#1101=FACE_OUTER_BOUND('',#1393,.T.);
#1102=FACE_OUTER_BOUND('',#1394,.T.);
#1103=FACE_OUTER_BOUND('',#1395,.T.);
#1104=FACE_OUTER_BOUND('',#1396,.T.);
#1105=FACE_OUTER_BOUND('',#1397,.T.);
#1106=FACE_OUTER_BOUND('',#1398,.T.);
#1107=FACE_OUTER_BOUND('',#1399,.T.);
#1108=FACE_OUTER_BOUND('',#1400,.T.);
#1109=FACE_OUTER_BOUND('',#1401,.T.);
#1110=FACE_OUTER_BOUND('',#1402,.T.);
#1111=FACE_OUTER_BOUND('',#1403,.T.);
#1112=FACE_OUTER_BOUND('',#1404,.T.);
#1113=FACE_OUTER_BOUND('',#1405,.T.);
#1114=FACE_OUTER_BOUND('',#1406,.T.);
#1115=FACE_OUTER_BOUND('',#1407,.T.);
#1116=FACE_OUTER_BOUND('',#1408,.T.);
#1117=FACE_OUTER_BOUND('',#1409,.T.);
#1118=FACE_OUTER_BOUND('',#1410,.T.);
#1119=FACE_OUTER_BOUND('',#1411,.T.);
#1120=FACE_OUTER_BOUND('',#1412,.T.);
#1121=FACE_OUTER_BOUND('',#1413,.T.);
#1122=FACE_OUTER_BOUND('',#1414,.T.);
#1123=FACE_OUTER_BOUND('',#1415,.T.);
#1124=FACE_OUTER_BOUND('',#1416,.T.);
#1125=FACE_OUTER_BOUND('',#1417,.T.);
#1126=FACE_OUTER_BOUND('',#1418,.T.);
#1127=FACE_OUTER_BOUND('',#1419,.T.);
#1128=FACE_OUTER_BOUND('',#1420,.T.);
#1129=FACE_OUTER_BOUND('',#1421,.T.);
#1130=FACE_OUTER_BOUND('',#1422,.T.);
#1131=FACE_OUTER_BOUND('',#1423,.T.);
#1132=FACE_OUTER_BOUND('',#1424,.T.);
#1133=FACE_OUTER_BOUND('',#1425,.T.);
#1134=FACE_OUTER_BOUND('',#1426,.T.);
#1135=FACE_OUTER_BOUND('',#1427,.T.);
#1136=FACE_OUTER_BOUND('',#1428,.T.);
#1137=FACE_OUTER_BOUND('',#1429,.T.);
#1138=FACE_OUTER_BOUND('',#1430,.T.);
#1139=FACE_OUTER_BOUND('',#1431,.T.);
#1140=FACE_OUTER_BOUND('',#1432,.T.);
#1141=FACE_OUTER_BOUND('',#1433,.T.);
#1142=FACE_OUTER_BOUND('',#1434,.T.);
#1143=FACE_OUTER_BOUND('',#1435,.T.);
#1144=FACE_OUTER_BOUND('',#1436,.T.);
#1145=FACE_OUTER_BOUND('',#1437,.T.);
#1146=FACE_OUTER_BOUND('',#1438,.T.);
#1147=FACE_OUTER_BOUND('',#1439,.T.);
#1148=FACE_OUTER_BOUND('',#1440,.T.);
#1149=FACE_OUTER_BOUND('',#1441,.T.);
#1150=FACE_OUTER_BOUND('',#1442,.T.);
#1151=FACE_OUTER_BOUND('',#1443,.T.);
#1152=FACE_OUTER_BOUND('',#1444,.T.);
#1153=FACE_OUTER_BOUND('',#1445,.T.);
#1154=FACE_OUTER_BOUND('',#1446,.T.);
#1155=FACE_OUTER_BOUND('',#1447,.T.);
#1156=FACE_OUTER_BOUND('',#1448,.T.);
#1157=FACE_OUTER_BOUND('',#1449,.T.);
#1158=FACE_OUTER_BOUND('',#1450,.T.);
#1159=FACE_OUTER_BOUND('',#1451,.T.);
#1160=FACE_OUTER_BOUND('',#1452,.T.);
#1161=FACE_OUTER_BOUND('',#1453,.T.);
#1162=FACE_OUTER_BOUND('',#1454,.T.);
#1163=FACE_OUTER_BOUND('',#1455,.T.);
#1164=FACE_OUTER_BOUND('',#1456,.T.);
#1165=FACE_OUTER_BOUND('',#1457,.T.);
#1166=FACE_OUTER_BOUND('',#1458,.T.);
#1167=FACE_OUTER_BOUND('',#1459,.T.);
#1168=FACE_OUTER_BOUND('',#1460,.T.);
#1169=FACE_OUTER_BOUND('',#1461,.T.);
#1170=FACE_OUTER_BOUND('',#1462,.T.);
#1171=FACE_OUTER_BOUND('',#1464,.T.);
#1172=FACE_OUTER_BOUND('',#1466,.T.);
#1173=FACE_OUTER_BOUND('',#1467,.T.);
#1174=FACE_OUTER_BOUND('',#1468,.T.);
#1175=FACE_OUTER_BOUND('',#1469,.T.);
#1176=FACE_OUTER_BOUND('',#1471,.T.);
#1177=FACE_OUTER_BOUND('',#1472,.T.);
#1178=FACE_OUTER_BOUND('',#1474,.T.);
#1179=FACE_OUTER_BOUND('',#1475,.T.);
#1180=FACE_OUTER_BOUND('',#1476,.T.);
#1181=FACE_OUTER_BOUND('',#1477,.T.);
#1182=FACE_OUTER_BOUND('',#1478,.T.);
#1183=FACE_OUTER_BOUND('',#1479,.T.);
#1184=FACE_OUTER_BOUND('',#1480,.T.);
#1185=FACE_OUTER_BOUND('',#1481,.T.);
#1186=FACE_OUTER_BOUND('',#1482,.T.);
#1187=FACE_OUTER_BOUND('',#1483,.T.);
#1188=FACE_OUTER_BOUND('',#1484,.T.);
#1189=FACE_OUTER_BOUND('',#1485,.T.);
#1190=FACE_OUTER_BOUND('',#1486,.T.);
#1191=FACE_OUTER_BOUND('',#1487,.T.);
#1192=FACE_OUTER_BOUND('',#1488,.T.);
#1193=FACE_OUTER_BOUND('',#1494,.T.);
#1194=FACE_OUTER_BOUND('',#1495,.T.);
#1195=FACE_OUTER_BOUND('',#1501,.T.);
#1196=FACE_OUTER_BOUND('',#1502,.T.);
#1197=FACE_OUTER_BOUND('',#1503,.T.);
#1198=FACE_OUTER_BOUND('',#1504,.T.);
#1199=FACE_OUTER_BOUND('',#1505,.T.);
#1200=FACE_OUTER_BOUND('',#1506,.T.);
#1201=FACE_OUTER_BOUND('',#1507,.T.);
#1202=FACE_OUTER_BOUND('',#1508,.T.);
#1203=FACE_OUTER_BOUND('',#1509,.T.);
#1204=FACE_OUTER_BOUND('',#1510,.T.);
#1205=FACE_OUTER_BOUND('',#1511,.T.);
#1206=FACE_OUTER_BOUND('',#1512,.T.);
#1207=FACE_OUTER_BOUND('',#1513,.T.);
#1208=FACE_OUTER_BOUND('',#1514,.T.);
#1209=FACE_OUTER_BOUND('',#1515,.T.);
#1210=FACE_OUTER_BOUND('',#1516,.T.);
#1211=FACE_OUTER_BOUND('',#1517,.T.);
#1212=FACE_OUTER_BOUND('',#1518,.T.);
#1213=FACE_OUTER_BOUND('',#1519,.T.);
#1214=FACE_OUTER_BOUND('',#1520,.T.);
#1215=FACE_OUTER_BOUND('',#1521,.T.);
#1216=FACE_OUTER_BOUND('',#1522,.T.);
#1217=FACE_OUTER_BOUND('',#1523,.T.);
#1218=FACE_OUTER_BOUND('',#1524,.T.);
#1219=FACE_OUTER_BOUND('',#1525,.T.);
#1220=FACE_OUTER_BOUND('',#1526,.T.);
#1221=FACE_OUTER_BOUND('',#1527,.T.);
#1222=FACE_OUTER_BOUND('',#1528,.T.);
#1223=FACE_OUTER_BOUND('',#1529,.T.);
#1224=FACE_OUTER_BOUND('',#1530,.T.);
#1225=FACE_OUTER_BOUND('',#1531,.T.);
#1226=FACE_OUTER_BOUND('',#1532,.T.);
#1227=FACE_OUTER_BOUND('',#1533,.T.);
#1228=FACE_OUTER_BOUND('',#1539,.T.);
#1229=FACE_OUTER_BOUND('',#1540,.T.);
#1230=FACE_OUTER_BOUND('',#1541,.T.);
#1231=FACE_OUTER_BOUND('',#1542,.T.);
#1232=FACE_OUTER_BOUND('',#1543,.T.);
#1233=FACE_OUTER_BOUND('',#1544,.T.);
#1234=FACE_OUTER_BOUND('',#1545,.T.);
#1235=FACE_OUTER_BOUND('',#1551,.T.);
#1236=FACE_OUTER_BOUND('',#1552,.T.);
#1237=FACE_OUTER_BOUND('',#1553,.T.);
#1238=FACE_OUTER_BOUND('',#1554,.T.);
#1239=FACE_OUTER_BOUND('',#1555,.T.);
#1240=FACE_OUTER_BOUND('',#1556,.T.);
#1241=FACE_OUTER_BOUND('',#1557,.T.);
#1242=FACE_OUTER_BOUND('',#1558,.T.);
#1243=FACE_OUTER_BOUND('',#1559,.T.);
#1244=FACE_OUTER_BOUND('',#1560,.T.);
#1245=FACE_OUTER_BOUND('',#1561,.T.);
#1246=FACE_OUTER_BOUND('',#1562,.T.);
#1247=FACE_OUTER_BOUND('',#1563,.T.);
#1248=FACE_OUTER_BOUND('',#1564,.T.);
#1249=FACE_OUTER_BOUND('',#1565,.T.);
#1250=FACE_OUTER_BOUND('',#1566,.T.);
#1251=FACE_OUTER_BOUND('',#1567,.T.);
#1252=FACE_OUTER_BOUND('',#1568,.T.);
#1253=FACE_OUTER_BOUND('',#1569,.T.);
#1254=FACE_OUTER_BOUND('',#1570,.T.);
#1255=FACE_OUTER_BOUND('',#1571,.T.);
#1256=FACE_OUTER_BOUND('',#1572,.T.);
#1257=FACE_OUTER_BOUND('',#1573,.T.);
#1258=FACE_OUTER_BOUND('',#1574,.T.);
#1259=FACE_OUTER_BOUND('',#1575,.T.);
#1260=FACE_OUTER_BOUND('',#1576,.T.);
#1261=FACE_OUTER_BOUND('',#1577,.T.);
#1262=FACE_OUTER_BOUND('',#1578,.T.);
#1263=FACE_OUTER_BOUND('',#1579,.T.);
#1264=FACE_OUTER_BOUND('',#1580,.T.);
#1265=FACE_OUTER_BOUND('',#1581,.T.);
#1266=FACE_OUTER_BOUND('',#1585,.T.);
#1267=FACE_OUTER_BOUND('',#1586,.T.);
#1268=FACE_OUTER_BOUND('',#1587,.T.);
#1269=FACE_OUTER_BOUND('',#1588,.T.);
#1270=FACE_OUTER_BOUND('',#1589,.T.);
#1271=FACE_OUTER_BOUND('',#1590,.T.);
#1272=FACE_OUTER_BOUND('',#1591,.T.);
#1273=FACE_OUTER_BOUND('',#1592,.T.);
#1274=FACE_OUTER_BOUND('',#1596,.T.);
#1275=FACE_OUTER_BOUND('',#1597,.T.);
#1276=FACE_OUTER_BOUND('',#1599,.T.);
#1277=FACE_OUTER_BOUND('',#1601,.T.);
#1278=FACE_OUTER_BOUND('',#1602,.T.);
#1279=FACE_OUTER_BOUND('',#1604,.T.);
#1280=FACE_OUTER_BOUND('',#1605,.T.);
#1281=FACE_OUTER_BOUND('',#1606,.T.);
#1282=FACE_OUTER_BOUND('',#1607,.T.);
#1283=FACE_OUTER_BOUND('',#1608,.T.);
#1284=FACE_OUTER_BOUND('',#1609,.T.);
#1285=FACE_OUTER_BOUND('',#1610,.T.);
#1286=FACE_OUTER_BOUND('',#1611,.T.);
#1287=FACE_OUTER_BOUND('',#1612,.T.);
#1288=FACE_OUTER_BOUND('',#1613,.T.);
#1289=FACE_OUTER_BOUND('',#1614,.T.);
#1290=FACE_OUTER_BOUND('',#1615,.T.);
#1291=FACE_OUTER_BOUND('',#1616,.T.);
#1292=FACE_OUTER_BOUND('',#1618,.T.);
#1293=FACE_OUTER_BOUND('',#1620,.T.);
#1294=FACE_OUTER_BOUND('',#1621,.T.);
#1295=FACE_OUTER_BOUND('',#1622,.T.);
#1296=FACE_OUTER_BOUND('',#1624,.T.);
#1297=FACE_OUTER_BOUND('',#1626,.T.);
#1298=FACE_OUTER_BOUND('',#1627,.T.);
#1299=FACE_OUTER_BOUND('',#1628,.T.);
#1300=FACE_OUTER_BOUND('',#1629,.T.);
#1301=FACE_OUTER_BOUND('',#1630,.T.);
#1302=FACE_OUTER_BOUND('',#1631,.T.);
#1303=FACE_OUTER_BOUND('',#1632,.T.);
#1304=FACE_OUTER_BOUND('',#1633,.T.);
#1305=FACE_OUTER_BOUND('',#1634,.T.);
#1306=FACE_OUTER_BOUND('',#1635,.T.);
#1307=FACE_OUTER_BOUND('',#1636,.T.);
#1308=FACE_OUTER_BOUND('',#1637,.T.);
#1309=FACE_OUTER_BOUND('',#1638,.T.);
#1310=FACE_OUTER_BOUND('',#1639,.T.);
#1311=FACE_OUTER_BOUND('',#1640,.T.);
#1312=FACE_OUTER_BOUND('',#1641,.T.);
#1313=FACE_OUTER_BOUND('',#1642,.T.);
#1314=FACE_OUTER_BOUND('',#1643,.T.);
#1315=FACE_OUTER_BOUND('',#1644,.T.);
#1316=FACE_OUTER_BOUND('',#1645,.T.);
#1317=FACE_OUTER_BOUND('',#1646,.T.);
#1318=FACE_OUTER_BOUND('',#1647,.T.);
#1319=FACE_OUTER_BOUND('',#1648,.T.);
#1320=FACE_OUTER_BOUND('',#1649,.T.);
#1321=FACE_OUTER_BOUND('',#1650,.T.);
#1322=FACE_OUTER_BOUND('',#1651,.T.);
#1323=FACE_OUTER_BOUND('',#1652,.T.);
#1324=FACE_OUTER_BOUND('',#1653,.T.);
#1325=FACE_OUTER_BOUND('',#1654,.T.);
#1326=FACE_OUTER_BOUND('',#1655,.T.);
#1327=FACE_OUTER_BOUND('',#1656,.T.);
#1328=FACE_OUTER_BOUND('',#1657,.T.);
#1329=FACE_OUTER_BOUND('',#1658,.T.);
#1330=FACE_OUTER_BOUND('',#1659,.T.);
#1331=FACE_OUTER_BOUND('',#1660,.T.);
#1332=FACE_OUTER_BOUND('',#1661,.T.);
#1333=FACE_OUTER_BOUND('',#1662,.T.);
#1334=FACE_OUTER_BOUND('',#1664,.T.);
#1335=FACE_OUTER_BOUND('',#1665,.T.);
#1336=FACE_OUTER_BOUND('',#1667,.T.);
#1337=EDGE_LOOP('',(#4413,#4414,#4415,#4416));
#1338=EDGE_LOOP('',(#4417,#4418,#4419,#4420));
#1339=EDGE_LOOP('',(#4421,#4422,#4423,#4424));
#1340=EDGE_LOOP('',(#4425,#4426,#4427,#4428));
#1341=EDGE_LOOP('',(#4429,#4430,#4431,#4432));
#1342=EDGE_LOOP('',(#4433,#4434,#4435,#4436));
#1343=EDGE_LOOP('',(#4437,#4438,#4439,#4440));
#1344=EDGE_LOOP('',(#4441,#4442,#4443,#4444));
#1345=EDGE_LOOP('',(#4445,#4446,#4447,#4448));
#1346=EDGE_LOOP('',(#4449));
#1347=EDGE_LOOP('',(#4450));
#1348=EDGE_LOOP('',(#4451));
#1349=EDGE_LOOP('',(#4452));
#1350=EDGE_LOOP('',(#4453,#4454,#4455,#4456));
#1351=EDGE_LOOP('',(#4457));
#1352=EDGE_LOOP('',(#4458));
#1353=EDGE_LOOP('',(#4459));
#1354=EDGE_LOOP('',(#4460));
#1355=EDGE_LOOP('',(#4461,#4462,#4463,#4464));
#1356=EDGE_LOOP('',(#4465,#4466,#4467,#4468));
#1357=EDGE_LOOP('',(#4469,#4470,#4471,#4472));
#1358=EDGE_LOOP('',(#4473,#4474,#4475,#4476));
#1359=EDGE_LOOP('',(#4477,#4478,#4479,#4480));
#1360=EDGE_LOOP('',(#4481,#4482,#4483,#4484));
#1361=EDGE_LOOP('',(#4485,#4486,#4487,#4488));
#1362=EDGE_LOOP('',(#4489,#4490,#4491,#4492));
#1363=EDGE_LOOP('',(#4493,#4494,#4495,#4496));
#1364=EDGE_LOOP('',(#4497,#4498,#4499,#4500));
#1365=EDGE_LOOP('',(#4501));
#1366=EDGE_LOOP('',(#4502));
#1367=EDGE_LOOP('',(#4503));
#1368=EDGE_LOOP('',(#4504));
#1369=EDGE_LOOP('',(#4505));
#1370=EDGE_LOOP('',(#4506,#4507,#4508,#4509));
#1371=EDGE_LOOP('',(#4510));
#1372=EDGE_LOOP('',(#4511));
#1373=EDGE_LOOP('',(#4512));
#1374=EDGE_LOOP('',(#4513));
#1375=EDGE_LOOP('',(#4514));
#1376=EDGE_LOOP('',(#4515,#4516,#4517,#4518));
#1377=EDGE_LOOP('',(#4519,#4520,#4521,#4522));
#1378=EDGE_LOOP('',(#4523));
#1379=EDGE_LOOP('',(#4524));
#1380=EDGE_LOOP('',(#4525));
#1381=EDGE_LOOP('',(#4526));
#1382=EDGE_LOOP('',(#4527,#4528,#4529,#4530));
#1383=EDGE_LOOP('',(#4531,#4532,#4533,#4534,#4535,#4536));
#1384=EDGE_LOOP('',(#4537,#4538,#4539,#4540,#4541,#4542));
#1385=EDGE_LOOP('',(#4543,#4544,#4545,#4546,#4547,#4548));
#1386=EDGE_LOOP('',(#4549,#4550,#4551,#4552,#4553,#4554));
#1387=EDGE_LOOP('',(#4555,#4556,#4557,#4558,#4559,#4560));
#1388=EDGE_LOOP('',(#4561,#4562,#4563,#4564,#4565,#4566));
#1389=EDGE_LOOP('',(#4567,#4568,#4569,#4570,#4571,#4572));
#1390=EDGE_LOOP('',(#4573,#4574,#4575,#4576,#4577,#4578));
#1391=EDGE_LOOP('',(#4579,#4580,#4581,#4582,#4583,#4584));
#1392=EDGE_LOOP('',(#4585,#4586,#4587,#4588,#4589,#4590));
#1393=EDGE_LOOP('',(#4591,#4592,#4593,#4594,#4595,#4596));
#1394=EDGE_LOOP('',(#4597,#4598,#4599,#4600,#4601,#4602));
#1395=EDGE_LOOP('',(#4603,#4604,#4605,#4606,#4607,#4608));
#1396=EDGE_LOOP('',(#4609,#4610,#4611,#4612,#4613,#4614));
#1397=EDGE_LOOP('',(#4615,#4616,#4617,#4618,#4619,#4620));
#1398=EDGE_LOOP('',(#4621,#4622,#4623,#4624,#4625,#4626));
#1399=EDGE_LOOP('',(#4627,#4628,#4629,#4630,#4631,#4632));
#1400=EDGE_LOOP('',(#4633,#4634,#4635,#4636,#4637,#4638));
#1401=EDGE_LOOP('',(#4639,#4640,#4641,#4642,#4643,#4644));
#1402=EDGE_LOOP('',(#4645,#4646,#4647,#4648,#4649,#4650));
#1403=EDGE_LOOP('',(#4651,#4652,#4653,#4654,#4655,#4656));
#1404=EDGE_LOOP('',(#4657,#4658,#4659,#4660,#4661,#4662));
#1405=EDGE_LOOP('',(#4663,#4664,#4665,#4666,#4667,#4668));
#1406=EDGE_LOOP('',(#4669,#4670,#4671,#4672,#4673,#4674));
#1407=EDGE_LOOP('',(#4675,#4676,#4677,#4678,#4679,#4680));
#1408=EDGE_LOOP('',(#4681,#4682,#4683,#4684,#4685,#4686));
#1409=EDGE_LOOP('',(#4687,#4688,#4689,#4690,#4691,#4692));
#1410=EDGE_LOOP('',(#4693,#4694,#4695,#4696,#4697,#4698));
#1411=EDGE_LOOP('',(#4699,#4700,#4701,#4702,#4703,#4704));
#1412=EDGE_LOOP('',(#4705,#4706,#4707,#4708,#4709,#4710));
#1413=EDGE_LOOP('',(#4711,#4712,#4713,#4714,#4715,#4716));
#1414=EDGE_LOOP('',(#4717,#4718,#4719,#4720,#4721,#4722));
#1415=EDGE_LOOP('',(#4723,#4724,#4725,#4726,#4727,#4728));
#1416=EDGE_LOOP('',(#4729,#4730,#4731,#4732,#4733,#4734));
#1417=EDGE_LOOP('',(#4735,#4736,#4737,#4738,#4739,#4740));
#1418=EDGE_LOOP('',(#4741,#4742,#4743,#4744,#4745,#4746));
#1419=EDGE_LOOP('',(#4747,#4748,#4749,#4750,#4751,#4752));
#1420=EDGE_LOOP('',(#4753,#4754,#4755,#4756,#4757,#4758));
#1421=EDGE_LOOP('',(#4759,#4760,#4761,#4762,#4763,#4764));
#1422=EDGE_LOOP('',(#4765,#4766,#4767,#4768,#4769,#4770));
#1423=EDGE_LOOP('',(#4771,#4772,#4773,#4774,#4775,#4776));
#1424=EDGE_LOOP('',(#4777,#4778,#4779,#4780,#4781,#4782));
#1425=EDGE_LOOP('',(#4783,#4784,#4785,#4786,#4787,#4788));
#1426=EDGE_LOOP('',(#4789,#4790,#4791,#4792,#4793,#4794));
#1427=EDGE_LOOP('',(#4795,#4796,#4797,#4798,#4799,#4800));
#1428=EDGE_LOOP('',(#4801,#4802,#4803,#4804,#4805,#4806));
#1429=EDGE_LOOP('',(#4807,#4808,#4809,#4810,#4811,#4812));
#1430=EDGE_LOOP('',(#4813,#4814,#4815,#4816,#4817,#4818));
#1431=EDGE_LOOP('',(#4819,#4820,#4821,#4822,#4823,#4824));
#1432=EDGE_LOOP('',(#4825,#4826,#4827,#4828,#4829,#4830));
#1433=EDGE_LOOP('',(#4831,#4832,#4833,#4834,#4835,#4836));
#1434=EDGE_LOOP('',(#4837,#4838,#4839,#4840,#4841,#4842));
#1435=EDGE_LOOP('',(#4843,#4844,#4845,#4846,#4847,#4848));
#1436=EDGE_LOOP('',(#4849,#4850,#4851,#4852,#4853,#4854));
#1437=EDGE_LOOP('',(#4855,#4856,#4857,#4858,#4859,#4860));
#1438=EDGE_LOOP('',(#4861,#4862,#4863,#4864,#4865,#4866));
#1439=EDGE_LOOP('',(#4867,#4868,#4869,#4870,#4871,#4872));
#1440=EDGE_LOOP('',(#4873,#4874,#4875,#4876,#4877,#4878));
#1441=EDGE_LOOP('',(#4879,#4880,#4881,#4882,#4883,#4884));
#1442=EDGE_LOOP('',(#4885,#4886,#4887,#4888,#4889,#4890));
#1443=EDGE_LOOP('',(#4891,#4892,#4893,#4894,#4895,#4896));
#1444=EDGE_LOOP('',(#4897,#4898,#4899,#4900,#4901,#4902));
#1445=EDGE_LOOP('',(#4903,#4904,#4905,#4906,#4907,#4908));
#1446=EDGE_LOOP('',(#4909,#4910,#4911,#4912,#4913,#4914));
#1447=EDGE_LOOP('',(#4915,#4916,#4917,#4918,#4919,#4920));
#1448=EDGE_LOOP('',(#4921,#4922,#4923,#4924,#4925,#4926));
#1449=EDGE_LOOP('',(#4927,#4928,#4929,#4930,#4931,#4932));
#1450=EDGE_LOOP('',(#4933,#4934,#4935,#4936,#4937,#4938));
#1451=EDGE_LOOP('',(#4939,#4940,#4941,#4942,#4943,#4944));
#1452=EDGE_LOOP('',(#4945,#4946,#4947,#4948,#4949,#4950));
#1453=EDGE_LOOP('',(#4951,#4952,#4953,#4954,#4955,#4956));
#1454=EDGE_LOOP('',(#4957,#4958,#4959,#4960,#4961,#4962));
#1455=EDGE_LOOP('',(#4963,#4964,#4965,#4966,#4967,#4968));
#1456=EDGE_LOOP('',(#4969,#4970,#4971,#4972,#4973,#4974));
#1457=EDGE_LOOP('',(#4975,#4976,#4977,#4978,#4979,#4980));
#1458=EDGE_LOOP('',(#4981,#4982,#4983,#4984,#4985,#4986));
#1459=EDGE_LOOP('',(#4987,#4988,#4989,#4990,#4991,#4992));
#1460=EDGE_LOOP('',(#4993,#4994,#4995,#4996,#4997,#4998,#4999,#5000,#5001,
#5002,#5003,#5004,#5005,#5006,#5007,#5008,#5009,#5010,#5011,#5012,#5013,
#5014,#5015,#5016,#5017,#5018,#5019,#5020,#5021,#5022,#5023,#5024,#5025,
#5026,#5027,#5028,#5029,#5030,#5031,#5032,#5033,#5034,#5035,#5036,#5037,
#5038,#5039,#5040,#5041,#5042,#5043,#5044,#5045,#5046,#5047,#5048,#5049,
#5050,#5051,#5052,#5053,#5054,#5055,#5056,#5057,#5058,#5059,#5060,#5061,
#5062,#5063,#5064,#5065,#5066,#5067,#5068,#5069,#5070,#5071,#5072,#5073,
#5074,#5075,#5076,#5077,#5078,#5079,#5080,#5081,#5082,#5083,#5084,#5085,
#5086,#5087,#5088,#5089,#5090,#5091,#5092,#5093,#5094,#5095,#5096,#5097,
#5098,#5099,#5100,#5101,#5102,#5103,#5104,#5105,#5106,#5107,#5108,#5109,
#5110,#5111,#5112,#5113,#5114,#5115,#5116,#5117,#5118,#5119,#5120,#5121,
#5122,#5123,#5124,#5125,#5126,#5127,#5128,#5129,#5130,#5131,#5132,#5133,
#5134,#5135));
#1461=EDGE_LOOP('',(#5136,#5137,#5138,#5139));
#1462=EDGE_LOOP('',(#5140));
#1463=EDGE_LOOP('',(#5141));
#1464=EDGE_LOOP('',(#5142));
#1465=EDGE_LOOP('',(#5143));
#1466=EDGE_LOOP('',(#5144,#5145,#5146,#5147));
#1467=EDGE_LOOP('',(#5148,#5149,#5150,#5151));
#1468=EDGE_LOOP('',(#5152));
#1469=EDGE_LOOP('',(#5153));
#1470=EDGE_LOOP('',(#5154,#5155,#5156,#5157));
#1471=EDGE_LOOP('',(#5158,#5159,#5160,#5161));
#1472=EDGE_LOOP('',(#5162));
#1473=EDGE_LOOP('',(#5163));
#1474=EDGE_LOOP('',(#5164,#5165,#5166,#5167));
#1475=EDGE_LOOP('',(#5168,#5169,#5170,#5171));
#1476=EDGE_LOOP('',(#5172,#5173,#5174,#5175));
#1477=EDGE_LOOP('',(#5176,#5177,#5178,#5179));
#1478=EDGE_LOOP('',(#5180,#5181,#5182,#5183));
#1479=EDGE_LOOP('',(#5184,#5185,#5186,#5187,#5188,#5189,#5190,#5191,#5192,
#5193,#5194,#5195,#5196,#5197,#5198,#5199,#5200,#5201,#5202,#5203,#5204,
#5205,#5206,#5207,#5208,#5209,#5210,#5211,#5212,#5213,#5214,#5215,#5216,
#5217,#5218,#5219,#5220,#5221,#5222,#5223,#5224,#5225,#5226,#5227,#5228,
#5229,#5230,#5231,#5232,#5233,#5234,#5235,#5236,#5237,#5238,#5239,#5240,
#5241,#5242,#5243,#5244,#5245,#5246,#5247,#5248,#5249,#5250,#5251,#5252,
#5253,#5254,#5255,#5256,#5257,#5258,#5259,#5260,#5261,#5262,#5263,#5264,
#5265,#5266,#5267,#5268,#5269,#5270,#5271,#5272,#5273,#5274,#5275,#5276,
#5277,#5278,#5279,#5280,#5281,#5282,#5283,#5284,#5285,#5286,#5287,#5288,
#5289,#5290,#5291,#5292,#5293,#5294,#5295,#5296,#5297,#5298,#5299,#5300,
#5301,#5302,#5303,#5304,#5305,#5306,#5307,#5308,#5309,#5310,#5311,#5312,
#5313,#5314,#5315,#5316,#5317,#5318,#5319,#5320,#5321,#5322,#5323,#5324,
#5325,#5326,#5327,#5328,#5329,#5330,#5331,#5332,#5333,#5334,#5335,#5336,
#5337,#5338,#5339,#5340,#5341,#5342,#5343,#5344,#5345,#5346,#5347,#5348,
#5349,#5350,#5351,#5352,#5353,#5354,#5355,#5356,#5357,#5358,#5359,#5360,
#5361,#5362,#5363,#5364,#5365,#5366,#5367,#5368,#5369,#5370,#5371,#5372,
#5373,#5374,#5375,#5376,#5377,#5378,#5379,#5380,#5381,#5382,#5383,#5384,
#5385,#5386,#5387,#5388,#5389,#5390,#5391,#5392,#5393,#5394,#5395,#5396,
#5397,#5398,#5399,#5400,#5401,#5402,#5403,#5404));
#1480=EDGE_LOOP('',(#5405,#5406,#5407,#5408,#5409,#5410,#5411,#5412,#5413,
#5414,#5415,#5416,#5417,#5418,#5419,#5420,#5421,#5422,#5423,#5424,#5425,
#5426,#5427,#5428,#5429,#5430,#5431,#5432,#5433,#5434,#5435,#5436,#5437,
#5438,#5439,#5440,#5441,#5442,#5443,#5444,#5445,#5446,#5447,#5448,#5449,
#5450,#5451,#5452,#5453,#5454,#5455,#5456,#5457,#5458,#5459,#5460,#5461,
#5462,#5463,#5464,#5465,#5466,#5467,#5468,#5469,#5470,#5471,#5472,#5473,
#5474,#5475,#5476,#5477,#5478,#5479,#5480,#5481,#5482,#5483,#5484,#5485,
#5486,#5487,#5488,#5489,#5490,#5491,#5492,#5493,#5494,#5495,#5496,#5497,
#5498,#5499,#5500,#5501,#5502,#5503,#5504,#5505,#5506,#5507,#5508,#5509,
#5510,#5511,#5512,#5513,#5514,#5515,#5516,#5517,#5518,#5519,#5520,#5521,
#5522,#5523,#5524,#5525,#5526,#5527,#5528,#5529,#5530,#5531,#5532,#5533,
#5534,#5535,#5536,#5537,#5538,#5539,#5540,#5541,#5542,#5543,#5544,#5545,
#5546,#5547,#5548,#5549,#5550,#5551,#5552,#5553,#5554,#5555,#5556,#5557,
#5558,#5559,#5560,#5561,#5562,#5563,#5564,#5565,#5566,#5567,#5568,#5569,
#5570,#5571,#5572,#5573,#5574,#5575,#5576,#5577,#5578,#5579,#5580,#5581,
#5582,#5583,#5584,#5585,#5586,#5587,#5588,#5589,#5590,#5591,#5592,#5593,
#5594,#5595,#5596,#5597,#5598,#5599,#5600,#5601,#5602,#5603,#5604,#5605,
#5606,#5607,#5608,#5609,#5610,#5611,#5612,#5613,#5614,#5615,#5616,#5617,
#5618,#5619,#5620,#5621,#5622,#5623,#5624,#5625,#5626,#5627,#5628,#5629,
#5630,#5631,#5632,#5633,#5634,#5635,#5636,#5637,#5638,#5639,#5640));
#1481=EDGE_LOOP('',(#5641,#5642,#5643,#5644));
#1482=EDGE_LOOP('',(#5645,#5646,#5647,#5648));
#1483=EDGE_LOOP('',(#5649,#5650,#5651,#5652));
#1484=EDGE_LOOP('',(#5653,#5654,#5655,#5656));
#1485=EDGE_LOOP('',(#5657,#5658,#5659,#5660));
#1486=EDGE_LOOP('',(#5661,#5662,#5663,#5664));
#1487=EDGE_LOOP('',(#5665,#5666,#5667,#5668,#5669,#5670));
#1488=EDGE_LOOP('',(#5671));
#1489=EDGE_LOOP('',(#5672,#5673,#5674,#5675));
#1490=EDGE_LOOP('',(#5676));
#1491=EDGE_LOOP('',(#5677));
#1492=EDGE_LOOP('',(#5678));
#1493=EDGE_LOOP('',(#5679));
#1494=EDGE_LOOP('',(#5680,#5681,#5682,#5683));
#1495=EDGE_LOOP('',(#5684));
#1496=EDGE_LOOP('',(#5685,#5686,#5687,#5688,#5689,#5690));
#1497=EDGE_LOOP('',(#5691));
#1498=EDGE_LOOP('',(#5692));
#1499=EDGE_LOOP('',(#5693));
#1500=EDGE_LOOP('',(#5694));
#1501=EDGE_LOOP('',(#5695,#5696,#5697,#5698));
#1502=EDGE_LOOP('',(#5699,#5700,#5701,#5702));
#1503=EDGE_LOOP('',(#5703,#5704,#5705,#5706));
#1504=EDGE_LOOP('',(#5707,#5708,#5709,#5710));
#1505=EDGE_LOOP('',(#5711,#5712,#5713,#5714));
#1506=EDGE_LOOP('',(#5715,#5716,#5717,#5718));
#1507=EDGE_LOOP('',(#5719,#5720,#5721,#5722));
#1508=EDGE_LOOP('',(#5723,#5724,#5725,#5726,#5727,#5728));
#1509=EDGE_LOOP('',(#5729,#5730,#5731,#5732,#5733,#5734));
#1510=EDGE_LOOP('',(#5735,#5736,#5737,#5738,#5739,#5740));
#1511=EDGE_LOOP('',(#5741,#5742,#5743,#5744,#5745,#5746));
#1512=EDGE_LOOP('',(#5747,#5748,#5749,#5750,#5751,#5752));
#1513=EDGE_LOOP('',(#5753,#5754,#5755,#5756,#5757,#5758));
#1514=EDGE_LOOP('',(#5759,#5760,#5761,#5762,#5763,#5764));
#1515=EDGE_LOOP('',(#5765,#5766,#5767,#5768,#5769,#5770));
#1516=EDGE_LOOP('',(#5771,#5772,#5773,#5774,#5775,#5776));
#1517=EDGE_LOOP('',(#5777,#5778,#5779,#5780));
#1518=EDGE_LOOP('',(#5781,#5782,#5783,#5784));
#1519=EDGE_LOOP('',(#5785,#5786,#5787,#5788,#5789,#5790));
#1520=EDGE_LOOP('',(#5791,#5792,#5793,#5794,#5795,#5796));
#1521=EDGE_LOOP('',(#5797,#5798,#5799,#5800,#5801));
#1522=EDGE_LOOP('',(#5802,#5803,#5804,#5805,#5806));
#1523=EDGE_LOOP('',(#5807,#5808,#5809,#5810,#5811,#5812));
#1524=EDGE_LOOP('',(#5813,#5814,#5815,#5816,#5817));
#1525=EDGE_LOOP('',(#5818,#5819,#5820,#5821,#5822,#5823));
#1526=EDGE_LOOP('',(#5824,#5825,#5826,#5827,#5828));
#1527=EDGE_LOOP('',(#5829,#5830,#5831,#5832,#5833));
#1528=EDGE_LOOP('',(#5834,#5835,#5836,#5837,#5838,#5839));
#1529=EDGE_LOOP('',(#5840,#5841,#5842,#5843));
#1530=EDGE_LOOP('',(#5844,#5845,#5846,#5847));
#1531=EDGE_LOOP('',(#5848,#5849,#5850,#5851,#5852,#5853,#5854,#5855,#5856,
#5857,#5858,#5859,#5860,#5861,#5862,#5863,#5864,#5865,#5866,#5867,#5868,
#5869,#5870,#5871,#5872,#5873,#5874,#5875,#5876,#5877,#5878,#5879,#5880,
#5881,#5882,#5883,#5884,#5885,#5886,#5887,#5888,#5889));
#1532=EDGE_LOOP('',(#5890,#5891,#5892,#5893,#5894,#5895,#5896,#5897,#5898,
#5899,#5900,#5901,#5902,#5903,#5904,#5905,#5906,#5907,#5908,#5909,#5910,
#5911,#5912,#5913,#5914,#5915,#5916,#5917,#5918,#5919,#5920,#5921,#5922,
#5923,#5924,#5925,#5926,#5927,#5928,#5929));
#1533=EDGE_LOOP('',(#5930,#5931,#5932,#5933));
#1534=EDGE_LOOP('',(#5934));
#1535=EDGE_LOOP('',(#5935));
#1536=EDGE_LOOP('',(#5936));
#1537=EDGE_LOOP('',(#5937));
#1538=EDGE_LOOP('',(#5938,#5939,#5940,#5941));
#1539=EDGE_LOOP('',(#5942,#5943,#5944,#5945));
#1540=EDGE_LOOP('',(#5946,#5947,#5948,#5949));
#1541=EDGE_LOOP('',(#5950,#5951,#5952,#5953));
#1542=EDGE_LOOP('',(#5954,#5955,#5956,#5957));
#1543=EDGE_LOOP('',(#5958,#5959,#5960,#5961));
#1544=EDGE_LOOP('',(#5962,#5963,#5964,#5965));
#1545=EDGE_LOOP('',(#5966,#5967,#5968,#5969));
#1546=EDGE_LOOP('',(#5970));
#1547=EDGE_LOOP('',(#5971));
#1548=EDGE_LOOP('',(#5972,#5973,#5974,#5975,#5976));
#1549=EDGE_LOOP('',(#5977));
#1550=EDGE_LOOP('',(#5978));
#1551=EDGE_LOOP('',(#5979,#5980,#5981,#5982));
#1552=EDGE_LOOP('',(#5983,#5984,#5985,#5986,#5987,#5988));
#1553=EDGE_LOOP('',(#5989,#5990,#5991,#5992,#5993,#5994));
#1554=EDGE_LOOP('',(#5995,#5996,#5997,#5998,#5999,#6000));
#1555=EDGE_LOOP('',(#6001,#6002,#6003,#6004,#6005,#6006));
#1556=EDGE_LOOP('',(#6007,#6008,#6009,#6010,#6011,#6012));
#1557=EDGE_LOOP('',(#6013,#6014,#6015,#6016));
#1558=EDGE_LOOP('',(#6017,#6018,#6019,#6020,#6021,#6022));
#1559=EDGE_LOOP('',(#6023,#6024,#6025,#6026,#6027,#6028));
#1560=EDGE_LOOP('',(#6029,#6030,#6031,#6032,#6033,#6034));
#1561=EDGE_LOOP('',(#6035,#6036,#6037,#6038,#6039,#6040));
#1562=EDGE_LOOP('',(#6041,#6042,#6043,#6044,#6045,#6046));
#1563=EDGE_LOOP('',(#6047,#6048,#6049,#6050));
#1564=EDGE_LOOP('',(#6051,#6052,#6053,#6054,#6055));
#1565=EDGE_LOOP('',(#6056,#6057,#6058,#6059,#6060,#6061));
#1566=EDGE_LOOP('',(#6062,#6063,#6064,#6065,#6066));
#1567=EDGE_LOOP('',(#6067,#6068,#6069,#6070,#6071,#6072));
#1568=EDGE_LOOP('',(#6073,#6074,#6075,#6076,#6077,#6078));
#1569=EDGE_LOOP('',(#6079,#6080,#6081,#6082));
#1570=EDGE_LOOP('',(#6083,#6084,#6085,#6086,#6087));
#1571=EDGE_LOOP('',(#6088,#6089,#6090,#6091,#6092,#6093));
#1572=EDGE_LOOP('',(#6094,#6095,#6096,#6097,#6098));
#1573=EDGE_LOOP('',(#6099,#6100,#6101,#6102,#6103,#6104));
#1574=EDGE_LOOP('',(#6105,#6106,#6107,#6108,#6109,#6110));
#1575=EDGE_LOOP('',(#6111,#6112,#6113,#6114,#6115,#6116));
#1576=EDGE_LOOP('',(#6117,#6118,#6119,#6120,#6121,#6122));
#1577=EDGE_LOOP('',(#6123,#6124,#6125,#6126,#6127,#6128));
#1578=EDGE_LOOP('',(#6129,#6130,#6131,#6132,#6133,#6134));
#1579=EDGE_LOOP('',(#6135,#6136,#6137,#6138,#6139,#6140,#6141,#6142,#6143,
#6144,#6145,#6146,#6147,#6148,#6149,#6150,#6151,#6152,#6153,#6154,#6155,
#6156,#6157,#6158,#6159,#6160,#6161));
#1580=EDGE_LOOP('',(#6162,#6163,#6164,#6165,#6166,#6167,#6168,#6169,#6170,
#6171,#6172,#6173,#6174,#6175,#6176,#6177,#6178,#6179,#6180,#6181,#6182,
#6183,#6184,#6185,#6186,#6187,#6188,#6189));
#1581=EDGE_LOOP('',(#6190,#6191,#6192,#6193));
#1582=EDGE_LOOP('',(#6194,#6195,#6196,#6197));
#1583=EDGE_LOOP('',(#6198,#6199,#6200,#6201));
#1584=EDGE_LOOP('',(#6202));
#1585=EDGE_LOOP('',(#6203,#6204,#6205,#6206,#6207,#6208,#6209,#6210,#6211,
#6212,#6213,#6214,#6215,#6216,#6217,#6218,#6219,#6220,#6221,#6222,#6223,
#6224,#6225,#6226,#6227,#6228,#6229));
#1586=EDGE_LOOP('',(#6230,#6231,#6232,#6233,#6234,#6235,#6236,#6237,#6238,
#6239,#6240,#6241,#6242,#6243,#6244,#6245,#6246,#6247,#6248,#6249,#6250,
#6251,#6252,#6253,#6254,#6255,#6256,#6257));
#1587=EDGE_LOOP('',(#6258,#6259,#6260,#6261));
#1588=EDGE_LOOP('',(#6262,#6263,#6264,#6265));
#1589=EDGE_LOOP('',(#6266,#6267,#6268,#6269));
#1590=EDGE_LOOP('',(#6270,#6271,#6272,#6273));
#1591=EDGE_LOOP('',(#6274,#6275,#6276,#6277));
#1592=EDGE_LOOP('',(#6278,#6279,#6280,#6281));
#1593=EDGE_LOOP('',(#6282,#6283,#6284,#6285,#6286));
#1594=EDGE_LOOP('',(#6287,#6288,#6289,#6290,#6291));
#1595=EDGE_LOOP('',(#6292));
#1596=EDGE_LOOP('',(#6293,#6294,#6295,#6296));
#1597=EDGE_LOOP('',(#6297));
#1598=EDGE_LOOP('',(#6298));
#1599=EDGE_LOOP('',(#6299));
#1600=EDGE_LOOP('',(#6300));
#1601=EDGE_LOOP('',(#6301,#6302,#6303,#6304));
#1602=EDGE_LOOP('',(#6305));
#1603=EDGE_LOOP('',(#6306));
#1604=EDGE_LOOP('',(#6307,#6308,#6309,#6310));
#1605=EDGE_LOOP('',(#6311));
#1606=EDGE_LOOP('',(#6312,#6313,#6314,#6315));
#1607=EDGE_LOOP('',(#6316));
#1608=EDGE_LOOP('',(#6317,#6318,#6319,#6320));
#1609=EDGE_LOOP('',(#6321,#6322,#6323,#6324));
#1610=EDGE_LOOP('',(#6325,#6326,#6327,#6328));
#1611=EDGE_LOOP('',(#6329,#6330,#6331,#6332));
#1612=EDGE_LOOP('',(#6333,#6334,#6335,#6336));
#1613=EDGE_LOOP('',(#6337,#6338,#6339,#6340));
#1614=EDGE_LOOP('',(#6341,#6342,#6343,#6344));
#1615=EDGE_LOOP('',(#6345,#6346,#6347,#6348));
#1616=EDGE_LOOP('',(#6349));
#1617=EDGE_LOOP('',(#6350));
#1618=EDGE_LOOP('',(#6351));
#1619=EDGE_LOOP('',(#6352));
#1620=EDGE_LOOP('',(#6353,#6354,#6355,#6356));
#1621=EDGE_LOOP('',(#6357,#6358,#6359,#6360));
#1622=EDGE_LOOP('',(#6361));
#1623=EDGE_LOOP('',(#6362));
#1624=EDGE_LOOP('',(#6363));
#1625=EDGE_LOOP('',(#6364));
#1626=EDGE_LOOP('',(#6365,#6366,#6367,#6368));
#1627=EDGE_LOOP('',(#6369,#6370,#6371,#6372,#6373));
#1628=EDGE_LOOP('',(#6374,#6375,#6376,#6377,#6378));
#1629=EDGE_LOOP('',(#6379,#6380,#6381,#6382,#6383));
#1630=EDGE_LOOP('',(#6384,#6385,#6386,#6387,#6388,#6389));
#1631=EDGE_LOOP('',(#6390,#6391,#6392,#6393,#6394));
#1632=EDGE_LOOP('',(#6395,#6396,#6397,#6398,#6399,#6400));
#1633=EDGE_LOOP('',(#6401,#6402,#6403,#6404));
#1634=EDGE_LOOP('',(#6405,#6406,#6407,#6408,#6409,#6410));
#1635=EDGE_LOOP('',(#6411,#6412,#6413,#6414));
#1636=EDGE_LOOP('',(#6415,#6416,#6417,#6418,#6419,#6420));
#1637=EDGE_LOOP('',(#6421,#6422,#6423,#6424,#6425,#6426));
#1638=EDGE_LOOP('',(#6427,#6428,#6429,#6430,#6431));
#1639=EDGE_LOOP('',(#6432,#6433,#6434,#6435,#6436));
#1640=EDGE_LOOP('',(#6437,#6438,#6439,#6440,#6441));
#1641=EDGE_LOOP('',(#6442,#6443,#6444,#6445,#6446));
#1642=EDGE_LOOP('',(#6447,#6448,#6449,#6450,#6451));
#1643=EDGE_LOOP('',(#6452,#6453,#6454,#6455,#6456));
#1644=EDGE_LOOP('',(#6457,#6458,#6459,#6460,#6461,#6462));
#1645=EDGE_LOOP('',(#6463,#6464,#6465,#6466));
#1646=EDGE_LOOP('',(#6467,#6468,#6469,#6470,#6471,#6472));
#1647=EDGE_LOOP('',(#6473,#6474,#6475,#6476));
#1648=EDGE_LOOP('',(#6477,#6478,#6479,#6480,#6481,#6482));
#1649=EDGE_LOOP('',(#6483,#6484,#6485,#6486));
#1650=EDGE_LOOP('',(#6487,#6488,#6489,#6490,#6491,#6492,#6493,#6494,#6495,
#6496,#6497,#6498,#6499,#6500,#6501,#6502,#6503,#6504,#6505,#6506,#6507,
#6508,#6509,#6510,#6511,#6512,#6513,#6514,#6515,#6516,#6517,#6518,#6519,
#6520,#6521,#6522,#6523,#6524,#6525,#6526,#6527,#6528,#6529,#6530,#6531,
#6532,#6533,#6534,#6535,#6536,#6537,#6538));
#1651=EDGE_LOOP('',(#6539,#6540,#6541,#6542,#6543,#6544));
#1652=EDGE_LOOP('',(#6545,#6546,#6547,#6548,#6549,#6550,#6551,#6552,#6553));
#1653=EDGE_LOOP('',(#6554,#6555,#6556,#6557,#6558,#6559,#6560,#6561,#6562,
#6563,#6564,#6565,#6566,#6567,#6568,#6569,#6570,#6571,#6572,#6573,#6574,
#6575,#6576,#6577,#6578,#6579,#6580,#6581,#6582,#6583,#6584,#6585,#6586,
#6587,#6588,#6589,#6590,#6591,#6592,#6593,#6594,#6595,#6596,#6597,#6598,
#6599,#6600,#6601,#6602,#6603,#6604,#6605,#6606,#6607,#6608,#6609,#6610,
#6611,#6612,#6613,#6614,#6615,#6616,#6617,#6618,#6619));
#1654=EDGE_LOOP('',(#6620,#6621,#6622,#6623,#6624,#6625,#6626,#6627,#6628,
#6629,#6630,#6631,#6632,#6633,#6634,#6635,#6636,#6637,#6638,#6639,#6640,
#6641,#6642,#6643,#6644,#6645,#6646,#6647,#6648,#6649,#6650,#6651,#6652,
#6653,#6654,#6655,#6656,#6657,#6658,#6659,#6660,#6661,#6662,#6663,#6664,
#6665,#6666,#6667,#6668,#6669,#6670,#6671,#6672,#6673,#6674,#6675,#6676,
#6677,#6678,#6679,#6680,#6681,#6682,#6683,#6684,#6685,#6686,#6687,#6688));
#1655=EDGE_LOOP('',(#6689,#6690,#6691,#6692));
#1656=EDGE_LOOP('',(#6693,#6694,#6695,#6696));
#1657=EDGE_LOOP('',(#6697,#6698,#6699,#6700));
#1658=EDGE_LOOP('',(#6701,#6702,#6703,#6704));
#1659=EDGE_LOOP('',(#6705,#6706,#6707,#6708));
#1660=EDGE_LOOP('',(#6709,#6710,#6711,#6712));
#1661=EDGE_LOOP('',(#6713,#6714,#6715,#6716,#6717,#6718));
#1662=EDGE_LOOP('',(#6719));
#1663=EDGE_LOOP('',(#6720,#6721,#6722,#6723,#6724));
#1664=EDGE_LOOP('',(#6725,#6726,#6727,#6728));
#1665=EDGE_LOOP('',(#6729));
#1666=EDGE_LOOP('',(#6730,#6731,#6732,#6733,#6734,#6735));
#1667=EDGE_LOOP('',(#6736));
#1668=LINE('',#8821,#1948);
#1669=LINE('',#8827,#1949);
#1670=LINE('',#8833,#1950);
#1671=LINE('',#8839,#1951);
#1672=LINE('',#8844,#1952);
#1673=LINE('',#8846,#1953);
#1674=LINE('',#8848,#1954);
#1675=LINE('',#8849,#1955);
#1676=LINE('',#8852,#1956);
#1677=LINE('',#8854,#1957);
#1678=LINE('',#8855,#1958);
#1679=LINE('',#8858,#1959);
#1680=LINE('',#8860,#1960);
#1681=LINE('',#8861,#1961);
#1682=LINE('',#8863,#1962);
#1683=LINE('',#8864,#1963);
#1684=LINE('',#8872,#1964);
#1685=LINE('',#8878,#1965);
#1686=LINE('',#8884,#1966);
#1687=LINE('',#8890,#1967);
#1688=LINE('',#8896,#1968);
#1689=LINE('',#8901,#1969);
#1690=LINE('',#8903,#1970);
#1691=LINE('',#8905,#1971);
#1692=LINE('',#8906,#1972);
#1693=LINE('',#8909,#1973);
#1694=LINE('',#8911,#1974);
#1695=LINE('',#8912,#1975);
#1696=LINE('',#8915,#1976);
#1697=LINE('',#8917,#1977);
#1698=LINE('',#8918,#1978);
#1699=LINE('',#8920,#1979);
#1700=LINE('',#8921,#1980);
#1701=LINE('',#8929,#1981);
#1702=LINE('',#8935,#1982);
#1703=LINE('',#8943,#1983);
#1704=LINE('',#9159,#1984);
#1705=LINE('',#9655,#1985);
#1706=LINE('',#10157,#1986);
#1707=LINE('',#10668,#1987);
#1708=LINE('',#11161,#1988);
#1709=LINE('',#11654,#1989);
#1710=LINE('',#12153,#1990);
#1711=LINE('',#12652,#1991);
#1712=LINE('',#13142,#1992);
#1713=LINE('',#13629,#1993);
#1714=LINE('',#14134,#1994);
#1715=LINE('',#14639,#1995);
#1716=LINE('',#15141,#1996);
#1717=LINE('',#15637,#1997);
#1718=LINE('',#16130,#1998);
#1719=LINE('',#16620,#1999);
#1720=LINE('',#17122,#2000);
#1721=LINE('',#17636,#2001);
#1722=LINE('',#18135,#2002);
#1723=LINE('',#18622,#2003);
#1724=LINE('',#19115,#2004);
#1725=LINE('',#19623,#2005);
#1726=LINE('',#20122,#2006);
#1727=LINE('',#20624,#2007);
#1728=LINE('',#21111,#2008);
#1729=LINE('',#21595,#2009);
#1730=LINE('',#22097,#2010);
#1731=LINE('',#22605,#2011);
#1732=LINE('',#23113,#2012);
#1733=LINE('',#23597,#2013);
#1734=LINE('',#24090,#2014);
#1735=LINE('',#24601,#2015);
#1736=LINE('',#25112,#2016);
#1737=LINE('',#25608,#2017);
#1738=LINE('',#26089,#2018);
#1739=LINE('',#26588,#2019);
#1740=LINE('',#27087,#2020);
#1741=LINE('',#27583,#2021);
#1742=LINE('',#28100,#2022);
#1743=LINE('',#28584,#2023);
#1744=LINE('',#29077,#2024);
#1745=LINE('',#29579,#2025);
#1746=LINE('',#30078,#2026);
#1747=LINE('',#30565,#2027);
#1748=LINE('',#30898,#2028);
#1749=LINE('',#31336,#2029);
#1750=LINE('',#31832,#2030);
#1751=LINE('',#32334,#2031);
#1752=LINE('',#32836,#2032);
#1753=LINE('',#33338,#2033);
#1754=LINE('',#33834,#2034);
#1755=LINE('',#34336,#2035);
#1756=LINE('',#34838,#2036);
#1757=LINE('',#35325,#2037);
#1758=LINE('',#35830,#2038);
#1759=LINE('',#36332,#2039);
#1760=LINE('',#36822,#2040);
#1761=LINE('',#37309,#2041);
#1762=LINE('',#37811,#2042);
#1763=LINE('',#38322,#2043);
#1764=LINE('',#38818,#2044);
#1765=LINE('',#39308,#2045);
#1766=LINE('',#39798,#2046);
#1767=LINE('',#40297,#2047);
#1768=LINE('',#40796,#2048);
#1769=LINE('',#41289,#2049);
#1770=LINE('',#41782,#2050);
#1771=LINE('',#42287,#2051);
#1772=LINE('',#42780,#2052);
#1773=LINE('',#43288,#2053);
#1774=LINE('',#43787,#2054);
#1775=LINE('',#44274,#2055);
#1776=LINE('',#44773,#2056);
#1777=LINE('',#45269,#2057);
#1778=LINE('',#45771,#2058);
#1779=LINE('',#46273,#2059);
#1780=LINE('',#66984,#2060);
#1781=LINE('',#66995,#2061);
#1782=LINE('',#66998,#2062);
#1783=LINE('',#67012,#2063);
#1784=LINE('',#67018,#2064);
#1785=LINE('',#67024,#2065);
#1786=LINE('',#67030,#2066);
#1787=LINE('',#67036,#2067);
#1788=LINE('',#71828,#2068);
#1789=LINE('',#71830,#2069);
#1790=LINE('',#71832,#2070);
#1791=LINE('',#71833,#2071);
#1792=LINE('',#71836,#2072);
#1793=LINE('',#71838,#2073);
#1794=LINE('',#71839,#2074);
#1795=LINE('',#71842,#2075);
#1796=LINE('',#71844,#2076);
#1797=LINE('',#71845,#2077);
#1798=LINE('',#71848,#2078);
#1799=LINE('',#71850,#2079);
#1800=LINE('',#71851,#2080);
#1801=LINE('',#71854,#2081);
#1802=LINE('',#71856,#2082);
#1803=LINE('',#71857,#2083);
#1804=LINE('',#71859,#2084);
#1805=LINE('',#71860,#2085);
#1806=LINE('',#71867,#2086);
#1807=LINE('',#71874,#2087);
#1808=LINE('',#71876,#2088);
#1809=LINE('',#71878,#2089);
#1810=LINE('',#71879,#2090);
#1811=LINE('',#71883,#2091);
#1812=LINE('',#71885,#2092);
#1813=LINE('',#71887,#2093);
#1814=LINE('',#71888,#2094);
#1815=LINE('',#71901,#2095);
#1816=LINE('',#71925,#2096);
#1817=LINE('',#72295,#2097);
#1818=LINE('',#72513,#2098);
#1819=LINE('',#72881,#2099);
#1820=LINE('',#73422,#2100);
#1821=LINE('',#73963,#2101);
#1822=LINE('',#74345,#2102);
#1823=LINE('',#74797,#2103);
#1824=LINE('',#75181,#2104);
#1825=LINE('',#75221,#2105);
#1826=LINE('',#75280,#2106);
#1827=LINE('',#75532,#2107);
#1828=LINE('',#75827,#2108);
#1829=LINE('',#76216,#2109);
#1830=LINE('',#76474,#2110);
#1831=LINE('',#76621,#2111);
#1832=LINE('',#77015,#2112);
#1833=LINE('',#77172,#2113);
#1834=LINE('',#77554,#2114);
#1835=LINE('',#78276,#2115);
#1836=LINE('',#78282,#2116);
#1837=LINE('',#79807,#2117);
#1838=LINE('',#79809,#2118);
#1839=LINE('',#79811,#2119);
#1840=LINE('',#79812,#2120);
#1841=LINE('',#79819,#2121);
#1842=LINE('',#79823,#2122);
#1843=LINE('',#79828,#2123);
#1844=LINE('',#79829,#2124);
#1845=LINE('',#79830,#2125);
#1846=LINE('',#79833,#2126);
#1847=LINE('',#79834,#2127);
#1848=LINE('',#79837,#2128);
#1849=LINE('',#79838,#2129);
#1850=LINE('',#79840,#2130);
#1851=LINE('',#79846,#2131);
#1852=LINE('',#79953,#2132);
#1853=LINE('',#80319,#2133);
#1854=LINE('',#80621,#2134);
#1855=LINE('',#80985,#2135);
#1856=LINE('',#81290,#2136);
#1857=LINE('',#81451,#2137);
#1858=LINE('',#81558,#2138);
#1859=LINE('',#81924,#2139);
#1860=LINE('',#82226,#2140);
#1861=LINE('',#82590,#2141);
#1862=LINE('',#82895,#2142);
#1863=LINE('',#83056,#2143);
#1864=LINE('',#83129,#2144);
#1865=LINE('',#83481,#2145);
#1866=LINE('',#83847,#2146);
#1867=LINE('',#84035,#2147);
#1868=LINE('',#84246,#2148);
#1869=LINE('',#84571,#2149);
#1870=LINE('',#84644,#2150);
#1871=LINE('',#84996,#2151);
#1872=LINE('',#85364,#2152);
#1873=LINE('',#85552,#2153);
#1874=LINE('',#85763,#2154);
#1875=LINE('',#88023,#2155);
#1876=LINE('',#88025,#2156);
#1877=LINE('',#88027,#2157);
#1878=LINE('',#88028,#2158);
#1879=LINE('',#88746,#2159);
#1880=LINE('',#88751,#2160);
#1881=LINE('',#88752,#2161);
#1882=LINE('',#88753,#2162);
#1883=LINE('',#88756,#2163);
#1884=LINE('',#88757,#2164);
#1885=LINE('',#88760,#2165);
#1886=LINE('',#88761,#2166);
#1887=LINE('',#88763,#2167);
#1888=LINE('',#88770,#2168);
#1889=LINE('',#88781,#2169);
#1890=LINE('',#88789,#2170);
#1891=LINE('',#88793,#2171);
#1892=LINE('',#88799,#2172);
#1893=LINE('',#88801,#2173);
#1894=LINE('',#88803,#2174);
#1895=LINE('',#88804,#2175);
#1896=LINE('',#88808,#2176);
#1897=LINE('',#88810,#2177);
#1898=LINE('',#88812,#2178);
#1899=LINE('',#88813,#2179);
#1900=LINE('',#88827,#2180);
#1901=LINE('',#88833,#2181);
#1902=LINE('',#88842,#2182);
#1903=LINE('',#88848,#2183);
#1904=LINE('',#88856,#2184);
#1905=LINE('',#89157,#2185);
#1906=LINE('',#89622,#2186);
#1907=LINE('',#90045,#2187);
#1908=LINE('',#90288,#2188);
#1909=LINE('',#90528,#2189);
#1910=LINE('',#90932,#2190);
#1911=LINE('',#91462,#2191);
#1912=LINE('',#91980,#2192);
#1913=LINE('',#92426,#2193);
#1914=LINE('',#92868,#2194);
#1915=LINE('',#92914,#2195);
#1916=LINE('',#93379,#2196);
#1917=LINE('',#93854,#2197);
#1918=LINE('',#94301,#2198);
#1919=LINE('',#94750,#2199);
#1920=LINE('',#95201,#2200);
#1921=LINE('',#95630,#2201);
#1922=LINE('',#95902,#2202);
#1923=LINE('',#96346,#2203);
#1924=LINE('',#96814,#2204);
#1925=LINE('',#97260,#2205);
#1926=LINE('',#97686,#2206);
#1927=LINE('',#98152,#2207);
#1928=LINE('',#104254,#2208);
#1929=LINE('',#105715,#2209);
#1930=LINE('',#105717,#2210);
#1931=LINE('',#105719,#2211);
#1932=LINE('',#105720,#2212);
#1933=LINE('',#105723,#2213);
#1934=LINE('',#105725,#2214);
#1935=LINE('',#105726,#2215);
#1936=LINE('',#105729,#2216);
#1937=LINE('',#105731,#2217);
#1938=LINE('',#105732,#2218);
#1939=LINE('',#105735,#2219);
#1940=LINE('',#105737,#2220);
#1941=LINE('',#105738,#2221);
#1942=LINE('',#105741,#2222);
#1943=LINE('',#105743,#2223);
#1944=LINE('',#105744,#2224);
#1945=LINE('',#105746,#2225);
#1946=LINE('',#105747,#2226);
#1947=LINE('',#105754,#2227);
#1948=VECTOR('',#7751,4.5);
#1949=VECTOR('',#7758,4.5);
#1950=VECTOR('',#7765,4.5);
#1951=VECTOR('',#7772,4.5);
#1952=VECTOR('',#7777,10.);
#1953=VECTOR('',#7778,10.);
#1954=VECTOR('',#7779,10.);
#1955=VECTOR('',#7780,10.);
#1956=VECTOR('',#7783,10.);
#1957=VECTOR('',#7784,10.);
#1958=VECTOR('',#7785,10.);
#1959=VECTOR('',#7788,10.);
#1960=VECTOR('',#7789,10.);
#1961=VECTOR('',#7790,10.);
#1962=VECTOR('',#7793,10.);
#1963=VECTOR('',#7794,10.);
#1964=VECTOR('',#7805,3.5);
#1965=VECTOR('',#7812,3.5);
#1966=VECTOR('',#7819,7.);
#1967=VECTOR('',#7826,8.);
#1968=VECTOR('',#7833,8.);
#1969=VECTOR('',#7838,10.);
#1970=VECTOR('',#7839,10.);
#1971=VECTOR('',#7840,10.);
#1972=VECTOR('',#7841,10.);
#1973=VECTOR('',#7844,10.);
#1974=VECTOR('',#7845,10.);
#1975=VECTOR('',#7846,10.);
#1976=VECTOR('',#7849,10.);
#1977=VECTOR('',#7850,10.);
#1978=VECTOR('',#7851,10.);
#1979=VECTOR('',#7854,10.);
#1980=VECTOR('',#7855,10.);
#1981=VECTOR('',#7866,5.);
#1982=VECTOR('',#7873,7.);
#1983=VECTOR('',#7884,6.767);
#1984=VECTOR('',#7889,6.767);
#1985=VECTOR('',#7892,6.767);
#1986=VECTOR('',#7895,6.767);
#1987=VECTOR('',#7898,6.767);
#1988=VECTOR('',#7901,6.767);
#1989=VECTOR('',#7904,6.767);
#1990=VECTOR('',#7907,6.767);
#1991=VECTOR('',#7910,6.767);
#1992=VECTOR('',#7913,6.767);
#1993=VECTOR('',#7916,6.767);
#1994=VECTOR('',#7919,6.767);
#1995=VECTOR('',#7922,6.767);
#1996=VECTOR('',#7925,6.767);
#1997=VECTOR('',#7928,6.767);
#1998=VECTOR('',#7931,6.767);
#1999=VECTOR('',#7934,6.767);
#2000=VECTOR('',#7937,6.767);
#2001=VECTOR('',#7940,6.767);
#2002=VECTOR('',#7943,6.767);
#2003=VECTOR('',#7946,6.767);
#2004=VECTOR('',#7949,6.767);
#2005=VECTOR('',#7952,6.767);
#2006=VECTOR('',#7955,6.767);
#2007=VECTOR('',#7958,6.767);
#2008=VECTOR('',#7961,6.767);
#2009=VECTOR('',#7964,6.767);
#2010=VECTOR('',#7967,6.767);
#2011=VECTOR('',#7970,6.767);
#2012=VECTOR('',#7973,6.767);
#2013=VECTOR('',#7976,6.767);
#2014=VECTOR('',#7979,6.767);
#2015=VECTOR('',#7982,6.767);
#2016=VECTOR('',#7985,6.767);
#2017=VECTOR('',#7988,6.767);
#2018=VECTOR('',#7991,6.767);
#2019=VECTOR('',#7994,6.767);
#2020=VECTOR('',#7997,6.767);
#2021=VECTOR('',#8000,6.767);
#2022=VECTOR('',#8003,6.767);
#2023=VECTOR('',#8006,6.767);
#2024=VECTOR('',#8009,6.767);
#2025=VECTOR('',#8012,6.767);
#2026=VECTOR('',#8015,6.767);
#2027=VECTOR('',#8018,6.767);
#2028=VECTOR('',#8021,6.767);
#2029=VECTOR('',#8024,6.767);
#2030=VECTOR('',#8027,6.767);
#2031=VECTOR('',#8030,6.767);
#2032=VECTOR('',#8033,6.767);
#2033=VECTOR('',#8036,6.767);
#2034=VECTOR('',#8039,6.767);
#2035=VECTOR('',#8042,6.767);
#2036=VECTOR('',#8045,6.767);
#2037=VECTOR('',#8048,6.767);
#2038=VECTOR('',#8051,6.767);
#2039=VECTOR('',#8054,6.767);
#2040=VECTOR('',#8057,6.767);
#2041=VECTOR('',#8060,6.767);
#2042=VECTOR('',#8063,6.767);
#2043=VECTOR('',#8066,6.767);
#2044=VECTOR('',#8069,6.767);
#2045=VECTOR('',#8072,6.767);
#2046=VECTOR('',#8075,6.767);
#2047=VECTOR('',#8078,6.767);
#2048=VECTOR('',#8081,6.767);
#2049=VECTOR('',#8084,6.767);
#2050=VECTOR('',#8087,6.767);
#2051=VECTOR('',#8090,6.767);
#2052=VECTOR('',#8093,6.767);
#2053=VECTOR('',#8096,6.767);
#2054=VECTOR('',#8099,6.767);
#2055=VECTOR('',#8102,6.767);
#2056=VECTOR('',#8105,6.767);
#2057=VECTOR('',#8108,6.767);
#2058=VECTOR('',#8111,6.767);
#2059=VECTOR('',#8114,6.767);
#2060=VECTOR('',#8129,4.);
#2061=VECTOR('',#8144,5.);
#2062=VECTOR('',#8147,5.);
#2063=VECTOR('',#8166,10.);
#2064=VECTOR('',#8173,8.);
#2065=VECTOR('',#8180,8.);
#2066=VECTOR('',#8187,8.);
#2067=VECTOR('',#8194,8.);
#2068=VECTOR('',#8201,10.);
#2069=VECTOR('',#8202,10.);
#2070=VECTOR('',#8203,10.);
#2071=VECTOR('',#8204,10.);
#2072=VECTOR('',#8207,10.);
#2073=VECTOR('',#8208,10.);
#2074=VECTOR('',#8209,10.);
#2075=VECTOR('',#8212,10.);
#2076=VECTOR('',#8213,10.);
#2077=VECTOR('',#8214,10.);
#2078=VECTOR('',#8217,10.);
#2079=VECTOR('',#8218,10.);
#2080=VECTOR('',#8219,10.);
#2081=VECTOR('',#8222,10.);
#2082=VECTOR('',#8223,10.);
#2083=VECTOR('',#8224,10.);
#2084=VECTOR('',#8227,10.);
#2085=VECTOR('',#8228,10.);
#2086=VECTOR('',#8237,45.);
#2087=VECTOR('',#8246,10.);
#2088=VECTOR('',#8247,10.);
#2089=VECTOR('',#8248,10.);
#2090=VECTOR('',#8249,10.);
#2091=VECTOR('',#8252,10.);
#2092=VECTOR('',#8253,10.);
#2093=VECTOR('',#8254,10.);
#2094=VECTOR('',#8255,10.);
#2095=VECTOR('',#8276,8.12525);
#2096=VECTOR('',#8281,8.12525);
#2097=VECTOR('',#8284,8.12525);
#2098=VECTOR('',#8287,8.12525);
#2099=VECTOR('',#8290,8.12525);
#2100=VECTOR('',#8293,8.12525);
#2101=VECTOR('',#8296,8.12525);
#2102=VECTOR('',#8299,8.12525);
#2103=VECTOR('',#8302,8.12525);
#2104=VECTOR('',#8305,8.12525);
#2105=VECTOR('',#8310,7.01125);
#2106=VECTOR('',#8315,7.01125);
#2107=VECTOR('',#8318,7.01125);
#2108=VECTOR('',#8321,7.01125);
#2109=VECTOR('',#8324,7.01125);
#2110=VECTOR('',#8327,7.01125);
#2111=VECTOR('',#8330,7.01125);
#2112=VECTOR('',#8333,7.01125);
#2113=VECTOR('',#8336,7.01125);
#2114=VECTOR('',#8339,7.01125);
#2115=VECTOR('',#8350,3.5);
#2116=VECTOR('',#8357,3.5);
#2117=VECTOR('',#8362,10.);
#2118=VECTOR('',#8363,10.);
#2119=VECTOR('',#8364,10.);
#2120=VECTOR('',#8365,10.);
#2121=VECTOR('',#8372,6.);
#2122=VECTOR('',#8377,6.);
#2123=VECTOR('',#8382,10.);
#2124=VECTOR('',#8383,10.);
#2125=VECTOR('',#8384,10.);
#2126=VECTOR('',#8387,10.);
#2127=VECTOR('',#8388,10.);
#2128=VECTOR('',#8391,10.);
#2129=VECTOR('',#8392,10.);
#2130=VECTOR('',#8395,10.);
#2131=VECTOR('',#8402,3.0735);
#2132=VECTOR('',#8407,3.0735);
#2133=VECTOR('',#8410,3.0735);
#2134=VECTOR('',#8413,3.0735);
#2135=VECTOR('',#8416,3.0735);
#2136=VECTOR('',#8419,3.0735);
#2137=VECTOR('',#8424,3.0735);
#2138=VECTOR('',#8429,3.0735);
#2139=VECTOR('',#8432,3.0735);
#2140=VECTOR('',#8435,3.0735);
#2141=VECTOR('',#8438,3.0735);
#2142=VECTOR('',#8441,3.0735);
#2143=VECTOR('',#8446,2.5175);
#2144=VECTOR('',#8451,2.5175);
#2145=VECTOR('',#8454,2.5175);
#2146=VECTOR('',#8457,2.5175);
#2147=VECTOR('',#8460,2.5175);
#2148=VECTOR('',#8463,2.5175);
#2149=VECTOR('',#8468,2.5175);
#2150=VECTOR('',#8473,2.5175);
#2151=VECTOR('',#8476,2.5175);
#2152=VECTOR('',#8479,2.5175);
#2153=VECTOR('',#8482,2.5175);
#2154=VECTOR('',#8485,2.5175);
#2155=VECTOR('',#8498,10.);
#2156=VECTOR('',#8499,10.);
#2157=VECTOR('',#8500,10.);
#2158=VECTOR('',#8501,10.);
#2159=VECTOR('',#8506,11.);
#2160=VECTOR('',#8511,10.);
#2161=VECTOR('',#8512,10.);
#2162=VECTOR('',#8513,10.);
#2163=VECTOR('',#8516,10.);
#2164=VECTOR('',#8517,10.);
#2165=VECTOR('',#8520,10.);
#2166=VECTOR('',#8521,10.);
#2167=VECTOR('',#8524,10.);
#2168=VECTOR('',#8533,5.);
#2169=VECTOR('',#8548,6.);
#2170=VECTOR('',#8557,8.);
#2171=VECTOR('',#8564,6.);
#2172=VECTOR('',#8571,10.);
#2173=VECTOR('',#8572,10.);
#2174=VECTOR('',#8573,10.);
#2175=VECTOR('',#8574,10.);
#2176=VECTOR('',#8577,10.);
#2177=VECTOR('',#8578,10.);
#2178=VECTOR('',#8579,10.);
#2179=VECTOR('',#8580,10.);
#2180=VECTOR('',#8603,6.);
#2181=VECTOR('',#8610,8.);
#2182=VECTOR('',#8623,5.);
#2183=VECTOR('',#8630,10.);
#2184=VECTOR('',#8641,2.37175);
#2185=VECTOR('',#8646,2.37175);
#2186=VECTOR('',#8649,2.37175);
#2187=VECTOR('',#8652,2.37175);
#2188=VECTOR('',#8655,2.37175);
#2189=VECTOR('',#8658,2.37175);
#2190=VECTOR('',#8661,2.37175);
#2191=VECTOR('',#8664,2.37175);
#2192=VECTOR('',#8667,2.37175);
#2193=VECTOR('',#8670,2.37175);
#2194=VECTOR('',#8673,2.37175);
#2195=VECTOR('',#8676,2.37175);
#2196=VECTOR('',#8679,2.37175);
#2197=VECTOR('',#8682,2.37175);
#2198=VECTOR('',#8685,2.37175);
#2199=VECTOR('',#8688,2.37175);
#2200=VECTOR('',#8691,2.37175);
#2201=VECTOR('',#8694,2.37175);
#2202=VECTOR('',#8697,2.37175);
#2203=VECTOR('',#8700,2.37175);
#2204=VECTOR('',#8703,2.37175);
#2205=VECTOR('',#8706,2.37175);
#2206=VECTOR('',#8709,2.37175);
#2207=VECTOR('',#8712,2.37175);
#2208=VECTOR('',#8725,2.5);
#2209=VECTOR('',#8730,10.);
#2210=VECTOR('',#8731,10.);
#2211=VECTOR('',#8732,10.);
#2212=VECTOR('',#8733,10.);
#2213=VECTOR('',#8736,10.);
#2214=VECTOR('',#8737,10.);
#2215=VECTOR('',#8738,10.);
#2216=VECTOR('',#8741,9.99999999999999);
#2217=VECTOR('',#8742,10.);
#2218=VECTOR('',#8743,10.);
#2219=VECTOR('',#8746,10.);
#2220=VECTOR('',#8747,10.);
#2221=VECTOR('',#8748,10.);
#2222=VECTOR('',#8751,10.);
#2223=VECTOR('',#8752,10.);
#2224=VECTOR('',#8753,10.);
#2225=VECTOR('',#8756,10.);
#2226=VECTOR('',#8757,10.);
#2227=VECTOR('',#8766,5.);
#2228=CIRCLE('',#7350,4.5);
#2229=CIRCLE('',#7351,4.5);
#2230=CIRCLE('',#7353,4.5);
#2231=CIRCLE('',#7354,4.5);
#2232=CIRCLE('',#7356,4.5);
#2233=CIRCLE('',#7357,4.5);
#2234=CIRCLE('',#7359,4.5);
#2235=CIRCLE('',#7360,4.5);
#2236=CIRCLE('',#7369,3.5);
#2237=CIRCLE('',#7370,3.5);
#2238=CIRCLE('',#7372,3.5);
#2239=CIRCLE('',#7373,3.5);
#2240=CIRCLE('',#7375,7.);
#2241=CIRCLE('',#7376,7.);
#2242=CIRCLE('',#7378,8.);
#2243=CIRCLE('',#7379,8.);
#2244=CIRCLE('',#7381,8.);
#2245=CIRCLE('',#7382,8.);
#2246=CIRCLE('',#7391,5.);
#2247=CIRCLE('',#7392,5.);
#2248=CIRCLE('',#7394,7.);
#2249=CIRCLE('',#7395,7.);
#2250=CIRCLE('',#7400,6.767);
#2251=CIRCLE('',#7478,6.767);
#2252=CIRCLE('',#7480,7.911);
#2253=CIRCLE('',#7481,7.911);
#2254=CIRCLE('',#7483,4.);
#2255=CIRCLE('',#7484,4.);
#2256=CIRCLE('',#7486,5.);
#2257=CIRCLE('',#7488,5.);
#2258=CIRCLE('',#7490,5.);
#2259=CIRCLE('',#7492,5.);
#2260=CIRCLE('',#7495,10.);
#2261=CIRCLE('',#7496,7.);
#2262=CIRCLE('',#7500,10.);
#2263=CIRCLE('',#7503,8.);
#2264=CIRCLE('',#7504,8.);
#2265=CIRCLE('',#7506,8.);
#2266=CIRCLE('',#7507,8.);
#2267=CIRCLE('',#7509,8.);
#2268=CIRCLE('',#7510,8.);
#2269=CIRCLE('',#7512,8.);
#2270=CIRCLE('',#7513,8.);
#2271=CIRCLE('',#7523,45.);
#2272=CIRCLE('',#7525,45.);
#2273=CIRCLE('',#7531,8.);
#2274=CIRCLE('',#7532,4.);
#2275=CIRCLE('',#7534,4.);
#2276=CIRCLE('',#7536,8.);
#2277=CIRCLE('',#7540,8.12525);
#2278=CIRCLE('',#7550,8.12525);
#2279=CIRCLE('',#7552,7.01125);
#2280=CIRCLE('',#7562,7.01125);
#2281=CIRCLE('',#7566,3.5);
#2282=CIRCLE('',#7567,3.5);
#2283=CIRCLE('',#7569,3.5);
#2284=CIRCLE('',#7570,3.5);
#2285=CIRCLE('',#7572,6.);
#2286=CIRCLE('',#7573,6.);
#2287=CIRCLE('',#7575,6.);
#2288=CIRCLE('',#7577,6.);
#2289=CIRCLE('',#7585,3.0735);
#2290=CIRCLE('',#7591,3.0735);
#2291=CIRCLE('',#7593,3.0735);
#2292=CIRCLE('',#7599,3.0735);
#2293=CIRCLE('',#7601,2.5175);
#2294=CIRCLE('',#7607,2.5175);
#2295=CIRCLE('',#7609,2.5175);
#2296=CIRCLE('',#7615,2.5175);
#2297=CIRCLE('',#7621,11.);
#2298=CIRCLE('',#7623,11.);
#2299=CIRCLE('',#7631,5.);
#2300=CIRCLE('',#7632,5.);
#2301=CIRCLE('',#7634,6.);
#2302=CIRCLE('',#7636,6.);
#2303=CIRCLE('',#7638,6.);
#2304=CIRCLE('',#7640,8.);
#2305=CIRCLE('',#7641,6.);
#2306=CIRCLE('',#7643,8.);
#2307=CIRCLE('',#7651,9.);
#2308=CIRCLE('',#7652,5.);
#2309=CIRCLE('',#7654,5.);
#2310=CIRCLE('',#7656,9.);
#2311=CIRCLE('',#7660,6.);
#2312=CIRCLE('',#7661,6.);
#2313=CIRCLE('',#7663,8.);
#2314=CIRCLE('',#7664,8.);
#2315=CIRCLE('',#7669,5.);
#2316=CIRCLE('',#7670,5.);
#2317=CIRCLE('',#7672,10.);
#2318=CIRCLE('',#7673,10.);
#2319=CIRCLE('',#7678,2.37175);
#2320=CIRCLE('',#7703,2.942);
#2321=CIRCLE('',#7704,2.942);
#2322=CIRCLE('',#7706,2.37175);
#2323=CIRCLE('',#7708,2.);
#2324=CIRCLE('',#7717,5.);
#2325=CIRCLE('',#7719,5.);
#2326=VERTEX_POINT('',#8818);
#2327=VERTEX_POINT('',#8820);
#2328=VERTEX_POINT('',#8824);
#2329=VERTEX_POINT('',#8826);
#2330=VERTEX_POINT('',#8830);
#2331=VERTEX_POINT('',#8832);
#2332=VERTEX_POINT('',#8836);
#2333=VERTEX_POINT('',#8838);
#2334=VERTEX_POINT('',#8842);
#2335=VERTEX_POINT('',#8843);
#2336=VERTEX_POINT('',#8845);
#2337=VERTEX_POINT('',#8847);
#2338=VERTEX_POINT('',#8851);
#2339=VERTEX_POINT('',#8853);
#2340=VERTEX_POINT('',#8857);
#2341=VERTEX_POINT('',#8859);
#2342=VERTEX_POINT('',#8869);
#2343=VERTEX_POINT('',#8871);
#2344=VERTEX_POINT('',#8875);
#2345=VERTEX_POINT('',#8877);
#2346=VERTEX_POINT('',#8881);
#2347=VERTEX_POINT('',#8883);
#2348=VERTEX_POINT('',#8887);
#2349=VERTEX_POINT('',#8889);
#2350=VERTEX_POINT('',#8893);
#2351=VERTEX_POINT('',#8895);
#2352=VERTEX_POINT('',#8899);
#2353=VERTEX_POINT('',#8900);
#2354=VERTEX_POINT('',#8902);
#2355=VERTEX_POINT('',#8904);
#2356=VERTEX_POINT('',#8908);
#2357=VERTEX_POINT('',#8910);
#2358=VERTEX_POINT('',#8914);
#2359=VERTEX_POINT('',#8916);
#2360=VERTEX_POINT('',#8926);
#2361=VERTEX_POINT('',#8928);
#2362=VERTEX_POINT('',#8932);
#2363=VERTEX_POINT('',#8934);
#2364=VERTEX_POINT('',#8941);
#2365=VERTEX_POINT('',#8942);
#2366=VERTEX_POINT('',#8944);
#2367=VERTEX_POINT('',#9078);
#2368=VERTEX_POINT('',#9157);
#2369=VERTEX_POINT('',#9158);
#2370=VERTEX_POINT('',#9160);
#2371=VERTEX_POINT('',#9403);
#2372=VERTEX_POINT('',#9653);
#2373=VERTEX_POINT('',#9654);
#2374=VERTEX_POINT('',#9656);
#2375=VERTEX_POINT('',#9899);
#2376=VERTEX_POINT('',#10155);
#2377=VERTEX_POINT('',#10156);
#2378=VERTEX_POINT('',#10158);
#2379=VERTEX_POINT('',#10413);
#2380=VERTEX_POINT('',#10666);
#2381=VERTEX_POINT('',#10667);
#2382=VERTEX_POINT('',#10669);
#2383=VERTEX_POINT('',#10906);
#2384=VERTEX_POINT('',#11159);
#2385=VERTEX_POINT('',#11160);
#2386=VERTEX_POINT('',#11162);
#2387=VERTEX_POINT('',#11411);
#2388=VERTEX_POINT('',#11652);
#2389=VERTEX_POINT('',#11653);
#2390=VERTEX_POINT('',#11655);
#2391=VERTEX_POINT('',#11907);
#2392=VERTEX_POINT('',#12151);
#2393=VERTEX_POINT('',#12152);
#2394=VERTEX_POINT('',#12154);
#2395=VERTEX_POINT('',#12406);
#2396=VERTEX_POINT('',#12650);
#2397=VERTEX_POINT('',#12651);
#2398=VERTEX_POINT('',#12653);
#2399=VERTEX_POINT('',#12893);
#2400=VERTEX_POINT('',#13140);
#2401=VERTEX_POINT('',#13141);
#2402=VERTEX_POINT('',#13143);
#2403=VERTEX_POINT('',#13386);
#2404=VERTEX_POINT('',#13627);
#2405=VERTEX_POINT('',#13628);
#2406=VERTEX_POINT('',#13630);
#2407=VERTEX_POINT('',#13885);
#2408=VERTEX_POINT('',#14132);
#2409=VERTEX_POINT('',#14133);
#2410=VERTEX_POINT('',#14135);
#2411=VERTEX_POINT('',#14378);
#2412=VERTEX_POINT('',#14637);
#2413=VERTEX_POINT('',#14638);
#2414=VERTEX_POINT('',#14640);
#2415=VERTEX_POINT('',#14883);
#2416=VERTEX_POINT('',#15139);
#2417=VERTEX_POINT('',#15140);
#2418=VERTEX_POINT('',#15142);
#2419=VERTEX_POINT('',#15382);
#2420=VERTEX_POINT('',#15635);
#2421=VERTEX_POINT('',#15636);
#2422=VERTEX_POINT('',#15638);
#2423=VERTEX_POINT('',#15887);
#2424=VERTEX_POINT('',#16128);
#2425=VERTEX_POINT('',#16129);
#2426=VERTEX_POINT('',#16131);
#2427=VERTEX_POINT('',#16371);
#2428=VERTEX_POINT('',#16618);
#2429=VERTEX_POINT('',#16619);
#2430=VERTEX_POINT('',#16621);
#2431=VERTEX_POINT('',#16867);
#2432=VERTEX_POINT('',#17120);
#2433=VERTEX_POINT('',#17121);
#2434=VERTEX_POINT('',#17123);
#2435=VERTEX_POINT('',#17381);
#2436=VERTEX_POINT('',#17634);
#2437=VERTEX_POINT('',#17635);
#2438=VERTEX_POINT('',#17637);
#2439=VERTEX_POINT('',#17877);
#2440=VERTEX_POINT('',#18133);
#2441=VERTEX_POINT('',#18134);
#2442=VERTEX_POINT('',#18136);
#2443=VERTEX_POINT('',#18379);
#2444=VERTEX_POINT('',#18620);
#2445=VERTEX_POINT('',#18621);
#2446=VERTEX_POINT('',#18623);
#2447=VERTEX_POINT('',#18866);
#2448=VERTEX_POINT('',#19113);
#2449=VERTEX_POINT('',#19114);
#2450=VERTEX_POINT('',#19116);
#2451=VERTEX_POINT('',#19362);
#2452=VERTEX_POINT('',#19621);
#2453=VERTEX_POINT('',#19622);
#2454=VERTEX_POINT('',#19624);
#2455=VERTEX_POINT('',#19864);
#2456=VERTEX_POINT('',#20120);
#2457=VERTEX_POINT('',#20121);
#2458=VERTEX_POINT('',#20123);
#2459=VERTEX_POINT('',#20369);
#2460=VERTEX_POINT('',#20622);
#2461=VERTEX_POINT('',#20623);
#2462=VERTEX_POINT('',#20625);
#2463=VERTEX_POINT('',#20868);
#2464=VERTEX_POINT('',#21109);
#2465=VERTEX_POINT('',#21110);
#2466=VERTEX_POINT('',#21112);
#2467=VERTEX_POINT('',#21346);
#2468=VERTEX_POINT('',#21593);
#2469=VERTEX_POINT('',#21594);
#2470=VERTEX_POINT('',#21596);
#2471=VERTEX_POINT('',#21842);
#2472=VERTEX_POINT('',#22095);
#2473=VERTEX_POINT('',#22096);
#2474=VERTEX_POINT('',#22098);
#2475=VERTEX_POINT('',#22350);
#2476=VERTEX_POINT('',#22603);
#2477=VERTEX_POINT('',#22604);
#2478=VERTEX_POINT('',#22606);
#2479=VERTEX_POINT('',#22855);
#2480=VERTEX_POINT('',#23111);
#2481=VERTEX_POINT('',#23112);
#2482=VERTEX_POINT('',#23114);
#2483=VERTEX_POINT('',#23354);
#2484=VERTEX_POINT('',#23595);
#2485=VERTEX_POINT('',#23596);
#2486=VERTEX_POINT('',#23598);
#2487=VERTEX_POINT('',#23841);
#2488=VERTEX_POINT('',#24088);
#2489=VERTEX_POINT('',#24089);
#2490=VERTEX_POINT('',#24091);
#2491=VERTEX_POINT('',#24346);
#2492=VERTEX_POINT('',#24599);
#2493=VERTEX_POINT('',#24600);
#2494=VERTEX_POINT('',#24602);
#2495=VERTEX_POINT('',#24854);
#2496=VERTEX_POINT('',#25110);
#2497=VERTEX_POINT('',#25111);
#2498=VERTEX_POINT('',#25113);
#2499=VERTEX_POINT('',#25365);
#2500=VERTEX_POINT('',#25606);
#2501=VERTEX_POINT('',#25607);
#2502=VERTEX_POINT('',#25609);
#2503=VERTEX_POINT('',#25852);
#2504=VERTEX_POINT('',#26087);
#2505=VERTEX_POINT('',#26088);
#2506=VERTEX_POINT('',#26090);
#2507=VERTEX_POINT('',#26339);
#2508=VERTEX_POINT('',#26586);
#2509=VERTEX_POINT('',#26587);
#2510=VERTEX_POINT('',#26589);
#2511=VERTEX_POINT('',#26841);
#2512=VERTEX_POINT('',#27085);
#2513=VERTEX_POINT('',#27086);
#2514=VERTEX_POINT('',#27088);
#2515=VERTEX_POINT('',#27337);
#2516=VERTEX_POINT('',#27581);
#2517=VERTEX_POINT('',#27582);
#2518=VERTEX_POINT('',#27584);
#2519=VERTEX_POINT('',#27839);
#2520=VERTEX_POINT('',#28098);
#2521=VERTEX_POINT('',#28099);
#2522=VERTEX_POINT('',#28101);
#2523=VERTEX_POINT('',#28341);
#2524=VERTEX_POINT('',#28582);
#2525=VERTEX_POINT('',#28583);
#2526=VERTEX_POINT('',#28585);
#2527=VERTEX_POINT('',#28831);
#2528=VERTEX_POINT('',#29075);
#2529=VERTEX_POINT('',#29076);
#2530=VERTEX_POINT('',#29078);
#2531=VERTEX_POINT('',#29333);
#2532=VERTEX_POINT('',#29577);
#2533=VERTEX_POINT('',#29578);
#2534=VERTEX_POINT('',#29580);
#2535=VERTEX_POINT('',#29829);
#2536=VERTEX_POINT('',#30076);
#2537=VERTEX_POINT('',#30077);
#2538=VERTEX_POINT('',#30079);
#2539=VERTEX_POINT('',#30322);
#2540=VERTEX_POINT('',#30563);
#2541=VERTEX_POINT('',#30564);
#2542=VERTEX_POINT('',#30566);
#2543=VERTEX_POINT('',#30809);
#2544=VERTEX_POINT('',#30896);
#2545=VERTEX_POINT('',#30897);
#2546=VERTEX_POINT('',#30899);
#2547=VERTEX_POINT('',#31154);
#2548=VERTEX_POINT('',#31334);
#2549=VERTEX_POINT('',#31335);
#2550=VERTEX_POINT('',#31337);
#2551=VERTEX_POINT('',#31589);
#2552=VERTEX_POINT('',#31830);
#2553=VERTEX_POINT('',#31831);
#2554=VERTEX_POINT('',#31833);
#2555=VERTEX_POINT('',#32085);
#2556=VERTEX_POINT('',#32332);
#2557=VERTEX_POINT('',#32333);
#2558=VERTEX_POINT('',#32335);
#2559=VERTEX_POINT('',#32578);
#2560=VERTEX_POINT('',#32834);
#2561=VERTEX_POINT('',#32835);
#2562=VERTEX_POINT('',#32837);
#2563=VERTEX_POINT('',#33086);
#2564=VERTEX_POINT('',#33336);
#2565=VERTEX_POINT('',#33337);
#2566=VERTEX_POINT('',#33339);
#2567=VERTEX_POINT('',#33591);
#2568=VERTEX_POINT('',#33832);
#2569=VERTEX_POINT('',#33833);
#2570=VERTEX_POINT('',#33835);
#2571=VERTEX_POINT('',#34087);
#2572=VERTEX_POINT('',#34334);
#2573=VERTEX_POINT('',#34335);
#2574=VERTEX_POINT('',#34337);
#2575=VERTEX_POINT('',#34580);
#2576=VERTEX_POINT('',#34836);
#2577=VERTEX_POINT('',#34837);
#2578=VERTEX_POINT('',#34839);
#2579=VERTEX_POINT('',#35085);
#2580=VERTEX_POINT('',#35323);
#2581=VERTEX_POINT('',#35324);
#2582=VERTEX_POINT('',#35326);
#2583=VERTEX_POINT('',#35578);
#2584=VERTEX_POINT('',#35828);
#2585=VERTEX_POINT('',#35829);
#2586=VERTEX_POINT('',#35831);
#2587=VERTEX_POINT('',#36086);
#2588=VERTEX_POINT('',#36330);
#2589=VERTEX_POINT('',#36331);
#2590=VERTEX_POINT('',#36333);
#2591=VERTEX_POINT('',#36585);
#2592=VERTEX_POINT('',#36820);
#2593=VERTEX_POINT('',#36821);
#2594=VERTEX_POINT('',#36823);
#2595=VERTEX_POINT('',#37060);
#2596=VERTEX_POINT('',#37307);
#2597=VERTEX_POINT('',#37308);
#2598=VERTEX_POINT('',#37310);
#2599=VERTEX_POINT('',#37556);
#2600=VERTEX_POINT('',#37809);
#2601=VERTEX_POINT('',#37810);
#2602=VERTEX_POINT('',#37812);
#2603=VERTEX_POINT('',#38067);
#2604=VERTEX_POINT('',#38320);
#2605=VERTEX_POINT('',#38321);
#2606=VERTEX_POINT('',#38323);
#2607=VERTEX_POINT('',#38575);
#2608=VERTEX_POINT('',#38816);
#2609=VERTEX_POINT('',#38817);
#2610=VERTEX_POINT('',#38819);
#2611=VERTEX_POINT('',#39059);
#2612=VERTEX_POINT('',#39306);
#2613=VERTEX_POINT('',#39307);
#2614=VERTEX_POINT('',#39309);
#2615=VERTEX_POINT('',#39543);
#2616=VERTEX_POINT('',#39796);
#2617=VERTEX_POINT('',#39797);
#2618=VERTEX_POINT('',#39799);
#2619=VERTEX_POINT('',#40045);
#2620=VERTEX_POINT('',#40295);
#2621=VERTEX_POINT('',#40296);
#2622=VERTEX_POINT('',#40298);
#2623=VERTEX_POINT('',#40538);
#2624=VERTEX_POINT('',#40794);
#2625=VERTEX_POINT('',#40795);
#2626=VERTEX_POINT('',#40797);
#2627=VERTEX_POINT('',#41043);
#2628=VERTEX_POINT('',#41287);
#2629=VERTEX_POINT('',#41288);
#2630=VERTEX_POINT('',#41290);
#2631=VERTEX_POINT('',#41530);
#2632=VERTEX_POINT('',#41780);
#2633=VERTEX_POINT('',#41781);
#2634=VERTEX_POINT('',#41783);
#2635=VERTEX_POINT('',#42032);
#2636=VERTEX_POINT('',#42285);
#2637=VERTEX_POINT('',#42286);
#2638=VERTEX_POINT('',#42288);
#2639=VERTEX_POINT('',#42528);
#2640=VERTEX_POINT('',#42778);
#2641=VERTEX_POINT('',#42779);
#2642=VERTEX_POINT('',#42781);
#2643=VERTEX_POINT('',#43030);
#2644=VERTEX_POINT('',#43286);
#2645=VERTEX_POINT('',#43287);
#2646=VERTEX_POINT('',#43289);
#2647=VERTEX_POINT('',#43544);
#2648=VERTEX_POINT('',#43785);
#2649=VERTEX_POINT('',#43786);
#2650=VERTEX_POINT('',#43788);
#2651=VERTEX_POINT('',#44025);
#2652=VERTEX_POINT('',#44272);
#2653=VERTEX_POINT('',#44273);
#2654=VERTEX_POINT('',#44275);
#2655=VERTEX_POINT('',#44518);
#2656=VERTEX_POINT('',#44771);
#2657=VERTEX_POINT('',#44772);
#2658=VERTEX_POINT('',#44774);
#2659=VERTEX_POINT('',#45017);
#2660=VERTEX_POINT('',#45267);
#2661=VERTEX_POINT('',#45268);
#2662=VERTEX_POINT('',#45270);
#2663=VERTEX_POINT('',#45516);
#2664=VERTEX_POINT('',#45769);
#2665=VERTEX_POINT('',#45770);
#2666=VERTEX_POINT('',#45772);
#2667=VERTEX_POINT('',#46027);
#2668=VERTEX_POINT('',#46271);
#2669=VERTEX_POINT('',#46272);
#2670=VERTEX_POINT('',#46274);
#2671=VERTEX_POINT('',#46529);
#2672=VERTEX_POINT('',#46776);
#2673=VERTEX_POINT('',#46859);
#2674=VERTEX_POINT('',#46942);
#2675=VERTEX_POINT('',#46944);
#2676=VERTEX_POINT('',#47065);
#2677=VERTEX_POINT('',#47066);
#2678=VERTEX_POINT('',#47075);
#2679=VERTEX_POINT('',#47077);
#2680=VERTEX_POINT('',#47121);
#2681=VERTEX_POINT('',#47384);
#2682=VERTEX_POINT('',#47403);
#2683=VERTEX_POINT('',#47669);
#2684=VERTEX_POINT('',#47688);
#2685=VERTEX_POINT('',#47707);
#2686=VERTEX_POINT('',#47719);
#2687=VERTEX_POINT('',#47738);
#2688=VERTEX_POINT('',#47750);
#2689=VERTEX_POINT('',#47769);
#2690=VERTEX_POINT('',#47788);
#2691=VERTEX_POINT('',#47807);
#2692=VERTEX_POINT('',#47826);
#2693=VERTEX_POINT('',#47837);
#2694=VERTEX_POINT('',#47856);
#2695=VERTEX_POINT('',#48119);
#2696=VERTEX_POINT('',#48138);
#2697=VERTEX_POINT('',#48401);
#2698=VERTEX_POINT('',#48415);
#2699=VERTEX_POINT('',#48434);
#2700=VERTEX_POINT('',#48453);
#2701=VERTEX_POINT('',#48472);
#2702=VERTEX_POINT('',#48738);
#2703=VERTEX_POINT('',#48757);
#2704=VERTEX_POINT('',#48769);
#2705=VERTEX_POINT('',#48788);
#2706=VERTEX_POINT('',#48807);
#2707=VERTEX_POINT('',#48819);
#2708=VERTEX_POINT('',#48832);
#2709=VERTEX_POINT('',#49098);
#2710=VERTEX_POINT('',#49117);
#2711=VERTEX_POINT('',#49380);
#2712=VERTEX_POINT('',#49399);
#2713=VERTEX_POINT('',#49418);
#2714=VERTEX_POINT('',#49684);
#2715=VERTEX_POINT('',#49703);
#2716=VERTEX_POINT('',#49715);
#2717=VERTEX_POINT('',#49981);
#2718=VERTEX_POINT('',#49993);
#2719=VERTEX_POINT('',#50012);
#2720=VERTEX_POINT('',#50031);
#2721=VERTEX_POINT('',#50043);
#2722=VERTEX_POINT('',#50056);
#2723=VERTEX_POINT('',#50322);
#2724=VERTEX_POINT('',#50341);
#2725=VERTEX_POINT('',#50604);
#2726=VERTEX_POINT('',#50623);
#2727=VERTEX_POINT('',#50635);
#2728=VERTEX_POINT('',#50877);
#2729=VERTEX_POINT('',#50896);
#2730=VERTEX_POINT('',#50908);
#2731=VERTEX_POINT('',#51174);
#2732=VERTEX_POINT('',#51186);
#2733=VERTEX_POINT('',#51205);
#2734=VERTEX_POINT('',#51224);
#2735=VERTEX_POINT('',#51490);
#2736=VERTEX_POINT('',#51509);
#2737=VERTEX_POINT('',#51772);
#2738=VERTEX_POINT('',#51791);
#2739=VERTEX_POINT('',#52057);
#2740=VERTEX_POINT('',#52071);
#2741=VERTEX_POINT('',#52083);
#2742=VERTEX_POINT('',#52102);
#2743=VERTEX_POINT('',#52121);
#2744=VERTEX_POINT('',#52133);
#2745=VERTEX_POINT('',#52152);
#2746=VERTEX_POINT('',#52418);
#2747=VERTEX_POINT('',#52437);
#2748=VERTEX_POINT('',#52456);
#2749=VERTEX_POINT('',#52475);
#2750=VERTEX_POINT('',#52488);
#2751=VERTEX_POINT('',#52751);
#2752=VERTEX_POINT('',#52770);
#2753=VERTEX_POINT('',#52782);
#2754=VERTEX_POINT('',#52801);
#2755=VERTEX_POINT('',#53064);
#2756=VERTEX_POINT('',#53083);
#2757=VERTEX_POINT('',#53092);
#2758=VERTEX_POINT('',#53094);
#2759=VERTEX_POINT('',#53101);
#2760=VERTEX_POINT('',#53113);
#2761=VERTEX_POINT('',#53702);
#2762=VERTEX_POINT('',#53968);
#2763=VERTEX_POINT('',#53987);
#2764=VERTEX_POINT('',#54253);
#2765=VERTEX_POINT('',#54272);
#2766=VERTEX_POINT('',#54284);
#2767=VERTEX_POINT('',#54550);
#2768=VERTEX_POINT('',#54562);
#2769=VERTEX_POINT('',#55155);
#2770=VERTEX_POINT('',#55421);
#2771=VERTEX_POINT('',#55654);
#2772=VERTEX_POINT('',#56245);
#2773=VERTEX_POINT('',#56264);
#2774=VERTEX_POINT('',#56530);
#2775=VERTEX_POINT('',#57105);
#2776=VERTEX_POINT('',#57124);
#2777=VERTEX_POINT('',#57143);
#2778=VERTEX_POINT('',#57155);
#2779=VERTEX_POINT('',#57174);
#2780=VERTEX_POINT('',#57437);
#2781=VERTEX_POINT('',#58042);
#2782=VERTEX_POINT('',#58643);
#2783=VERTEX_POINT('',#58655);
#2784=VERTEX_POINT('',#59216);
#2785=VERTEX_POINT('',#59482);
#2786=VERTEX_POINT('',#59501);
#2787=VERTEX_POINT('',#59764);
#2788=VERTEX_POINT('',#60341);
#2789=VERTEX_POINT('',#60958);
#2790=VERTEX_POINT('',#61221);
#2791=VERTEX_POINT('',#61240);
#2792=VERTEX_POINT('',#61252);
#2793=VERTEX_POINT('',#61841);
#2794=VERTEX_POINT('',#62408);
#2795=VERTEX_POINT('',#62674);
#2796=VERTEX_POINT('',#62693);
#2797=VERTEX_POINT('',#63266);
#2798=VERTEX_POINT('',#63285);
#2799=VERTEX_POINT('',#63551);
#2800=VERTEX_POINT('',#64116);
#2801=VERTEX_POINT('',#64128);
#2802=VERTEX_POINT('',#64394);
#2803=VERTEX_POINT('',#64406);
#2804=VERTEX_POINT('',#64425);
#2805=VERTEX_POINT('',#64691);
#2806=VERTEX_POINT('',#64710);
#2807=VERTEX_POINT('',#64976);
#2808=VERTEX_POINT('',#65218);
#2809=VERTEX_POINT('',#65237);
#2810=VERTEX_POINT('',#65249);
#2811=VERTEX_POINT('',#65515);
#2812=VERTEX_POINT('',#65527);
#2813=VERTEX_POINT('',#65546);
#2814=VERTEX_POINT('',#65565);
#2815=VERTEX_POINT('',#65577);
#2816=VERTEX_POINT('',#65596);
#2817=VERTEX_POINT('',#65608);
#2818=VERTEX_POINT('',#65847);
#2819=VERTEX_POINT('',#66981);
#2820=VERTEX_POINT('',#66983);
#2821=VERTEX_POINT('',#66987);
#2822=VERTEX_POINT('',#66990);
#2823=VERTEX_POINT('',#66993);
#2824=VERTEX_POINT('',#66997);
#2825=VERTEX_POINT('',#67002);
#2826=VERTEX_POINT('',#67004);
#2827=VERTEX_POINT('',#67005);
#2828=VERTEX_POINT('',#67010);
#2829=VERTEX_POINT('',#67015);
#2830=VERTEX_POINT('',#67017);
#2831=VERTEX_POINT('',#67021);
#2832=VERTEX_POINT('',#67023);
#2833=VERTEX_POINT('',#67027);
#2834=VERTEX_POINT('',#67029);
#2835=VERTEX_POINT('',#67033);
#2836=VERTEX_POINT('',#67035);
#2837=VERTEX_POINT('',#71826);
#2838=VERTEX_POINT('',#71827);
#2839=VERTEX_POINT('',#71829);
#2840=VERTEX_POINT('',#71831);
#2841=VERTEX_POINT('',#71835);
#2842=VERTEX_POINT('',#71837);
#2843=VERTEX_POINT('',#71841);
#2844=VERTEX_POINT('',#71843);
#2845=VERTEX_POINT('',#71847);
#2846=VERTEX_POINT('',#71849);
#2847=VERTEX_POINT('',#71853);
#2848=VERTEX_POINT('',#71855);
#2849=VERTEX_POINT('',#71863);
#2850=VERTEX_POINT('',#71866);
#2851=VERTEX_POINT('',#71872);
#2852=VERTEX_POINT('',#71873);
#2853=VERTEX_POINT('',#71875);
#2854=VERTEX_POINT('',#71877);
#2855=VERTEX_POINT('',#71881);
#2856=VERTEX_POINT('',#71882);
#2857=VERTEX_POINT('',#71884);
#2858=VERTEX_POINT('',#71886);
#2859=VERTEX_POINT('',#71899);
#2860=VERTEX_POINT('',#71900);
#2861=VERTEX_POINT('',#71902);
#2862=VERTEX_POINT('',#71911);
#2863=VERTEX_POINT('',#71923);
#2864=VERTEX_POINT('',#71924);
#2865=VERTEX_POINT('',#71926);
#2866=VERTEX_POINT('',#72110);
#2867=VERTEX_POINT('',#72293);
#2868=VERTEX_POINT('',#72294);
#2869=VERTEX_POINT('',#72296);
#2870=VERTEX_POINT('',#72403);
#2871=VERTEX_POINT('',#72511);
#2872=VERTEX_POINT('',#72512);
#2873=VERTEX_POINT('',#72514);
#2874=VERTEX_POINT('',#72696);
#2875=VERTEX_POINT('',#72879);
#2876=VERTEX_POINT('',#72880);
#2877=VERTEX_POINT('',#72882);
#2878=VERTEX_POINT('',#73149);
#2879=VERTEX_POINT('',#73420);
#2880=VERTEX_POINT('',#73421);
#2881=VERTEX_POINT('',#73423);
#2882=VERTEX_POINT('',#73690);
#2883=VERTEX_POINT('',#73961);
#2884=VERTEX_POINT('',#73962);
#2885=VERTEX_POINT('',#73964);
#2886=VERTEX_POINT('',#74072);
#2887=VERTEX_POINT('',#74343);
#2888=VERTEX_POINT('',#74344);
#2889=VERTEX_POINT('',#74346);
#2890=VERTEX_POINT('',#74527);
#2891=VERTEX_POINT('',#74795);
#2892=VERTEX_POINT('',#74796);
#2893=VERTEX_POINT('',#74798);
#2894=VERTEX_POINT('',#74908);
#2895=VERTEX_POINT('',#75179);
#2896=VERTEX_POINT('',#75180);
#2897=VERTEX_POINT('',#75182);
#2898=VERTEX_POINT('',#75192);
#2899=VERTEX_POINT('',#75199);
#2900=VERTEX_POINT('',#75201);
#2901=VERTEX_POINT('',#75219);
#2902=VERTEX_POINT('',#75220);
#2903=VERTEX_POINT('',#75222);
#2904=VERTEX_POINT('',#75231);
#2905=VERTEX_POINT('',#75278);
#2906=VERTEX_POINT('',#75279);
#2907=VERTEX_POINT('',#75530);
#2908=VERTEX_POINT('',#75531);
#2909=VERTEX_POINT('',#75533);
#2910=VERTEX_POINT('',#75561);
#2911=VERTEX_POINT('',#75825);
#2912=VERTEX_POINT('',#75826);
#2913=VERTEX_POINT('',#75828);
#2914=VERTEX_POINT('',#76084);
#2915=VERTEX_POINT('',#76214);
#2916=VERTEX_POINT('',#76215);
#2917=VERTEX_POINT('',#76217);
#2918=VERTEX_POINT('',#76472);
#2919=VERTEX_POINT('',#76473);
#2920=VERTEX_POINT('',#76591);
#2921=VERTEX_POINT('',#76619);
#2922=VERTEX_POINT('',#76620);
#2923=VERTEX_POINT('',#76622);
#2924=VERTEX_POINT('',#76757);
#2925=VERTEX_POINT('',#77013);
#2926=VERTEX_POINT('',#77014);
#2927=VERTEX_POINT('',#77136);
#2928=VERTEX_POINT('',#77170);
#2929=VERTEX_POINT('',#77171);
#2930=VERTEX_POINT('',#77173);
#2931=VERTEX_POINT('',#77298);
#2932=VERTEX_POINT('',#77552);
#2933=VERTEX_POINT('',#77553);
#2934=VERTEX_POINT('',#77555);
#2935=VERTEX_POINT('',#77634);
#2936=VERTEX_POINT('',#77636);
#2937=VERTEX_POINT('',#78005);
#2938=VERTEX_POINT('',#78144);
#2939=VERTEX_POINT('',#78165);
#2940=VERTEX_POINT('',#78273);
#2941=VERTEX_POINT('',#78275);
#2942=VERTEX_POINT('',#78279);
#2943=VERTEX_POINT('',#78281);
#2944=VERTEX_POINT('',#78816);
#2945=VERTEX_POINT('',#79805);
#2946=VERTEX_POINT('',#79806);
#2947=VERTEX_POINT('',#79808);
#2948=VERTEX_POINT('',#79810);
#2949=VERTEX_POINT('',#79813);
#2950=VERTEX_POINT('',#79815);
#2951=VERTEX_POINT('',#79818);
#2952=VERTEX_POINT('',#79822);
#2953=VERTEX_POINT('',#79826);
#2954=VERTEX_POINT('',#79827);
#2955=VERTEX_POINT('',#79832);
#2956=VERTEX_POINT('',#79836);
#2957=VERTEX_POINT('',#79844);
#2958=VERTEX_POINT('',#79845);
#2959=VERTEX_POINT('',#79847);
#2960=VERTEX_POINT('',#79854);
#2961=VERTEX_POINT('',#79951);
#2962=VERTEX_POINT('',#79952);
#2963=VERTEX_POINT('',#79954);
#2964=VERTEX_POINT('',#80097);
#2965=VERTEX_POINT('',#80317);
#2966=VERTEX_POINT('',#80318);
#2967=VERTEX_POINT('',#80320);
#2968=VERTEX_POINT('',#80405);
#2969=VERTEX_POINT('',#80619);
#2970=VERTEX_POINT('',#80620);
#2971=VERTEX_POINT('',#80622);
#2972=VERTEX_POINT('',#80769);
#2973=VERTEX_POINT('',#80983);
#2974=VERTEX_POINT('',#80984);
#2975=VERTEX_POINT('',#80986);
#2976=VERTEX_POINT('',#81199);
#2977=VERTEX_POINT('',#81288);
#2978=VERTEX_POINT('',#81289);
#2979=VERTEX_POINT('',#81291);
#2980=VERTEX_POINT('',#81368);
#2981=VERTEX_POINT('',#81374);
#2982=VERTEX_POINT('',#81376);
#2983=VERTEX_POINT('',#81449);
#2984=VERTEX_POINT('',#81450);
#2985=VERTEX_POINT('',#81452);
#2986=VERTEX_POINT('',#81459);
#2987=VERTEX_POINT('',#81556);
#2988=VERTEX_POINT('',#81557);
#2989=VERTEX_POINT('',#81559);
#2990=VERTEX_POINT('',#81702);
#2991=VERTEX_POINT('',#81922);
#2992=VERTEX_POINT('',#81923);
#2993=VERTEX_POINT('',#81925);
#2994=VERTEX_POINT('',#82010);
#2995=VERTEX_POINT('',#82224);
#2996=VERTEX_POINT('',#82225);
#2997=VERTEX_POINT('',#82227);
#2998=VERTEX_POINT('',#82374);
#2999=VERTEX_POINT('',#82588);
#3000=VERTEX_POINT('',#82589);
#3001=VERTEX_POINT('',#82591);
#3002=VERTEX_POINT('',#82804);
#3003=VERTEX_POINT('',#82893);
#3004=VERTEX_POINT('',#82894);
#3005=VERTEX_POINT('',#82896);
#3006=VERTEX_POINT('',#82973);
#3007=VERTEX_POINT('',#82979);
#3008=VERTEX_POINT('',#82981);
#3009=VERTEX_POINT('',#83054);
#3010=VERTEX_POINT('',#83055);
#3011=VERTEX_POINT('',#83057);
#3012=VERTEX_POINT('',#83068);
#3013=VERTEX_POINT('',#83127);
#3014=VERTEX_POINT('',#83128);
#3015=VERTEX_POINT('',#83130);
#3016=VERTEX_POINT('',#83479);
#3017=VERTEX_POINT('',#83480);
#3018=VERTEX_POINT('',#83482);
#3019=VERTEX_POINT('',#83683);
#3020=VERTEX_POINT('',#83845);
#3021=VERTEX_POINT('',#83846);
#3022=VERTEX_POINT('',#83848);
#3023=VERTEX_POINT('',#84033);
#3024=VERTEX_POINT('',#84034);
#3025=VERTEX_POINT('',#84036);
#3026=VERTEX_POINT('',#84222);
#3027=VERTEX_POINT('',#84244);
#3028=VERTEX_POINT('',#84245);
#3029=VERTEX_POINT('',#84247);
#3030=VERTEX_POINT('',#84261);
#3031=VERTEX_POINT('',#84380);
#3032=VERTEX_POINT('',#84382);
#3033=VERTEX_POINT('',#84569);
#3034=VERTEX_POINT('',#84570);
#3035=VERTEX_POINT('',#84572);
#3036=VERTEX_POINT('',#84583);
#3037=VERTEX_POINT('',#84642);
#3038=VERTEX_POINT('',#84643);
#3039=VERTEX_POINT('',#84645);
#3040=VERTEX_POINT('',#84994);
#3041=VERTEX_POINT('',#84995);
#3042=VERTEX_POINT('',#84997);
#3043=VERTEX_POINT('',#85198);
#3044=VERTEX_POINT('',#85362);
#3045=VERTEX_POINT('',#85363);
#3046=VERTEX_POINT('',#85365);
#3047=VERTEX_POINT('',#85550);
#3048=VERTEX_POINT('',#85551);
#3049=VERTEX_POINT('',#85553);
#3050=VERTEX_POINT('',#85739);
#3051=VERTEX_POINT('',#85761);
#3052=VERTEX_POINT('',#85762);
#3053=VERTEX_POINT('',#85764);
#3054=VERTEX_POINT('',#85778);
#3055=VERTEX_POINT('',#85897);
#3056=VERTEX_POINT('',#85899);
#3057=VERTEX_POINT('',#86086);
#3058=VERTEX_POINT('',#86284);
#3059=VERTEX_POINT('',#86471);
#3060=VERTEX_POINT('',#86669);
#3061=VERTEX_POINT('',#86856);
#3062=VERTEX_POINT('',#86941);
#3063=VERTEX_POINT('',#87085);
#3064=VERTEX_POINT('',#87170);
#3065=VERTEX_POINT('',#87485);
#3066=VERTEX_POINT('',#88021);
#3067=VERTEX_POINT('',#88022);
#3068=VERTEX_POINT('',#88024);
#3069=VERTEX_POINT('',#88026);
#3070=VERTEX_POINT('',#88211);
#3071=VERTEX_POINT('',#88385);
#3072=VERTEX_POINT('',#88745);
#3073=VERTEX_POINT('',#88749);
#3074=VERTEX_POINT('',#88750);
#3075=VERTEX_POINT('',#88755);
#3076=VERTEX_POINT('',#88759);
#3077=VERTEX_POINT('',#88767);
#3078=VERTEX_POINT('',#88769);
#3079=VERTEX_POINT('',#88773);
#3080=VERTEX_POINT('',#88776);
#3081=VERTEX_POINT('',#88779);
#3082=VERTEX_POINT('',#88783);
#3083=VERTEX_POINT('',#88785);
#3084=VERTEX_POINT('',#88788);
#3085=VERTEX_POINT('',#88797);
#3086=VERTEX_POINT('',#88798);
#3087=VERTEX_POINT('',#88800);
#3088=VERTEX_POINT('',#88802);
#3089=VERTEX_POINT('',#88806);
#3090=VERTEX_POINT('',#88807);
#3091=VERTEX_POINT('',#88809);
#3092=VERTEX_POINT('',#88811);
#3093=VERTEX_POINT('',#88824);
#3094=VERTEX_POINT('',#88826);
#3095=VERTEX_POINT('',#88830);
#3096=VERTEX_POINT('',#88832);
#3097=VERTEX_POINT('',#88839);
#3098=VERTEX_POINT('',#88841);
#3099=VERTEX_POINT('',#88845);
#3100=VERTEX_POINT('',#88847);
#3101=VERTEX_POINT('',#88854);
#3102=VERTEX_POINT('',#88855);
#3103=VERTEX_POINT('',#88857);
#3104=VERTEX_POINT('',#89028);
#3105=VERTEX_POINT('',#89155);
#3106=VERTEX_POINT('',#89156);
#3107=VERTEX_POINT('',#89410);
#3108=VERTEX_POINT('',#89620);
#3109=VERTEX_POINT('',#89621);
#3110=VERTEX_POINT('',#89623);
#3111=VERTEX_POINT('',#90043);
#3112=VERTEX_POINT('',#90044);
#3113=VERTEX_POINT('',#90270);
#3114=VERTEX_POINT('',#90286);
#3115=VERTEX_POINT('',#90287);
#3116=VERTEX_POINT('',#90289);
#3117=VERTEX_POINT('',#90304);
#3118=VERTEX_POINT('',#90526);
#3119=VERTEX_POINT('',#90527);
#3120=VERTEX_POINT('',#90529);
#3121=VERTEX_POINT('',#90930);
#3122=VERTEX_POINT('',#90931);
#3123=VERTEX_POINT('',#90933);
#3124=VERTEX_POINT('',#91214);
#3125=VERTEX_POINT('',#91460);
#3126=VERTEX_POINT('',#91461);
#3127=VERTEX_POINT('',#91978);
#3128=VERTEX_POINT('',#91979);
#3129=VERTEX_POINT('',#91981);
#3130=VERTEX_POINT('',#92198);
#3131=VERTEX_POINT('',#92424);
#3132=VERTEX_POINT('',#92425);
#3133=VERTEX_POINT('',#92866);
#3134=VERTEX_POINT('',#92867);
#3135=VERTEX_POINT('',#92869);
#3136=VERTEX_POINT('',#92896);
#3137=VERTEX_POINT('',#92912);
#3138=VERTEX_POINT('',#92913);
#3139=VERTEX_POINT('',#92915);
#3140=VERTEX_POINT('',#93110);
#3141=VERTEX_POINT('',#93377);
#3142=VERTEX_POINT('',#93378);
#3143=VERTEX_POINT('',#93380);
#3144=VERTEX_POINT('',#93852);
#3145=VERTEX_POINT('',#93853);
#3146=VERTEX_POINT('',#94085);
#3147=VERTEX_POINT('',#94299);
#3148=VERTEX_POINT('',#94300);
#3149=VERTEX_POINT('',#94302);
#3150=VERTEX_POINT('',#94748);
#3151=VERTEX_POINT('',#94749);
#3152=VERTEX_POINT('',#94979);
#3153=VERTEX_POINT('',#95199);
#3154=VERTEX_POINT('',#95200);
#3155=VERTEX_POINT('',#95202);
#3156=VERTEX_POINT('',#95628);
#3157=VERTEX_POINT('',#95629);
#3158=VERTEX_POINT('',#95883);
#3159=VERTEX_POINT('',#95900);
#3160=VERTEX_POINT('',#95901);
#3161=VERTEX_POINT('',#95903);
#3162=VERTEX_POINT('',#96130);
#3163=VERTEX_POINT('',#96344);
#3164=VERTEX_POINT('',#96345);
#3165=VERTEX_POINT('',#96812);
#3166=VERTEX_POINT('',#96813);
#3167=VERTEX_POINT('',#96815);
#3168=VERTEX_POINT('',#97034);
#3169=VERTEX_POINT('',#97258);
#3170=VERTEX_POINT('',#97259);
#3171=VERTEX_POINT('',#97684);
#3172=VERTEX_POINT('',#97685);
#3173=VERTEX_POINT('',#97687);
#3174=VERTEX_POINT('',#97934);
#3175=VERTEX_POINT('',#98150);
#3176=VERTEX_POINT('',#98151);
#3177=VERTEX_POINT('',#98676);
#3178=VERTEX_POINT('',#98677);
#3179=VERTEX_POINT('',#98684);
#3180=VERTEX_POINT('',#98686);
#3181=VERTEX_POINT('',#98724);
#3182=VERTEX_POINT('',#98933);
#3183=VERTEX_POINT('',#98944);
#3184=VERTEX_POINT('',#99153);
#3185=VERTEX_POINT('',#99166);
#3186=VERTEX_POINT('',#99375);
#3187=VERTEX_POINT('',#99386);
#3188=VERTEX_POINT('',#99398);
#3189=VERTEX_POINT('',#99409);
#3190=VERTEX_POINT('',#99618);
#3191=VERTEX_POINT('',#99830);
#3192=VERTEX_POINT('',#100039);
#3193=VERTEX_POINT('',#100050);
#3194=VERTEX_POINT('',#100061);
#3195=VERTEX_POINT('',#100270);
#3196=VERTEX_POINT('',#100281);
#3197=VERTEX_POINT('',#100493);
#3198=VERTEX_POINT('',#100505);
#3199=VERTEX_POINT('',#100714);
#3200=VERTEX_POINT('',#100725);
#3201=VERTEX_POINT('',#100934);
#3202=VERTEX_POINT('',#100946);
#3203=VERTEX_POINT('',#101158);
#3204=VERTEX_POINT('',#101169);
#3205=VERTEX_POINT('',#101180);
#3206=VERTEX_POINT('',#101182);
#3207=VERTEX_POINT('',#101334);
#3208=VERTEX_POINT('',#101345);
#3209=VERTEX_POINT('',#101554);
#3210=VERTEX_POINT('',#101766);
#3211=VERTEX_POINT('',#101975);
#3212=VERTEX_POINT('',#102187);
#3213=VERTEX_POINT('',#102198);
#3214=VERTEX_POINT('',#102407);
#3215=VERTEX_POINT('',#102418);
#3216=VERTEX_POINT('',#102429);
#3217=VERTEX_POINT('',#102638);
#3218=VERTEX_POINT('',#102649);
#3219=VERTEX_POINT('',#102858);
#3220=VERTEX_POINT('',#102869);
#3221=VERTEX_POINT('',#103081);
#3222=VERTEX_POINT('',#103092);
#3223=VERTEX_POINT('',#103103);
#3224=VERTEX_POINT('',#103309);
#3225=VERTEX_POINT('',#103320);
#3226=VERTEX_POINT('',#103529);
#3227=VERTEX_POINT('',#103541);
#3228=VERTEX_POINT('',#103750);
#3229=VERTEX_POINT('',#103772);
#3230=VERTEX_POINT('',#103777);
#3231=VERTEX_POINT('',#103962);
#3232=VERTEX_POINT('',#103964);
#3233=VERTEX_POINT('',#104120);
#3234=VERTEX_POINT('',#104217);
#3235=VERTEX_POINT('',#104253);
#3236=VERTEX_POINT('',#105619);
#3237=VERTEX_POINT('',#105713);
#3238=VERTEX_POINT('',#105714);
#3239=VERTEX_POINT('',#105716);
#3240=VERTEX_POINT('',#105718);
#3241=VERTEX_POINT('',#105722);
#3242=VERTEX_POINT('',#105724);
#3243=VERTEX_POINT('',#105728);
#3244=VERTEX_POINT('',#105730);
#3245=VERTEX_POINT('',#105734);
#3246=VERTEX_POINT('',#105736);
#3247=VERTEX_POINT('',#105740);
#3248=VERTEX_POINT('',#105742);
#3249=VERTEX_POINT('',#105750);
#3250=VERTEX_POINT('',#105753);
#3251=EDGE_CURVE('',#2326,#2326,#2228,.T.);
#3252=EDGE_CURVE('',#2326,#2327,#1668,.T.);
#3253=EDGE_CURVE('',#2327,#2327,#2229,.T.);
#3254=EDGE_CURVE('',#2328,#2328,#2230,.T.);
#3255=EDGE_CURVE('',#2328,#2329,#1669,.T.);
#3256=EDGE_CURVE('',#2329,#2329,#2231,.T.);
#3257=EDGE_CURVE('',#2330,#2330,#2232,.T.);
#3258=EDGE_CURVE('',#2330,#2331,#1670,.T.);
#3259=EDGE_CURVE('',#2331,#2331,#2233,.T.);
#3260=EDGE_CURVE('',#2332,#2332,#2234,.T.);
#3261=EDGE_CURVE('',#2332,#2333,#1671,.T.);
#3262=EDGE_CURVE('',#2333,#2333,#2235,.T.);
#3263=EDGE_CURVE('',#2334,#2335,#1672,.F.);
#3264=EDGE_CURVE('',#2335,#2336,#1673,.T.);
#3265=EDGE_CURVE('',#2337,#2336,#1674,.F.);
#3266=EDGE_CURVE('',#2334,#2337,#1675,.F.);
#3267=EDGE_CURVE('',#2338,#2334,#1676,.F.);
#3268=EDGE_CURVE('',#2339,#2337,#1677,.F.);
#3269=EDGE_CURVE('',#2338,#2339,#1678,.F.);
#3270=EDGE_CURVE('',#2340,#2338,#1679,.F.);
#3271=EDGE_CURVE('',#2341,#2339,#1680,.F.);
#3272=EDGE_CURVE('',#2340,#2341,#1681,.T.);
#3273=EDGE_CURVE('',#2335,#2340,#1682,.F.);
#3274=EDGE_CURVE('',#2336,#2341,#1683,.F.);
#3275=EDGE_CURVE('',#2342,#2342,#2236,.T.);
#3276=EDGE_CURVE('',#2342,#2343,#1684,.T.);
#3277=EDGE_CURVE('',#2343,#2343,#2237,.T.);
#3278=EDGE_CURVE('',#2344,#2344,#2238,.T.);
#3279=EDGE_CURVE('',#2344,#2345,#1685,.T.);
#3280=EDGE_CURVE('',#2345,#2345,#2239,.T.);
#3281=EDGE_CURVE('',#2346,#2346,#2240,.T.);
#3282=EDGE_CURVE('',#2346,#2347,#1686,.T.);
#3283=EDGE_CURVE('',#2347,#2347,#2241,.T.);
#3284=EDGE_CURVE('',#2348,#2348,#2242,.T.);
#3285=EDGE_CURVE('',#2348,#2349,#1687,.T.);
#3286=EDGE_CURVE('',#2349,#2349,#2243,.T.);
#3287=EDGE_CURVE('',#2350,#2350,#2244,.T.);
#3288=EDGE_CURVE('',#2350,#2351,#1688,.T.);
#3289=EDGE_CURVE('',#2351,#2351,#2245,.T.);
#3290=EDGE_CURVE('',#2352,#2353,#1689,.F.);
#3291=EDGE_CURVE('',#2353,#2354,#1690,.T.);
#3292=EDGE_CURVE('',#2355,#2354,#1691,.F.);
#3293=EDGE_CURVE('',#2352,#2355,#1692,.F.);
#3294=EDGE_CURVE('',#2356,#2352,#1693,.T.);
#3295=EDGE_CURVE('',#2357,#2355,#1694,.T.);
#3296=EDGE_CURVE('',#2356,#2357,#1695,.T.);
#3297=EDGE_CURVE('',#2358,#2356,#1696,.T.);
#3298=EDGE_CURVE('',#2359,#2357,#1697,.T.);
#3299=EDGE_CURVE('',#2358,#2359,#1698,.T.);
#3300=EDGE_CURVE('',#2353,#2358,#1699,.T.);
#3301=EDGE_CURVE('',#2354,#2359,#1700,.T.);
#3302=EDGE_CURVE('',#2360,#2360,#2246,.T.);
#3303=EDGE_CURVE('',#2360,#2361,#1701,.T.);
#3304=EDGE_CURVE('',#2361,#2361,#2247,.T.);
#3305=EDGE_CURVE('',#2362,#2362,#2248,.T.);
#3306=EDGE_CURVE('',#2362,#2363,#1702,.T.);
#3307=EDGE_CURVE('',#2363,#2363,#2249,.T.);
#3308=EDGE_CURVE('',#2364,#2365,#1703,.T.);
#3309=EDGE_CURVE('',#2366,#2364,#109,.T.);
#3310=EDGE_CURVE('',#2367,#2366,#2250,.T.);
#3311=EDGE_CURVE('',#2367,#2365,#110,.T.);
#3312=EDGE_CURVE('',#2368,#2369,#1704,.T.);
#3313=EDGE_CURVE('',#2370,#2368,#111,.T.);
#3314=EDGE_CURVE('',#2364,#2370,#112,.T.);
#3315=EDGE_CURVE('',#2365,#2371,#113,.T.);
#3316=EDGE_CURVE('',#2371,#2369,#114,.T.);
#3317=EDGE_CURVE('',#2372,#2373,#1705,.T.);
#3318=EDGE_CURVE('',#2374,#2372,#115,.T.);
#3319=EDGE_CURVE('',#2368,#2374,#116,.T.);
#3320=EDGE_CURVE('',#2369,#2375,#117,.T.);
#3321=EDGE_CURVE('',#2375,#2373,#118,.T.);
#3322=EDGE_CURVE('',#2376,#2377,#1706,.T.);
#3323=EDGE_CURVE('',#2378,#2376,#119,.T.);
#3324=EDGE_CURVE('',#2372,#2378,#120,.T.);
#3325=EDGE_CURVE('',#2373,#2379,#121,.T.);
#3326=EDGE_CURVE('',#2379,#2377,#122,.T.);
#3327=EDGE_CURVE('',#2380,#2381,#1707,.T.);
#3328=EDGE_CURVE('',#2382,#2380,#123,.T.);
#3329=EDGE_CURVE('',#2376,#2382,#124,.T.);
#3330=EDGE_CURVE('',#2377,#2383,#125,.T.);
#3331=EDGE_CURVE('',#2383,#2381,#126,.T.);
#3332=EDGE_CURVE('',#2384,#2385,#1708,.T.);
#3333=EDGE_CURVE('',#2386,#2384,#127,.T.);
#3334=EDGE_CURVE('',#2380,#2386,#128,.T.);
#3335=EDGE_CURVE('',#2381,#2387,#129,.T.);
#3336=EDGE_CURVE('',#2387,#2385,#130,.T.);
#3337=EDGE_CURVE('',#2388,#2389,#1709,.T.);
#3338=EDGE_CURVE('',#2390,#2388,#131,.T.);
#3339=EDGE_CURVE('',#2384,#2390,#132,.T.);
#3340=EDGE_CURVE('',#2385,#2391,#133,.T.);
#3341=EDGE_CURVE('',#2391,#2389,#134,.T.);
#3342=EDGE_CURVE('',#2392,#2393,#1710,.T.);
#3343=EDGE_CURVE('',#2394,#2392,#135,.T.);
#3344=EDGE_CURVE('',#2388,#2394,#136,.T.);
#3345=EDGE_CURVE('',#2389,#2395,#137,.T.);
#3346=EDGE_CURVE('',#2395,#2393,#138,.T.);
#3347=EDGE_CURVE('',#2396,#2397,#1711,.T.);
#3348=EDGE_CURVE('',#2398,#2396,#139,.T.);
#3349=EDGE_CURVE('',#2392,#2398,#140,.T.);
#3350=EDGE_CURVE('',#2393,#2399,#141,.T.);
#3351=EDGE_CURVE('',#2399,#2397,#142,.T.);
#3352=EDGE_CURVE('',#2400,#2401,#1712,.T.);
#3353=EDGE_CURVE('',#2402,#2400,#143,.T.);
#3354=EDGE_CURVE('',#2396,#2402,#144,.T.);
#3355=EDGE_CURVE('',#2397,#2403,#145,.T.);
#3356=EDGE_CURVE('',#2403,#2401,#146,.T.);
#3357=EDGE_CURVE('',#2404,#2405,#1713,.T.);
#3358=EDGE_CURVE('',#2406,#2404,#147,.T.);
#3359=EDGE_CURVE('',#2400,#2406,#148,.T.);
#3360=EDGE_CURVE('',#2401,#2407,#149,.T.);
#3361=EDGE_CURVE('',#2407,#2405,#150,.T.);
#3362=EDGE_CURVE('',#2408,#2409,#1714,.T.);
#3363=EDGE_CURVE('',#2410,#2408,#151,.T.);
#3364=EDGE_CURVE('',#2404,#2410,#152,.T.);
#3365=EDGE_CURVE('',#2405,#2411,#153,.T.);
#3366=EDGE_CURVE('',#2411,#2409,#154,.T.);
#3367=EDGE_CURVE('',#2412,#2413,#1715,.T.);
#3368=EDGE_CURVE('',#2414,#2412,#155,.T.);
#3369=EDGE_CURVE('',#2408,#2414,#156,.T.);
#3370=EDGE_CURVE('',#2409,#2415,#157,.T.);
#3371=EDGE_CURVE('',#2415,#2413,#158,.T.);
#3372=EDGE_CURVE('',#2416,#2417,#1716,.T.);
#3373=EDGE_CURVE('',#2418,#2416,#159,.T.);
#3374=EDGE_CURVE('',#2412,#2418,#160,.T.);
#3375=EDGE_CURVE('',#2413,#2419,#161,.T.);
#3376=EDGE_CURVE('',#2419,#2417,#162,.T.);
#3377=EDGE_CURVE('',#2420,#2421,#1717,.T.);
#3378=EDGE_CURVE('',#2422,#2420,#163,.T.);
#3379=EDGE_CURVE('',#2416,#2422,#164,.T.);
#3380=EDGE_CURVE('',#2417,#2423,#165,.T.);
#3381=EDGE_CURVE('',#2423,#2421,#166,.T.);
#3382=EDGE_CURVE('',#2424,#2425,#1718,.T.);
#3383=EDGE_CURVE('',#2426,#2424,#167,.T.);
#3384=EDGE_CURVE('',#2420,#2426,#168,.T.);
#3385=EDGE_CURVE('',#2421,#2427,#169,.T.);
#3386=EDGE_CURVE('',#2427,#2425,#170,.T.);
#3387=EDGE_CURVE('',#2428,#2429,#1719,.T.);
#3388=EDGE_CURVE('',#2430,#2428,#171,.T.);
#3389=EDGE_CURVE('',#2424,#2430,#172,.T.);
#3390=EDGE_CURVE('',#2425,#2431,#173,.T.);
#3391=EDGE_CURVE('',#2431,#2429,#174,.T.);
#3392=EDGE_CURVE('',#2432,#2433,#1720,.T.);
#3393=EDGE_CURVE('',#2434,#2432,#175,.T.);
#3394=EDGE_CURVE('',#2428,#2434,#176,.T.);
#3395=EDGE_CURVE('',#2429,#2435,#177,.T.);
#3396=EDGE_CURVE('',#2435,#2433,#178,.T.);
#3397=EDGE_CURVE('',#2436,#2437,#1721,.T.);
#3398=EDGE_CURVE('',#2438,#2436,#179,.T.);
#3399=EDGE_CURVE('',#2432,#2438,#180,.T.);
#3400=EDGE_CURVE('',#2433,#2439,#181,.T.);
#3401=EDGE_CURVE('',#2439,#2437,#182,.T.);
#3402=EDGE_CURVE('',#2440,#2441,#1722,.T.);
#3403=EDGE_CURVE('',#2442,#2440,#183,.T.);
#3404=EDGE_CURVE('',#2436,#2442,#184,.T.);
#3405=EDGE_CURVE('',#2437,#2443,#185,.T.);
#3406=EDGE_CURVE('',#2443,#2441,#186,.T.);
#3407=EDGE_CURVE('',#2444,#2445,#1723,.T.);
#3408=EDGE_CURVE('',#2446,#2444,#187,.T.);
#3409=EDGE_CURVE('',#2440,#2446,#188,.T.);
#3410=EDGE_CURVE('',#2441,#2447,#189,.T.);
#3411=EDGE_CURVE('',#2447,#2445,#190,.T.);
#3412=EDGE_CURVE('',#2448,#2449,#1724,.T.);
#3413=EDGE_CURVE('',#2450,#2448,#191,.T.);
#3414=EDGE_CURVE('',#2444,#2450,#192,.T.);
#3415=EDGE_CURVE('',#2445,#2451,#193,.T.);
#3416=EDGE_CURVE('',#2451,#2449,#194,.T.);
#3417=EDGE_CURVE('',#2452,#2453,#1725,.T.);
#3418=EDGE_CURVE('',#2454,#2452,#195,.T.);
#3419=EDGE_CURVE('',#2448,#2454,#196,.T.);
#3420=EDGE_CURVE('',#2449,#2455,#197,.T.);
#3421=EDGE_CURVE('',#2455,#2453,#198,.T.);
#3422=EDGE_CURVE('',#2456,#2457,#1726,.T.);
#3423=EDGE_CURVE('',#2458,#2456,#199,.T.);
#3424=EDGE_CURVE('',#2452,#2458,#200,.T.);
#3425=EDGE_CURVE('',#2453,#2459,#201,.T.);
#3426=EDGE_CURVE('',#2459,#2457,#202,.T.);
#3427=EDGE_CURVE('',#2460,#2461,#1727,.T.);
#3428=EDGE_CURVE('',#2462,#2460,#203,.T.);
#3429=EDGE_CURVE('',#2456,#2462,#204,.T.);
#3430=EDGE_CURVE('',#2457,#2463,#205,.T.);
#3431=EDGE_CURVE('',#2463,#2461,#206,.T.);
#3432=EDGE_CURVE('',#2464,#2465,#1728,.T.);
#3433=EDGE_CURVE('',#2466,#2464,#207,.T.);
#3434=EDGE_CURVE('',#2460,#2466,#208,.T.);
#3435=EDGE_CURVE('',#2461,#2467,#209,.T.);
#3436=EDGE_CURVE('',#2467,#2465,#210,.T.);
#3437=EDGE_CURVE('',#2468,#2469,#1729,.T.);
#3438=EDGE_CURVE('',#2470,#2468,#211,.T.);
#3439=EDGE_CURVE('',#2464,#2470,#212,.T.);
#3440=EDGE_CURVE('',#2465,#2471,#213,.T.);
#3441=EDGE_CURVE('',#2471,#2469,#214,.T.);
#3442=EDGE_CURVE('',#2472,#2473,#1730,.T.);
#3443=EDGE_CURVE('',#2474,#2472,#215,.T.);
#3444=EDGE_CURVE('',#2468,#2474,#216,.T.);
#3445=EDGE_CURVE('',#2469,#2475,#217,.T.);
#3446=EDGE_CURVE('',#2475,#2473,#218,.T.);
#3447=EDGE_CURVE('',#2476,#2477,#1731,.T.);
#3448=EDGE_CURVE('',#2478,#2476,#219,.T.);
#3449=EDGE_CURVE('',#2472,#2478,#220,.T.);
#3450=EDGE_CURVE('',#2473,#2479,#221,.T.);
#3451=EDGE_CURVE('',#2479,#2477,#222,.T.);
#3452=EDGE_CURVE('',#2480,#2481,#1732,.T.);
#3453=EDGE_CURVE('',#2482,#2480,#223,.T.);
#3454=EDGE_CURVE('',#2476,#2482,#224,.T.);
#3455=EDGE_CURVE('',#2477,#2483,#225,.T.);
#3456=EDGE_CURVE('',#2483,#2481,#226,.T.);
#3457=EDGE_CURVE('',#2484,#2485,#1733,.T.);
#3458=EDGE_CURVE('',#2486,#2484,#227,.T.);
#3459=EDGE_CURVE('',#2480,#2486,#228,.T.);
#3460=EDGE_CURVE('',#2481,#2487,#229,.T.);
#3461=EDGE_CURVE('',#2487,#2485,#230,.T.);
#3462=EDGE_CURVE('',#2488,#2489,#1734,.T.);
#3463=EDGE_CURVE('',#2490,#2488,#231,.T.);
#3464=EDGE_CURVE('',#2484,#2490,#232,.T.);
#3465=EDGE_CURVE('',#2485,#2491,#233,.T.);
#3466=EDGE_CURVE('',#2491,#2489,#234,.T.);
#3467=EDGE_CURVE('',#2492,#2493,#1735,.T.);
#3468=EDGE_CURVE('',#2494,#2492,#235,.T.);
#3469=EDGE_CURVE('',#2488,#2494,#236,.T.);
#3470=EDGE_CURVE('',#2489,#2495,#237,.T.);
#3471=EDGE_CURVE('',#2495,#2493,#238,.T.);
#3472=EDGE_CURVE('',#2496,#2497,#1736,.T.);
#3473=EDGE_CURVE('',#2498,#2496,#239,.T.);
#3474=EDGE_CURVE('',#2492,#2498,#240,.T.);
#3475=EDGE_CURVE('',#2493,#2499,#241,.T.);
#3476=EDGE_CURVE('',#2499,#2497,#242,.T.);
#3477=EDGE_CURVE('',#2500,#2501,#1737,.T.);
#3478=EDGE_CURVE('',#2502,#2500,#243,.T.);
#3479=EDGE_CURVE('',#2496,#2502,#244,.T.);
#3480=EDGE_CURVE('',#2497,#2503,#245,.T.);
#3481=EDGE_CURVE('',#2503,#2501,#246,.T.);
#3482=EDGE_CURVE('',#2504,#2505,#1738,.T.);
#3483=EDGE_CURVE('',#2506,#2504,#247,.T.);
#3484=EDGE_CURVE('',#2500,#2506,#248,.T.);
#3485=EDGE_CURVE('',#2501,#2507,#249,.T.);
#3486=EDGE_CURVE('',#2507,#2505,#250,.T.);
#3487=EDGE_CURVE('',#2508,#2509,#1739,.T.);
#3488=EDGE_CURVE('',#2510,#2508,#251,.T.);
#3489=EDGE_CURVE('',#2504,#2510,#252,.T.);
#3490=EDGE_CURVE('',#2505,#2511,#253,.T.);
#3491=EDGE_CURVE('',#2511,#2509,#254,.T.);
#3492=EDGE_CURVE('',#2512,#2513,#1740,.T.);
#3493=EDGE_CURVE('',#2514,#2512,#255,.T.);
#3494=EDGE_CURVE('',#2508,#2514,#256,.T.);
#3495=EDGE_CURVE('',#2509,#2515,#257,.T.);
#3496=EDGE_CURVE('',#2515,#2513,#258,.T.);
#3497=EDGE_CURVE('',#2516,#2517,#1741,.T.);
#3498=EDGE_CURVE('',#2518,#2516,#259,.T.);
#3499=EDGE_CURVE('',#2512,#2518,#260,.T.);
#3500=EDGE_CURVE('',#2513,#2519,#261,.T.);
#3501=EDGE_CURVE('',#2519,#2517,#262,.T.);
#3502=EDGE_CURVE('',#2520,#2521,#1742,.T.);
#3503=EDGE_CURVE('',#2522,#2520,#263,.T.);
#3504=EDGE_CURVE('',#2516,#2522,#264,.T.);
#3505=EDGE_CURVE('',#2517,#2523,#265,.T.);
#3506=EDGE_CURVE('',#2523,#2521,#266,.T.);
#3507=EDGE_CURVE('',#2524,#2525,#1743,.T.);
#3508=EDGE_CURVE('',#2526,#2524,#267,.T.);
#3509=EDGE_CURVE('',#2520,#2526,#268,.T.);
#3510=EDGE_CURVE('',#2521,#2527,#269,.T.);
#3511=EDGE_CURVE('',#2527,#2525,#270,.T.);
#3512=EDGE_CURVE('',#2528,#2529,#1744,.T.);
#3513=EDGE_CURVE('',#2530,#2528,#271,.T.);
#3514=EDGE_CURVE('',#2524,#2530,#272,.T.);
#3515=EDGE_CURVE('',#2525,#2531,#273,.T.);
#3516=EDGE_CURVE('',#2531,#2529,#274,.T.);
#3517=EDGE_CURVE('',#2532,#2533,#1745,.T.);
#3518=EDGE_CURVE('',#2534,#2532,#275,.T.);
#3519=EDGE_CURVE('',#2528,#2534,#276,.T.);
#3520=EDGE_CURVE('',#2529,#2535,#277,.T.);
#3521=EDGE_CURVE('',#2535,#2533,#278,.T.);
#3522=EDGE_CURVE('',#2536,#2537,#1746,.T.);
#3523=EDGE_CURVE('',#2538,#2536,#279,.T.);
#3524=EDGE_CURVE('',#2532,#2538,#280,.T.);
#3525=EDGE_CURVE('',#2533,#2539,#281,.T.);
#3526=EDGE_CURVE('',#2539,#2537,#282,.T.);
#3527=EDGE_CURVE('',#2540,#2541,#1747,.T.);
#3528=EDGE_CURVE('',#2542,#2540,#283,.T.);
#3529=EDGE_CURVE('',#2536,#2542,#284,.T.);
#3530=EDGE_CURVE('',#2537,#2543,#285,.T.);
#3531=EDGE_CURVE('',#2543,#2541,#286,.T.);
#3532=EDGE_CURVE('',#2544,#2545,#1748,.T.);
#3533=EDGE_CURVE('',#2546,#2544,#287,.T.);
#3534=EDGE_CURVE('',#2540,#2546,#288,.T.);
#3535=EDGE_CURVE('',#2541,#2547,#289,.T.);
#3536=EDGE_CURVE('',#2547,#2545,#290,.T.);
#3537=EDGE_CURVE('',#2548,#2549,#1749,.T.);
#3538=EDGE_CURVE('',#2550,#2548,#291,.T.);
#3539=EDGE_CURVE('',#2544,#2550,#292,.T.);
#3540=EDGE_CURVE('',#2545,#2551,#293,.T.);
#3541=EDGE_CURVE('',#2551,#2549,#294,.T.);
#3542=EDGE_CURVE('',#2552,#2553,#1750,.T.);
#3543=EDGE_CURVE('',#2554,#2552,#295,.T.);
#3544=EDGE_CURVE('',#2548,#2554,#296,.T.);
#3545=EDGE_CURVE('',#2549,#2555,#297,.T.);
#3546=EDGE_CURVE('',#2555,#2553,#298,.T.);
#3547=EDGE_CURVE('',#2556,#2557,#1751,.T.);
#3548=EDGE_CURVE('',#2558,#2556,#299,.T.);
#3549=EDGE_CURVE('',#2552,#2558,#300,.T.);
#3550=EDGE_CURVE('',#2553,#2559,#301,.T.);
#3551=EDGE_CURVE('',#2559,#2557,#302,.T.);
#3552=EDGE_CURVE('',#2560,#2561,#1752,.T.);
#3553=EDGE_CURVE('',#2562,#2560,#303,.T.);
#3554=EDGE_CURVE('',#2556,#2562,#304,.T.);
#3555=EDGE_CURVE('',#2557,#2563,#305,.T.);
#3556=EDGE_CURVE('',#2563,#2561,#306,.T.);
#3557=EDGE_CURVE('',#2564,#2565,#1753,.T.);
#3558=EDGE_CURVE('',#2566,#2564,#307,.T.);
#3559=EDGE_CURVE('',#2560,#2566,#308,.T.);
#3560=EDGE_CURVE('',#2561,#2567,#309,.T.);
#3561=EDGE_CURVE('',#2567,#2565,#310,.T.);
#3562=EDGE_CURVE('',#2568,#2569,#1754,.T.);
#3563=EDGE_CURVE('',#2570,#2568,#311,.T.);
#3564=EDGE_CURVE('',#2564,#2570,#312,.T.);
#3565=EDGE_CURVE('',#2565,#2571,#313,.T.);
#3566=EDGE_CURVE('',#2571,#2569,#314,.T.);
#3567=EDGE_CURVE('',#2572,#2573,#1755,.T.);
#3568=EDGE_CURVE('',#2574,#2572,#315,.T.);
#3569=EDGE_CURVE('',#2568,#2574,#316,.T.);
#3570=EDGE_CURVE('',#2569,#2575,#317,.T.);
#3571=EDGE_CURVE('',#2575,#2573,#318,.T.);
#3572=EDGE_CURVE('',#2576,#2577,#1756,.T.);
#3573=EDGE_CURVE('',#2578,#2576,#319,.T.);
#3574=EDGE_CURVE('',#2572,#2578,#320,.T.);
#3575=EDGE_CURVE('',#2573,#2579,#321,.T.);
#3576=EDGE_CURVE('',#2579,#2577,#322,.T.);
#3577=EDGE_CURVE('',#2580,#2581,#1757,.T.);
#3578=EDGE_CURVE('',#2582,#2580,#323,.T.);
#3579=EDGE_CURVE('',#2576,#2582,#324,.T.);
#3580=EDGE_CURVE('',#2577,#2583,#325,.T.);
#3581=EDGE_CURVE('',#2583,#2581,#326,.T.);
#3582=EDGE_CURVE('',#2584,#2585,#1758,.T.);
#3583=EDGE_CURVE('',#2586,#2584,#327,.T.);
#3584=EDGE_CURVE('',#2580,#2586,#328,.T.);
#3585=EDGE_CURVE('',#2581,#2587,#329,.T.);
#3586=EDGE_CURVE('',#2587,#2585,#330,.T.);
#3587=EDGE_CURVE('',#2588,#2589,#1759,.T.);
#3588=EDGE_CURVE('',#2590,#2588,#331,.T.);
#3589=EDGE_CURVE('',#2584,#2590,#332,.T.);
#3590=EDGE_CURVE('',#2585,#2591,#333,.T.);
#3591=EDGE_CURVE('',#2591,#2589,#334,.T.);
#3592=EDGE_CURVE('',#2592,#2593,#1760,.T.);
#3593=EDGE_CURVE('',#2594,#2592,#335,.T.);
#3594=EDGE_CURVE('',#2588,#2594,#336,.T.);
#3595=EDGE_CURVE('',#2589,#2595,#337,.T.);
#3596=EDGE_CURVE('',#2595,#2593,#338,.T.);
#3597=EDGE_CURVE('',#2596,#2597,#1761,.T.);
#3598=EDGE_CURVE('',#2598,#2596,#339,.T.);
#3599=EDGE_CURVE('',#2592,#2598,#340,.T.);
#3600=EDGE_CURVE('',#2593,#2599,#341,.T.);
#3601=EDGE_CURVE('',#2599,#2597,#342,.T.);
#3602=EDGE_CURVE('',#2600,#2601,#1762,.T.);
#3603=EDGE_CURVE('',#2602,#2600,#343,.T.);
#3604=EDGE_CURVE('',#2596,#2602,#344,.T.);
#3605=EDGE_CURVE('',#2597,#2603,#345,.T.);
#3606=EDGE_CURVE('',#2603,#2601,#346,.T.);
#3607=EDGE_CURVE('',#2604,#2605,#1763,.T.);
#3608=EDGE_CURVE('',#2606,#2604,#347,.T.);
#3609=EDGE_CURVE('',#2600,#2606,#348,.T.);
#3610=EDGE_CURVE('',#2601,#2607,#349,.T.);
#3611=EDGE_CURVE('',#2607,#2605,#350,.T.);
#3612=EDGE_CURVE('',#2608,#2609,#1764,.T.);
#3613=EDGE_CURVE('',#2610,#2608,#351,.T.);
#3614=EDGE_CURVE('',#2604,#2610,#352,.T.);
#3615=EDGE_CURVE('',#2605,#2611,#353,.T.);
#3616=EDGE_CURVE('',#2611,#2609,#354,.T.);
#3617=EDGE_CURVE('',#2612,#2613,#1765,.T.);
#3618=EDGE_CURVE('',#2614,#2612,#355,.T.);
#3619=EDGE_CURVE('',#2608,#2614,#356,.T.);
#3620=EDGE_CURVE('',#2609,#2615,#357,.T.);
#3621=EDGE_CURVE('',#2615,#2613,#358,.T.);
#3622=EDGE_CURVE('',#2616,#2617,#1766,.T.);
#3623=EDGE_CURVE('',#2618,#2616,#359,.T.);
#3624=EDGE_CURVE('',#2612,#2618,#360,.T.);
#3625=EDGE_CURVE('',#2613,#2619,#361,.T.);
#3626=EDGE_CURVE('',#2619,#2617,#362,.T.);
#3627=EDGE_CURVE('',#2620,#2621,#1767,.T.);
#3628=EDGE_CURVE('',#2622,#2620,#363,.T.);
#3629=EDGE_CURVE('',#2616,#2622,#364,.T.);
#3630=EDGE_CURVE('',#2617,#2623,#365,.T.);
#3631=EDGE_CURVE('',#2623,#2621,#366,.T.);
#3632=EDGE_CURVE('',#2624,#2625,#1768,.T.);
#3633=EDGE_CURVE('',#2626,#2624,#367,.T.);
#3634=EDGE_CURVE('',#2620,#2626,#368,.T.);
#3635=EDGE_CURVE('',#2621,#2627,#369,.T.);
#3636=EDGE_CURVE('',#2627,#2625,#370,.T.);
#3637=EDGE_CURVE('',#2628,#2629,#1769,.T.);
#3638=EDGE_CURVE('',#2630,#2628,#371,.T.);
#3639=EDGE_CURVE('',#2624,#2630,#372,.T.);
#3640=EDGE_CURVE('',#2625,#2631,#373,.T.);
#3641=EDGE_CURVE('',#2631,#2629,#374,.T.);
#3642=EDGE_CURVE('',#2632,#2633,#1770,.T.);
#3643=EDGE_CURVE('',#2634,#2632,#375,.T.);
#3644=EDGE_CURVE('',#2628,#2634,#376,.T.);
#3645=EDGE_CURVE('',#2629,#2635,#377,.T.);
#3646=EDGE_CURVE('',#2635,#2633,#378,.T.);
#3647=EDGE_CURVE('',#2636,#2637,#1771,.T.);
#3648=EDGE_CURVE('',#2638,#2636,#379,.T.);
#3649=EDGE_CURVE('',#2632,#2638,#380,.T.);
#3650=EDGE_CURVE('',#2633,#2639,#381,.T.);
#3651=EDGE_CURVE('',#2639,#2637,#382,.T.);
#3652=EDGE_CURVE('',#2640,#2641,#1772,.T.);
#3653=EDGE_CURVE('',#2642,#2640,#383,.T.);
#3654=EDGE_CURVE('',#2636,#2642,#384,.T.);
#3655=EDGE_CURVE('',#2637,#2643,#385,.T.);
#3656=EDGE_CURVE('',#2643,#2641,#386,.T.);
#3657=EDGE_CURVE('',#2644,#2645,#1773,.T.);
#3658=EDGE_CURVE('',#2646,#2644,#387,.T.);
#3659=EDGE_CURVE('',#2640,#2646,#388,.T.);
#3660=EDGE_CURVE('',#2641,#2647,#389,.T.);
#3661=EDGE_CURVE('',#2647,#2645,#390,.T.);
#3662=EDGE_CURVE('',#2648,#2649,#1774,.T.);
#3663=EDGE_CURVE('',#2650,#2648,#391,.T.);
#3664=EDGE_CURVE('',#2644,#2650,#392,.T.);
#3665=EDGE_CURVE('',#2645,#2651,#393,.T.);
#3666=EDGE_CURVE('',#2651,#2649,#394,.T.);
#3667=EDGE_CURVE('',#2652,#2653,#1775,.T.);
#3668=EDGE_CURVE('',#2654,#2652,#395,.T.);
#3669=EDGE_CURVE('',#2648,#2654,#396,.T.);
#3670=EDGE_CURVE('',#2649,#2655,#397,.T.);
#3671=EDGE_CURVE('',#2655,#2653,#398,.T.);
#3672=EDGE_CURVE('',#2656,#2657,#1776,.T.);
#3673=EDGE_CURVE('',#2658,#2656,#399,.T.);
#3674=EDGE_CURVE('',#2652,#2658,#400,.T.);
#3675=EDGE_CURVE('',#2653,#2659,#401,.T.);
#3676=EDGE_CURVE('',#2659,#2657,#402,.T.);
#3677=EDGE_CURVE('',#2660,#2661,#1777,.T.);
#3678=EDGE_CURVE('',#2662,#2660,#403,.T.);
#3679=EDGE_CURVE('',#2656,#2662,#404,.T.);
#3680=EDGE_CURVE('',#2657,#2663,#405,.T.);
#3681=EDGE_CURVE('',#2663,#2661,#406,.T.);
#3682=EDGE_CURVE('',#2664,#2665,#1778,.T.);
#3683=EDGE_CURVE('',#2666,#2664,#407,.T.);
#3684=EDGE_CURVE('',#2660,#2666,#408,.T.);
#3685=EDGE_CURVE('',#2661,#2667,#409,.T.);
#3686=EDGE_CURVE('',#2667,#2665,#410,.T.);
#3687=EDGE_CURVE('',#2668,#2669,#1779,.T.);
#3688=EDGE_CURVE('',#2670,#2668,#411,.T.);
#3689=EDGE_CURVE('',#2664,#2670,#412,.T.);
#3690=EDGE_CURVE('',#2665,#2671,#413,.T.);
#3691=EDGE_CURVE('',#2671,#2669,#414,.T.);
#3692=EDGE_CURVE('',#2669,#2672,#415,.T.);
#3693=EDGE_CURVE('',#2672,#2673,#416,.T.);
#3694=EDGE_CURVE('',#2674,#2673,#2251,.T.);
#3695=EDGE_CURVE('',#2675,#2674,#417,.T.);
#3696=EDGE_CURVE('',#2668,#2675,#418,.T.);
#3697=EDGE_CURVE('',#2676,#2677,#419,.T.);
#3698=EDGE_CURVE('',#2677,#2678,#2252,.F.);
#3699=EDGE_CURVE('',#2678,#2679,#420,.T.);
#3700=EDGE_CURVE('',#2679,#2680,#421,.T.);
#3701=EDGE_CURVE('',#2680,#2681,#422,.T.);
#3702=EDGE_CURVE('',#2681,#2682,#423,.T.);
#3703=EDGE_CURVE('',#2682,#2683,#424,.T.);
#3704=EDGE_CURVE('',#2683,#2684,#425,.T.);
#3705=EDGE_CURVE('',#2684,#2685,#426,.T.);
#3706=EDGE_CURVE('',#2685,#2686,#427,.T.);
#3707=EDGE_CURVE('',#2686,#2687,#428,.T.);
#3708=EDGE_CURVE('',#2687,#2688,#429,.T.);
#3709=EDGE_CURVE('',#2688,#2689,#430,.T.);
#3710=EDGE_CURVE('',#2689,#2690,#431,.T.);
#3711=EDGE_CURVE('',#2690,#2691,#432,.T.);
#3712=EDGE_CURVE('',#2691,#2692,#433,.T.);
#3713=EDGE_CURVE('',#2692,#2693,#434,.T.);
#3714=EDGE_CURVE('',#2693,#2694,#435,.T.);
#3715=EDGE_CURVE('',#2694,#2695,#436,.T.);
#3716=EDGE_CURVE('',#2695,#2696,#437,.T.);
#3717=EDGE_CURVE('',#2696,#2697,#438,.T.);
#3718=EDGE_CURVE('',#2697,#2698,#439,.T.);
#3719=EDGE_CURVE('',#2698,#2699,#440,.T.);
#3720=EDGE_CURVE('',#2699,#2700,#441,.T.);
#3721=EDGE_CURVE('',#2700,#2701,#442,.T.);
#3722=EDGE_CURVE('',#2701,#2702,#443,.T.);
#3723=EDGE_CURVE('',#2702,#2703,#444,.T.);
#3724=EDGE_CURVE('',#2703,#2704,#445,.T.);
#3725=EDGE_CURVE('',#2704,#2705,#446,.T.);
#3726=EDGE_CURVE('',#2705,#2706,#447,.T.);
#3727=EDGE_CURVE('',#2706,#2707,#448,.T.);
#3728=EDGE_CURVE('',#2707,#2708,#449,.T.);
#3729=EDGE_CURVE('',#2708,#2709,#450,.T.);
#3730=EDGE_CURVE('',#2709,#2710,#451,.T.);
#3731=EDGE_CURVE('',#2710,#2711,#452,.T.);
#3732=EDGE_CURVE('',#2711,#2712,#453,.T.);
#3733=EDGE_CURVE('',#2712,#2713,#454,.T.);
#3734=EDGE_CURVE('',#2713,#2714,#455,.T.);
#3735=EDGE_CURVE('',#2714,#2715,#456,.T.);
#3736=EDGE_CURVE('',#2715,#2716,#457,.T.);
#3737=EDGE_CURVE('',#2716,#2717,#458,.T.);
#3738=EDGE_CURVE('',#2717,#2718,#459,.T.);
#3739=EDGE_CURVE('',#2718,#2719,#460,.T.);
#3740=EDGE_CURVE('',#2719,#2720,#461,.T.);
#3741=EDGE_CURVE('',#2720,#2721,#462,.T.);
#3742=EDGE_CURVE('',#2721,#2722,#463,.T.);
#3743=EDGE_CURVE('',#2722,#2723,#464,.T.);
#3744=EDGE_CURVE('',#2723,#2724,#465,.T.);
#3745=EDGE_CURVE('',#2724,#2725,#466,.T.);
#3746=EDGE_CURVE('',#2725,#2726,#467,.T.);
#3747=EDGE_CURVE('',#2726,#2727,#468,.T.);
#3748=EDGE_CURVE('',#2727,#2728,#469,.T.);
#3749=EDGE_CURVE('',#2728,#2729,#470,.T.);
#3750=EDGE_CURVE('',#2729,#2730,#471,.T.);
#3751=EDGE_CURVE('',#2730,#2731,#472,.T.);
#3752=EDGE_CURVE('',#2731,#2732,#473,.T.);
#3753=EDGE_CURVE('',#2732,#2733,#474,.T.);
#3754=EDGE_CURVE('',#2733,#2734,#475,.T.);
#3755=EDGE_CURVE('',#2734,#2735,#476,.T.);
#3756=EDGE_CURVE('',#2735,#2736,#477,.T.);
#3757=EDGE_CURVE('',#2736,#2737,#478,.T.);
#3758=EDGE_CURVE('',#2737,#2738,#479,.T.);
#3759=EDGE_CURVE('',#2738,#2739,#480,.T.);
#3760=EDGE_CURVE('',#2739,#2740,#481,.T.);
#3761=EDGE_CURVE('',#2740,#2741,#482,.T.);
#3762=EDGE_CURVE('',#2741,#2742,#483,.T.);
#3763=EDGE_CURVE('',#2742,#2743,#484,.T.);
#3764=EDGE_CURVE('',#2743,#2744,#485,.T.);
#3765=EDGE_CURVE('',#2744,#2745,#486,.T.);
#3766=EDGE_CURVE('',#2745,#2746,#487,.T.);
#3767=EDGE_CURVE('',#2746,#2747,#488,.T.);
#3768=EDGE_CURVE('',#2747,#2748,#489,.T.);
#3769=EDGE_CURVE('',#2748,#2749,#490,.T.);
#3770=EDGE_CURVE('',#2749,#2750,#491,.T.);
#3771=EDGE_CURVE('',#2750,#2751,#492,.T.);
#3772=EDGE_CURVE('',#2751,#2752,#493,.T.);
#3773=EDGE_CURVE('',#2752,#2753,#494,.T.);
#3774=EDGE_CURVE('',#2753,#2754,#495,.T.);
#3775=EDGE_CURVE('',#2754,#2755,#496,.T.);
#3776=EDGE_CURVE('',#2755,#2756,#497,.T.);
#3777=EDGE_CURVE('',#2756,#2757,#2253,.T.);
#3778=EDGE_CURVE('',#2757,#2758,#498,.T.);
#3779=EDGE_CURVE('',#2758,#2759,#499,.T.);
#3780=EDGE_CURVE('',#2759,#2760,#500,.T.);
#3781=EDGE_CURVE('',#2760,#2761,#501,.T.);
#3782=EDGE_CURVE('',#2761,#2762,#502,.T.);
#3783=EDGE_CURVE('',#2762,#2763,#503,.T.);
#3784=EDGE_CURVE('',#2763,#2764,#504,.T.);
#3785=EDGE_CURVE('',#2764,#2765,#505,.T.);
#3786=EDGE_CURVE('',#2765,#2766,#506,.T.);
#3787=EDGE_CURVE('',#2766,#2767,#507,.T.);
#3788=EDGE_CURVE('',#2767,#2768,#508,.T.);
#3789=EDGE_CURVE('',#2768,#2769,#509,.T.);
#3790=EDGE_CURVE('',#2769,#2770,#510,.T.);
#3791=EDGE_CURVE('',#2770,#2771,#511,.T.);
#3792=EDGE_CURVE('',#2771,#2772,#512,.T.);
#3793=EDGE_CURVE('',#2772,#2773,#513,.T.);
#3794=EDGE_CURVE('',#2773,#2774,#514,.T.);
#3795=EDGE_CURVE('',#2774,#2775,#515,.T.);
#3796=EDGE_CURVE('',#2775,#2776,#516,.T.);
#3797=EDGE_CURVE('',#2776,#2777,#517,.T.);
#3798=EDGE_CURVE('',#2777,#2778,#518,.T.);
#3799=EDGE_CURVE('',#2778,#2779,#519,.T.);
#3800=EDGE_CURVE('',#2779,#2780,#520,.T.);
#3801=EDGE_CURVE('',#2780,#2781,#521,.T.);
#3802=EDGE_CURVE('',#2781,#2782,#522,.T.);
#3803=EDGE_CURVE('',#2782,#2783,#523,.T.);
#3804=EDGE_CURVE('',#2783,#2784,#524,.T.);
#3805=EDGE_CURVE('',#2784,#2785,#525,.T.);
#3806=EDGE_CURVE('',#2785,#2786,#526,.T.);
#3807=EDGE_CURVE('',#2786,#2787,#527,.T.);
#3808=EDGE_CURVE('',#2787,#2788,#528,.T.);
#3809=EDGE_CURVE('',#2788,#2789,#529,.T.);
#3810=EDGE_CURVE('',#2789,#2790,#530,.T.);
#3811=EDGE_CURVE('',#2790,#2791,#531,.T.);
#3812=EDGE_CURVE('',#2791,#2792,#532,.T.);
#3813=EDGE_CURVE('',#2792,#2793,#533,.T.);
#3814=EDGE_CURVE('',#2793,#2794,#534,.T.);
#3815=EDGE_CURVE('',#2794,#2795,#535,.T.);
#3816=EDGE_CURVE('',#2795,#2796,#536,.T.);
#3817=EDGE_CURVE('',#2796,#2797,#537,.T.);
#3818=EDGE_CURVE('',#2797,#2798,#538,.T.);
#3819=EDGE_CURVE('',#2798,#2799,#539,.T.);
#3820=EDGE_CURVE('',#2799,#2800,#540,.T.);
#3821=EDGE_CURVE('',#2800,#2801,#541,.T.);
#3822=EDGE_CURVE('',#2801,#2802,#542,.T.);
#3823=EDGE_CURVE('',#2802,#2803,#543,.T.);
#3824=EDGE_CURVE('',#2803,#2804,#544,.T.);
#3825=EDGE_CURVE('',#2804,#2805,#545,.T.);
#3826=EDGE_CURVE('',#2805,#2806,#546,.T.);
#3827=EDGE_CURVE('',#2806,#2807,#547,.T.);
#3828=EDGE_CURVE('',#2807,#2808,#548,.T.);
#3829=EDGE_CURVE('',#2808,#2809,#549,.T.);
#3830=EDGE_CURVE('',#2809,#2810,#550,.T.);
#3831=EDGE_CURVE('',#2810,#2811,#551,.T.);
#3832=EDGE_CURVE('',#2811,#2812,#552,.T.);
#3833=EDGE_CURVE('',#2812,#2813,#553,.T.);
#3834=EDGE_CURVE('',#2813,#2814,#554,.T.);
#3835=EDGE_CURVE('',#2814,#2815,#555,.T.);
#3836=EDGE_CURVE('',#2815,#2816,#556,.T.);
#3837=EDGE_CURVE('',#2816,#2817,#557,.T.);
#3838=EDGE_CURVE('',#2817,#2818,#558,.T.);
#3839=EDGE_CURVE('',#2818,#2676,#559,.T.);
#3840=EDGE_CURVE('',#2819,#2819,#2254,.T.);
#3841=EDGE_CURVE('',#2819,#2820,#1780,.T.);
#3842=EDGE_CURVE('',#2820,#2820,#2255,.T.);
#3843=EDGE_CURVE('',#2821,#2821,#2256,.T.);
#3844=EDGE_CURVE('',#2822,#2822,#2257,.T.);
#3845=EDGE_CURVE('',#2823,#2823,#2258,.T.);
#3846=EDGE_CURVE('',#2823,#2822,#1781,.T.);
#3847=EDGE_CURVE('',#2821,#2824,#1782,.T.);
#3848=EDGE_CURVE('',#2824,#2824,#2259,.T.);
#3849=EDGE_CURVE('',#2825,#2825,#2260,.T.);
#3850=EDGE_CURVE('',#2826,#2827,#2261,.T.);
#3851=EDGE_CURVE('',#2827,#2674,#107,.T.);
#3852=EDGE_CURVE('',#2673,#2826,#108,.T.);
#3853=EDGE_CURVE('',#2828,#2828,#2262,.T.);
#3854=EDGE_CURVE('',#2828,#2825,#1783,.T.);
#3855=EDGE_CURVE('',#2829,#2829,#2263,.T.);
#3856=EDGE_CURVE('',#2829,#2830,#1784,.T.);
#3857=EDGE_CURVE('',#2830,#2830,#2264,.T.);
#3858=EDGE_CURVE('',#2831,#2831,#2265,.T.);
#3859=EDGE_CURVE('',#2831,#2832,#1785,.T.);
#3860=EDGE_CURVE('',#2832,#2832,#2266,.T.);
#3861=EDGE_CURVE('',#2833,#2833,#2267,.T.);
#3862=EDGE_CURVE('',#2833,#2834,#1786,.T.);
#3863=EDGE_CURVE('',#2834,#2834,#2268,.T.);
#3864=EDGE_CURVE('',#2835,#2835,#2269,.T.);
#3865=EDGE_CURVE('',#2835,#2836,#1787,.T.);
#3866=EDGE_CURVE('',#2836,#2836,#2270,.T.);
#3867=EDGE_CURVE('',#2827,#2756,#560,.T.);
#3868=EDGE_CURVE('',#2757,#2826,#561,.T.);
#3869=EDGE_CURVE('',#2677,#2367,#562,.T.);
#3870=EDGE_CURVE('',#2366,#2678,#563,.T.);
#3871=EDGE_CURVE('',#2837,#2838,#1788,.T.);
#3872=EDGE_CURVE('',#2837,#2839,#1789,.T.);
#3873=EDGE_CURVE('',#2839,#2840,#1790,.T.);
#3874=EDGE_CURVE('',#2838,#2840,#1791,.T.);
#3875=EDGE_CURVE('',#2841,#2837,#1792,.T.);
#3876=EDGE_CURVE('',#2841,#2842,#1793,.T.);
#3877=EDGE_CURVE('',#2842,#2839,#1794,.T.);
#3878=EDGE_CURVE('',#2843,#2841,#1795,.T.);
#3879=EDGE_CURVE('',#2843,#2844,#1796,.T.);
#3880=EDGE_CURVE('',#2844,#2842,#1797,.T.);
#3881=EDGE_CURVE('',#2845,#2843,#1798,.T.);
#3882=EDGE_CURVE('',#2845,#2846,#1799,.T.);
#3883=EDGE_CURVE('',#2846,#2844,#1800,.T.);
#3884=EDGE_CURVE('',#2847,#2845,#1801,.T.);
#3885=EDGE_CURVE('',#2847,#2848,#1802,.T.);
#3886=EDGE_CURVE('',#2848,#2846,#1803,.T.);
#3887=EDGE_CURVE('',#2838,#2847,#1804,.T.);
#3888=EDGE_CURVE('',#2840,#2848,#1805,.T.);
#3889=EDGE_CURVE('',#2849,#2849,#2271,.F.);
#3890=EDGE_CURVE('',#2849,#2850,#1806,.T.);
#3891=EDGE_CURVE('',#2850,#2850,#2272,.F.);
#3892=EDGE_CURVE('',#2851,#2852,#1807,.T.);
#3893=EDGE_CURVE('',#2853,#2851,#1808,.T.);
#3894=EDGE_CURVE('',#2854,#2853,#1809,.T.);
#3895=EDGE_CURVE('',#2852,#2854,#1810,.T.);
#3896=EDGE_CURVE('',#2855,#2856,#1811,.T.);
#3897=EDGE_CURVE('',#2857,#2855,#1812,.T.);
#3898=EDGE_CURVE('',#2858,#2857,#1813,.T.);
#3899=EDGE_CURVE('',#2856,#2858,#1814,.T.);
#3900=EDGE_CURVE('',#2853,#2858,#2273,.T.);
#3901=EDGE_CURVE('',#2856,#2851,#2274,.T.);
#3902=EDGE_CURVE('',#2855,#2852,#2275,.T.);
#3903=EDGE_CURVE('',#2854,#2857,#2276,.T.);
#3904=EDGE_CURVE('',#2859,#2860,#1815,.T.);
#3905=EDGE_CURVE('',#2860,#2861,#564,.T.);
#3906=EDGE_CURVE('',#2862,#2861,#2277,.T.);
#3907=EDGE_CURVE('',#2859,#2862,#565,.T.);
#3908=EDGE_CURVE('',#2863,#2864,#1816,.T.);
#3909=EDGE_CURVE('',#2864,#2865,#566,.T.);
#3910=EDGE_CURVE('',#2865,#2860,#567,.T.);
#3911=EDGE_CURVE('',#2866,#2859,#568,.T.);
#3912=EDGE_CURVE('',#2863,#2866,#569,.T.);
#3913=EDGE_CURVE('',#2867,#2868,#1817,.T.);
#3914=EDGE_CURVE('',#2868,#2869,#570,.T.);
#3915=EDGE_CURVE('',#2869,#2864,#571,.T.);
#3916=EDGE_CURVE('',#2870,#2863,#572,.T.);
#3917=EDGE_CURVE('',#2867,#2870,#573,.T.);
#3918=EDGE_CURVE('',#2871,#2872,#1818,.T.);
#3919=EDGE_CURVE('',#2872,#2873,#574,.T.);
#3920=EDGE_CURVE('',#2873,#2868,#575,.T.);
#3921=EDGE_CURVE('',#2874,#2867,#576,.T.);
#3922=EDGE_CURVE('',#2871,#2874,#577,.T.);
#3923=EDGE_CURVE('',#2875,#2876,#1819,.T.);
#3924=EDGE_CURVE('',#2876,#2877,#578,.T.);
#3925=EDGE_CURVE('',#2877,#2872,#579,.T.);
#3926=EDGE_CURVE('',#2878,#2871,#580,.T.);
#3927=EDGE_CURVE('',#2875,#2878,#581,.T.);
#3928=EDGE_CURVE('',#2879,#2880,#1820,.T.);
#3929=EDGE_CURVE('',#2880,#2881,#582,.T.);
#3930=EDGE_CURVE('',#2881,#2876,#583,.T.);
#3931=EDGE_CURVE('',#2882,#2875,#584,.T.);
#3932=EDGE_CURVE('',#2879,#2882,#585,.T.);
#3933=EDGE_CURVE('',#2883,#2884,#1821,.T.);
#3934=EDGE_CURVE('',#2884,#2885,#586,.T.);
#3935=EDGE_CURVE('',#2885,#2880,#587,.T.);
#3936=EDGE_CURVE('',#2886,#2879,#588,.T.);
#3937=EDGE_CURVE('',#2883,#2886,#589,.T.);
#3938=EDGE_CURVE('',#2887,#2888,#1822,.T.);
#3939=EDGE_CURVE('',#2888,#2889,#590,.T.);
#3940=EDGE_CURVE('',#2889,#2884,#591,.T.);
#3941=EDGE_CURVE('',#2890,#2883,#592,.T.);
#3942=EDGE_CURVE('',#2887,#2890,#593,.T.);
#3943=EDGE_CURVE('',#2891,#2892,#1823,.T.);
#3944=EDGE_CURVE('',#2892,#2893,#594,.T.);
#3945=EDGE_CURVE('',#2893,#2888,#595,.T.);
#3946=EDGE_CURVE('',#2894,#2887,#596,.T.);
#3947=EDGE_CURVE('',#2891,#2894,#597,.T.);
#3948=EDGE_CURVE('',#2895,#2896,#1824,.T.);
#3949=EDGE_CURVE('',#2897,#2895,#598,.T.);
#3950=EDGE_CURVE('',#2898,#2897,#599,.T.);
#3951=EDGE_CURVE('',#2899,#2898,#2278,.T.);
#3952=EDGE_CURVE('',#2899,#2900,#600,.T.);
#3953=EDGE_CURVE('',#2900,#2896,#601,.T.);
#3954=EDGE_CURVE('',#2901,#2902,#1825,.T.);
#3955=EDGE_CURVE('',#2902,#2903,#602,.T.);
#3956=EDGE_CURVE('',#2904,#2903,#2279,.F.);
#3957=EDGE_CURVE('',#2904,#2901,#603,.T.);
#3958=EDGE_CURVE('',#2905,#2906,#1826,.T.);
#3959=EDGE_CURVE('',#2906,#2902,#604,.T.);
#3960=EDGE_CURVE('',#2901,#2905,#605,.T.);
#3961=EDGE_CURVE('',#2907,#2908,#1827,.T.);
#3962=EDGE_CURVE('',#2908,#2909,#606,.T.);
#3963=EDGE_CURVE('',#2909,#2906,#607,.T.);
#3964=EDGE_CURVE('',#2905,#2910,#608,.T.);
#3965=EDGE_CURVE('',#2910,#2907,#609,.T.);
#3966=EDGE_CURVE('',#2911,#2912,#1828,.T.);
#3967=EDGE_CURVE('',#2912,#2913,#610,.T.);
#3968=EDGE_CURVE('',#2913,#2908,#611,.T.);
#3969=EDGE_CURVE('',#2907,#2914,#612,.T.);
#3970=EDGE_CURVE('',#2914,#2911,#613,.T.);
#3971=EDGE_CURVE('',#2915,#2916,#1829,.T.);
#3972=EDGE_CURVE('',#2916,#2917,#614,.T.);
#3973=EDGE_CURVE('',#2917,#2912,#615,.T.);
#3974=EDGE_CURVE('',#2911,#2915,#616,.T.);
#3975=EDGE_CURVE('',#2918,#2919,#1830,.T.);
#3976=EDGE_CURVE('',#2919,#2916,#617,.T.);
#3977=EDGE_CURVE('',#2915,#2920,#618,.T.);
#3978=EDGE_CURVE('',#2920,#2918,#619,.T.);
#3979=EDGE_CURVE('',#2921,#2922,#1831,.T.);
#3980=EDGE_CURVE('',#2922,#2923,#620,.T.);
#3981=EDGE_CURVE('',#2923,#2919,#621,.T.);
#3982=EDGE_CURVE('',#2918,#2924,#622,.T.);
#3983=EDGE_CURVE('',#2924,#2921,#623,.T.);
#3984=EDGE_CURVE('',#2925,#2926,#1832,.T.);
#3985=EDGE_CURVE('',#2926,#2922,#624,.T.);
#3986=EDGE_CURVE('',#2921,#2927,#625,.T.);
#3987=EDGE_CURVE('',#2927,#2925,#626,.T.);
#3988=EDGE_CURVE('',#2928,#2929,#1833,.T.);
#3989=EDGE_CURVE('',#2929,#2930,#627,.T.);
#3990=EDGE_CURVE('',#2930,#2926,#628,.T.);
#3991=EDGE_CURVE('',#2925,#2931,#629,.T.);
#3992=EDGE_CURVE('',#2931,#2928,#630,.T.);
#3993=EDGE_CURVE('',#2932,#2933,#1834,.T.);
#3994=EDGE_CURVE('',#2932,#2934,#631,.F.);
#3995=EDGE_CURVE('',#2935,#2934,#2280,.T.);
#3996=EDGE_CURVE('',#2935,#2936,#632,.T.);
#3997=EDGE_CURVE('',#2936,#2933,#633,.T.);
#3998=EDGE_CURVE('',#2933,#2929,#634,.T.);
#3999=EDGE_CURVE('',#2928,#2937,#635,.T.);
#4000=EDGE_CURVE('',#2937,#2932,#636,.F.);
#4001=EDGE_CURVE('',#2896,#2938,#637,.T.);
#4002=EDGE_CURVE('',#2938,#2892,#638,.T.);
#4003=EDGE_CURVE('',#2939,#2891,#639,.T.);
#4004=EDGE_CURVE('',#2895,#2939,#640,.T.);
#4005=EDGE_CURVE('',#2940,#2940,#2281,.T.);
#4006=EDGE_CURVE('',#2940,#2941,#1835,.T.);
#4007=EDGE_CURVE('',#2941,#2941,#2282,.T.);
#4008=EDGE_CURVE('',#2942,#2942,#2283,.T.);
#4009=EDGE_CURVE('',#2942,#2943,#1836,.T.);
#4010=EDGE_CURVE('',#2943,#2943,#2284,.T.);
#4011=EDGE_CURVE('',#2861,#2944,#641,.T.);
#4012=EDGE_CURVE('',#2934,#2899,#642,.T.);
#4013=EDGE_CURVE('',#2944,#2904,#643,.T.);
#4014=EDGE_CURVE('',#2903,#2862,#644,.T.);
#4015=EDGE_CURVE('',#2898,#2935,#645,.T.);
#4016=EDGE_CURVE('',#2945,#2946,#1837,.T.);
#4017=EDGE_CURVE('',#2946,#2947,#1838,.T.);
#4018=EDGE_CURVE('',#2947,#2948,#1839,.T.);
#4019=EDGE_CURVE('',#2948,#2945,#1840,.F.);
#4020=EDGE_CURVE('',#2949,#2949,#2285,.T.);
#4021=EDGE_CURVE('',#2950,#2950,#2286,.T.);
#4022=EDGE_CURVE('',#2950,#2951,#1841,.T.);
#4023=EDGE_CURVE('',#2951,#2951,#2287,.T.);
#4024=EDGE_CURVE('',#2949,#2952,#1842,.T.);
#4025=EDGE_CURVE('',#2952,#2952,#2288,.T.);
#4026=EDGE_CURVE('',#2953,#2954,#1843,.F.);
#4027=EDGE_CURVE('',#2954,#2945,#1844,.T.);
#4028=EDGE_CURVE('',#2953,#2948,#1845,.F.);
#4029=EDGE_CURVE('',#2955,#2953,#1846,.T.);
#4030=EDGE_CURVE('',#2955,#2947,#1847,.T.);
#4031=EDGE_CURVE('',#2956,#2955,#1848,.T.);
#4032=EDGE_CURVE('',#2956,#2946,#1849,.T.);
#4033=EDGE_CURVE('',#2954,#2956,#1850,.T.);
#4034=EDGE_CURVE('',#2957,#2958,#1851,.T.);
#4035=EDGE_CURVE('',#2958,#2959,#646,.T.);
#4036=EDGE_CURVE('',#2960,#2959,#2289,.T.);
#4037=EDGE_CURVE('',#2957,#2960,#647,.T.);
#4038=EDGE_CURVE('',#2961,#2962,#1852,.T.);
#4039=EDGE_CURVE('',#2962,#2963,#648,.T.);
#4040=EDGE_CURVE('',#2963,#2958,#649,.T.);
#4041=EDGE_CURVE('',#2964,#2957,#650,.T.);
#4042=EDGE_CURVE('',#2961,#2964,#651,.T.);
#4043=EDGE_CURVE('',#2965,#2966,#1853,.T.);
#4044=EDGE_CURVE('',#2966,#2967,#652,.T.);
#4045=EDGE_CURVE('',#2967,#2962,#653,.T.);
#4046=EDGE_CURVE('',#2968,#2961,#654,.T.);
#4047=EDGE_CURVE('',#2965,#2968,#655,.T.);
#4048=EDGE_CURVE('',#2969,#2970,#1854,.T.);
#4049=EDGE_CURVE('',#2970,#2971,#656,.T.);
#4050=EDGE_CURVE('',#2971,#2966,#657,.T.);
#4051=EDGE_CURVE('',#2972,#2965,#658,.T.);
#4052=EDGE_CURVE('',#2969,#2972,#659,.T.);
#4053=EDGE_CURVE('',#2973,#2974,#1855,.T.);
#4054=EDGE_CURVE('',#2974,#2975,#660,.T.);
#4055=EDGE_CURVE('',#2975,#2970,#661,.T.);
#4056=EDGE_CURVE('',#2976,#2969,#662,.T.);
#4057=EDGE_CURVE('',#2973,#2976,#663,.T.);
#4058=EDGE_CURVE('',#2977,#2978,#1856,.T.);
#4059=EDGE_CURVE('',#2979,#2977,#664,.T.);
#4060=EDGE_CURVE('',#2980,#2979,#665,.T.);
#4061=EDGE_CURVE('',#2981,#2980,#2290,.T.);
#4062=EDGE_CURVE('',#2981,#2982,#666,.T.);
#4063=EDGE_CURVE('',#2982,#2978,#667,.T.);
#4064=EDGE_CURVE('',#2983,#2984,#1857,.T.);
#4065=EDGE_CURVE('',#2984,#2985,#668,.T.);
#4066=EDGE_CURVE('',#2986,#2985,#2291,.T.);
#4067=EDGE_CURVE('',#2983,#2986,#669,.T.);
#4068=EDGE_CURVE('',#2987,#2988,#1858,.T.);
#4069=EDGE_CURVE('',#2988,#2989,#670,.T.);
#4070=EDGE_CURVE('',#2989,#2984,#671,.T.);
#4071=EDGE_CURVE('',#2990,#2983,#672,.T.);
#4072=EDGE_CURVE('',#2987,#2990,#673,.T.);
#4073=EDGE_CURVE('',#2991,#2992,#1859,.T.);
#4074=EDGE_CURVE('',#2992,#2993,#674,.T.);
#4075=EDGE_CURVE('',#2993,#2988,#675,.T.);
#4076=EDGE_CURVE('',#2994,#2987,#676,.T.);
#4077=EDGE_CURVE('',#2991,#2994,#677,.T.);
#4078=EDGE_CURVE('',#2995,#2996,#1860,.T.);
#4079=EDGE_CURVE('',#2996,#2997,#678,.T.);
#4080=EDGE_CURVE('',#2997,#2992,#679,.T.);
#4081=EDGE_CURVE('',#2998,#2991,#680,.T.);
#4082=EDGE_CURVE('',#2995,#2998,#681,.T.);
#4083=EDGE_CURVE('',#2999,#3000,#1861,.T.);
#4084=EDGE_CURVE('',#3000,#3001,#682,.T.);
#4085=EDGE_CURVE('',#3001,#2996,#683,.T.);
#4086=EDGE_CURVE('',#3002,#2995,#684,.T.);
#4087=EDGE_CURVE('',#2999,#3002,#685,.T.);
#4088=EDGE_CURVE('',#3003,#3004,#1862,.T.);
#4089=EDGE_CURVE('',#3005,#3003,#686,.T.);
#4090=EDGE_CURVE('',#3006,#3005,#687,.T.);
#4091=EDGE_CURVE('',#3007,#3006,#2292,.T.);
#4092=EDGE_CURVE('',#3007,#3008,#688,.T.);
#4093=EDGE_CURVE('',#3008,#3004,#689,.T.);
#4094=EDGE_CURVE('',#3009,#3010,#1863,.T.);
#4095=EDGE_CURVE('',#3010,#3011,#690,.T.);
#4096=EDGE_CURVE('',#3012,#3011,#2293,.F.);
#4097=EDGE_CURVE('',#3012,#3009,#691,.T.);
#4098=EDGE_CURVE('',#3013,#3014,#1864,.T.);
#4099=EDGE_CURVE('',#3014,#3015,#692,.T.);
#4100=EDGE_CURVE('',#3015,#3010,#693,.T.);
#4101=EDGE_CURVE('',#3009,#3013,#694,.T.);
#4102=EDGE_CURVE('',#3016,#3017,#1865,.T.);
#4103=EDGE_CURVE('',#3017,#3018,#695,.T.);
#4104=EDGE_CURVE('',#3018,#3014,#696,.T.);
#4105=EDGE_CURVE('',#3013,#3019,#697,.T.);
#4106=EDGE_CURVE('',#3019,#3016,#698,.T.);
#4107=EDGE_CURVE('',#3020,#3021,#1866,.T.);
#4108=EDGE_CURVE('',#3021,#3022,#699,.T.);
#4109=EDGE_CURVE('',#3022,#3017,#700,.T.);
#4110=EDGE_CURVE('',#3016,#3020,#701,.T.);
#4111=EDGE_CURVE('',#3023,#3024,#1867,.T.);
#4112=EDGE_CURVE('',#3024,#3025,#702,.T.);
#4113=EDGE_CURVE('',#3025,#3021,#703,.T.);
#4114=EDGE_CURVE('',#3020,#3026,#704,.T.);
#4115=EDGE_CURVE('',#3026,#3023,#705,.T.);
#4116=EDGE_CURVE('',#3027,#3028,#1868,.T.);
#4117=EDGE_CURVE('',#3027,#3029,#706,.T.);
#4118=EDGE_CURVE('',#3029,#3030,#707,.T.);
#4119=EDGE_CURVE('',#3031,#3030,#2294,.T.);
#4120=EDGE_CURVE('',#3031,#3032,#708,.T.);
#4121=EDGE_CURVE('',#3032,#3028,#709,.T.);
#4122=EDGE_CURVE('',#3033,#3034,#1869,.T.);
#4123=EDGE_CURVE('',#3034,#3035,#710,.T.);
#4124=EDGE_CURVE('',#3036,#3035,#2295,.F.);
#4125=EDGE_CURVE('',#3036,#3033,#711,.T.);
#4126=EDGE_CURVE('',#3037,#3038,#1870,.T.);
#4127=EDGE_CURVE('',#3038,#3039,#712,.T.);
#4128=EDGE_CURVE('',#3039,#3034,#713,.T.);
#4129=EDGE_CURVE('',#3033,#3037,#714,.T.);
#4130=EDGE_CURVE('',#3040,#3041,#1871,.T.);
#4131=EDGE_CURVE('',#3041,#3042,#715,.T.);
#4132=EDGE_CURVE('',#3042,#3038,#716,.T.);
#4133=EDGE_CURVE('',#3037,#3043,#717,.T.);
#4134=EDGE_CURVE('',#3043,#3040,#718,.T.);
#4135=EDGE_CURVE('',#3044,#3045,#1872,.T.);
#4136=EDGE_CURVE('',#3045,#3046,#719,.T.);
#4137=EDGE_CURVE('',#3046,#3041,#720,.T.);
#4138=EDGE_CURVE('',#3040,#3044,#721,.T.);
#4139=EDGE_CURVE('',#3047,#3048,#1873,.T.);
#4140=EDGE_CURVE('',#3048,#3049,#722,.T.);
#4141=EDGE_CURVE('',#3049,#3045,#723,.T.);
#4142=EDGE_CURVE('',#3044,#3050,#724,.T.);
#4143=EDGE_CURVE('',#3050,#3047,#725,.T.);
#4144=EDGE_CURVE('',#3051,#3052,#1874,.T.);
#4145=EDGE_CURVE('',#3051,#3053,#726,.T.);
#4146=EDGE_CURVE('',#3053,#3054,#727,.T.);
#4147=EDGE_CURVE('',#3055,#3054,#2296,.T.);
#4148=EDGE_CURVE('',#3055,#3056,#728,.T.);
#4149=EDGE_CURVE('',#3056,#3052,#729,.T.);
#4150=EDGE_CURVE('',#3052,#3057,#730,.T.);
#4151=EDGE_CURVE('',#3057,#3048,#731,.T.);
#4152=EDGE_CURVE('',#3047,#3058,#732,.T.);
#4153=EDGE_CURVE('',#3058,#3051,#733,.T.);
#4154=EDGE_CURVE('',#3028,#3059,#734,.T.);
#4155=EDGE_CURVE('',#3059,#3024,#735,.T.);
#4156=EDGE_CURVE('',#3023,#3060,#736,.T.);
#4157=EDGE_CURVE('',#3060,#3027,#737,.T.);
#4158=EDGE_CURVE('',#3004,#3061,#738,.T.);
#4159=EDGE_CURVE('',#3061,#3000,#739,.T.);
#4160=EDGE_CURVE('',#3062,#2999,#740,.T.);
#4161=EDGE_CURVE('',#3003,#3062,#741,.T.);
#4162=EDGE_CURVE('',#2978,#3063,#742,.T.);
#4163=EDGE_CURVE('',#3063,#2974,#743,.T.);
#4164=EDGE_CURVE('',#3064,#2973,#744,.T.);
#4165=EDGE_CURVE('',#2977,#3064,#745,.T.);
#4166=EDGE_CURVE('',#2959,#3065,#746,.T.);
#4167=EDGE_CURVE('',#3054,#2981,#747,.T.);
#4168=EDGE_CURVE('',#3065,#3036,#748,.T.);
#4169=EDGE_CURVE('',#3035,#2960,#749,.T.);
#4170=EDGE_CURVE('',#2980,#3055,#750,.T.);
#4171=EDGE_CURVE('',#3066,#3067,#1875,.T.);
#4172=EDGE_CURVE('',#3067,#3068,#1876,.T.);
#4173=EDGE_CURVE('',#3068,#3069,#1877,.T.);
#4174=EDGE_CURVE('',#3069,#3066,#1878,.T.);
#4175=EDGE_CURVE('',#3030,#3007,#751,.T.);
#4176=EDGE_CURVE('',#3006,#3031,#752,.T.);
#4177=EDGE_CURVE('',#3070,#3070,#2297,.T.);
#4178=EDGE_CURVE('',#2985,#3071,#753,.T.);
#4179=EDGE_CURVE('',#3071,#3012,#754,.T.);
#4180=EDGE_CURVE('',#3011,#2986,#755,.T.);
#4181=EDGE_CURVE('',#3070,#3072,#1879,.T.);
#4182=EDGE_CURVE('',#3072,#3072,#2298,.T.);
#4183=EDGE_CURVE('',#3073,#3074,#1880,.T.);
#4184=EDGE_CURVE('',#3074,#3066,#1881,.T.);
#4185=EDGE_CURVE('',#3073,#3069,#1882,.T.);
#4186=EDGE_CURVE('',#3075,#3073,#1883,.T.);
#4187=EDGE_CURVE('',#3075,#3068,#1884,.T.);
#4188=EDGE_CURVE('',#3076,#3075,#1885,.T.);
#4189=EDGE_CURVE('',#3076,#3067,#1886,.T.);
#4190=EDGE_CURVE('',#3074,#3076,#1887,.T.);
#4191=EDGE_CURVE('',#3077,#3077,#2299,.T.);
#4192=EDGE_CURVE('',#3077,#3078,#1888,.T.);
#4193=EDGE_CURVE('',#3078,#3078,#2300,.T.);
#4194=EDGE_CURVE('',#3079,#3079,#2301,.T.);
#4195=EDGE_CURVE('',#3080,#3080,#2302,.T.);
#4196=EDGE_CURVE('',#3081,#3081,#2303,.T.);
#4197=EDGE_CURVE('',#3081,#3080,#1889,.T.);
#4198=EDGE_CURVE('',#3082,#3082,#2304,.T.);
#4199=EDGE_CURVE('',#3083,#3083,#2305,.T.);
#4200=EDGE_CURVE('',#3082,#3084,#1890,.T.);
#4201=EDGE_CURVE('',#3084,#3084,#2306,.T.);
#4202=EDGE_CURVE('',#3079,#3083,#1891,.T.);
#4203=EDGE_CURVE('',#3085,#3086,#1892,.T.);
#4204=EDGE_CURVE('',#3087,#3085,#1893,.T.);
#4205=EDGE_CURVE('',#3088,#3087,#1894,.T.);
#4206=EDGE_CURVE('',#3086,#3088,#1895,.T.);
#4207=EDGE_CURVE('',#3089,#3090,#1896,.T.);
#4208=EDGE_CURVE('',#3091,#3089,#1897,.T.);
#4209=EDGE_CURVE('',#3092,#3091,#1898,.T.);
#4210=EDGE_CURVE('',#3090,#3092,#1899,.T.);
#4211=EDGE_CURVE('',#3087,#3092,#2307,.T.);
#4212=EDGE_CURVE('',#3090,#3085,#2308,.T.);
#4213=EDGE_CURVE('',#3089,#3086,#2309,.T.);
#4214=EDGE_CURVE('',#3088,#3091,#2310,.T.);
#4215=EDGE_CURVE('',#3093,#3093,#2311,.T.);
#4216=EDGE_CURVE('',#3093,#3094,#1900,.T.);
#4217=EDGE_CURVE('',#3094,#3094,#2312,.T.);
#4218=EDGE_CURVE('',#3095,#3095,#2313,.T.);
#4219=EDGE_CURVE('',#3095,#3096,#1901,.T.);
#4220=EDGE_CURVE('',#3096,#3096,#2314,.T.);
#4221=EDGE_CURVE('',#3097,#3097,#2315,.T.);
#4222=EDGE_CURVE('',#3097,#3098,#1902,.T.);
#4223=EDGE_CURVE('',#3098,#3098,#2316,.T.);
#4224=EDGE_CURVE('',#3099,#3099,#2317,.T.);
#4225=EDGE_CURVE('',#3099,#3100,#1903,.T.);
#4226=EDGE_CURVE('',#3100,#3100,#2318,.T.);
#4227=EDGE_CURVE('',#3101,#3102,#1904,.T.);
#4228=EDGE_CURVE('',#3103,#3101,#756,.F.);
#4229=EDGE_CURVE('',#3104,#3103,#2319,.T.);
#4230=EDGE_CURVE('',#3104,#3102,#757,.T.);
#4231=EDGE_CURVE('',#3105,#3106,#1905,.T.);
#4232=EDGE_CURVE('',#3101,#3105,#758,.F.);
#4233=EDGE_CURVE('',#3102,#3107,#759,.T.);
#4234=EDGE_CURVE('',#3107,#3106,#760,.T.);
#4235=EDGE_CURVE('',#3108,#3109,#1906,.T.);
#4236=EDGE_CURVE('',#3110,#3108,#761,.F.);
#4237=EDGE_CURVE('',#3105,#3110,#762,.F.);
#4238=EDGE_CURVE('',#3106,#3109,#763,.T.);
#4239=EDGE_CURVE('',#3111,#3112,#1907,.T.);
#4240=EDGE_CURVE('',#3108,#3111,#764,.F.);
#4241=EDGE_CURVE('',#3109,#3113,#765,.T.);
#4242=EDGE_CURVE('',#3113,#3112,#766,.T.);
#4243=EDGE_CURVE('',#3114,#3115,#1908,.T.);
#4244=EDGE_CURVE('',#3116,#3114,#767,.T.);
#4245=EDGE_CURVE('',#3111,#3116,#768,.F.);
#4246=EDGE_CURVE('',#3112,#3117,#769,.T.);
#4247=EDGE_CURVE('',#3117,#3115,#770,.T.);
#4248=EDGE_CURVE('',#3118,#3119,#1909,.T.);
#4249=EDGE_CURVE('',#3120,#3118,#771,.T.);
#4250=EDGE_CURVE('',#3114,#3120,#772,.T.);
#4251=EDGE_CURVE('',#3115,#3119,#773,.T.);
#4252=EDGE_CURVE('',#3121,#3122,#1910,.T.);
#4253=EDGE_CURVE('',#3123,#3121,#774,.F.);
#4254=EDGE_CURVE('',#3118,#3123,#775,.T.);
#4255=EDGE_CURVE('',#3119,#3124,#776,.T.);
#4256=EDGE_CURVE('',#3124,#3122,#777,.T.);
#4257=EDGE_CURVE('',#3125,#3126,#1911,.T.);
#4258=EDGE_CURVE('',#3121,#3125,#778,.F.);
#4259=EDGE_CURVE('',#3122,#3126,#779,.T.);
#4260=EDGE_CURVE('',#3127,#3128,#1912,.T.);
#4261=EDGE_CURVE('',#3129,#3127,#780,.F.);
#4262=EDGE_CURVE('',#3125,#3129,#781,.F.);
#4263=EDGE_CURVE('',#3126,#3130,#782,.T.);
#4264=EDGE_CURVE('',#3130,#3128,#783,.T.);
#4265=EDGE_CURVE('',#3131,#3132,#1913,.T.);
#4266=EDGE_CURVE('',#3127,#3131,#784,.F.);
#4267=EDGE_CURVE('',#3128,#3132,#785,.T.);
#4268=EDGE_CURVE('',#3133,#3134,#1914,.T.);
#4269=EDGE_CURVE('',#3135,#3133,#786,.T.);
#4270=EDGE_CURVE('',#3131,#3135,#787,.F.);
#4271=EDGE_CURVE('',#3132,#3136,#788,.T.);
#4272=EDGE_CURVE('',#3136,#3134,#789,.T.);
#4273=EDGE_CURVE('',#3137,#3138,#1915,.T.);
#4274=EDGE_CURVE('',#3139,#3137,#790,.T.);
#4275=EDGE_CURVE('',#3133,#3139,#791,.T.);
#4276=EDGE_CURVE('',#3134,#3140,#792,.T.);
#4277=EDGE_CURVE('',#3140,#3138,#793,.T.);
#4278=EDGE_CURVE('',#3141,#3142,#1916,.T.);
#4279=EDGE_CURVE('',#3143,#3141,#794,.F.);
#4280=EDGE_CURVE('',#3137,#3143,#795,.T.);
#4281=EDGE_CURVE('',#3138,#3142,#796,.T.);
#4282=EDGE_CURVE('',#3144,#3145,#1917,.T.);
#4283=EDGE_CURVE('',#3141,#3144,#797,.F.);
#4284=EDGE_CURVE('',#3142,#3146,#798,.T.);
#4285=EDGE_CURVE('',#3146,#3145,#799,.T.);
#4286=EDGE_CURVE('',#3147,#3148,#1918,.T.);
#4287=EDGE_CURVE('',#3149,#3147,#800,.F.);
#4288=EDGE_CURVE('',#3144,#3149,#801,.F.);
#4289=EDGE_CURVE('',#3145,#3148,#802,.T.);
#4290=EDGE_CURVE('',#3150,#3151,#1919,.T.);
#4291=EDGE_CURVE('',#3147,#3150,#803,.F.);
#4292=EDGE_CURVE('',#3148,#3152,#804,.T.);
#4293=EDGE_CURVE('',#3152,#3151,#805,.T.);
#4294=EDGE_CURVE('',#3153,#3154,#1920,.T.);
#4295=EDGE_CURVE('',#3155,#3153,#806,.F.);
#4296=EDGE_CURVE('',#3150,#3155,#807,.F.);
#4297=EDGE_CURVE('',#3151,#3154,#808,.T.);
#4298=EDGE_CURVE('',#3156,#3157,#1921,.T.);
#4299=EDGE_CURVE('',#3153,#3156,#809,.F.);
#4300=EDGE_CURVE('',#3154,#3158,#810,.T.);
#4301=EDGE_CURVE('',#3158,#3157,#811,.T.);
#4302=EDGE_CURVE('',#3159,#3160,#1922,.T.);
#4303=EDGE_CURVE('',#3161,#3159,#812,.F.);
#4304=EDGE_CURVE('',#3156,#3161,#813,.F.);
#4305=EDGE_CURVE('',#3157,#3162,#814,.T.);
#4306=EDGE_CURVE('',#3162,#3160,#815,.T.);
#4307=EDGE_CURVE('',#3163,#3164,#1923,.T.);
#4308=EDGE_CURVE('',#3159,#3163,#816,.F.);
#4309=EDGE_CURVE('',#3160,#3164,#817,.T.);
#4310=EDGE_CURVE('',#3165,#3166,#1924,.T.);
#4311=EDGE_CURVE('',#3167,#3165,#818,.F.);
#4312=EDGE_CURVE('',#3163,#3167,#819,.F.);
#4313=EDGE_CURVE('',#3164,#3168,#820,.T.);
#4314=EDGE_CURVE('',#3168,#3166,#821,.T.);
#4315=EDGE_CURVE('',#3169,#3170,#1925,.T.);
#4316=EDGE_CURVE('',#3165,#3169,#822,.F.);
#4317=EDGE_CURVE('',#3166,#3170,#823,.T.);
#4318=EDGE_CURVE('',#3171,#3172,#1926,.T.);
#4319=EDGE_CURVE('',#3173,#3171,#824,.F.);
#4320=EDGE_CURVE('',#3169,#3173,#825,.F.);
#4321=EDGE_CURVE('',#3170,#3174,#826,.T.);
#4322=EDGE_CURVE('',#3174,#3172,#827,.T.);
#4323=EDGE_CURVE('',#3175,#3176,#1927,.T.);
#4324=EDGE_CURVE('',#3171,#3175,#828,.F.);
#4325=EDGE_CURVE('',#3172,#3176,#829,.T.);
#4326=EDGE_CURVE('',#3177,#3178,#830,.T.);
#4327=EDGE_CURVE('',#3178,#3179,#2320,.F.);
#4328=EDGE_CURVE('',#3179,#3180,#831,.T.);
#4329=EDGE_CURVE('',#3180,#3181,#832,.T.);
#4330=EDGE_CURVE('',#3181,#3182,#833,.T.);
#4331=EDGE_CURVE('',#3182,#3183,#834,.T.);
#4332=EDGE_CURVE('',#3183,#3184,#835,.T.);
#4333=EDGE_CURVE('',#3184,#3185,#836,.T.);
#4334=EDGE_CURVE('',#3185,#3186,#837,.T.);
#4335=EDGE_CURVE('',#3186,#3187,#838,.T.);
#4336=EDGE_CURVE('',#3187,#3188,#839,.T.);
#4337=EDGE_CURVE('',#3188,#3189,#840,.T.);
#4338=EDGE_CURVE('',#3189,#3190,#841,.T.);
#4339=EDGE_CURVE('',#3190,#3191,#842,.T.);
#4340=EDGE_CURVE('',#3191,#3192,#843,.T.);
#4341=EDGE_CURVE('',#3192,#3193,#844,.T.);
#4342=EDGE_CURVE('',#3193,#3194,#845,.T.);
#4343=EDGE_CURVE('',#3194,#3195,#846,.T.);
#4344=EDGE_CURVE('',#3195,#3196,#847,.T.);
#4345=EDGE_CURVE('',#3196,#3197,#848,.T.);
#4346=EDGE_CURVE('',#3197,#3198,#849,.T.);
#4347=EDGE_CURVE('',#3198,#3199,#850,.T.);
#4348=EDGE_CURVE('',#3199,#3200,#851,.T.);
#4349=EDGE_CURVE('',#3200,#3201,#852,.T.);
#4350=EDGE_CURVE('',#3201,#3202,#853,.T.);
#4351=EDGE_CURVE('',#3202,#3203,#854,.T.);
#4352=EDGE_CURVE('',#3203,#3204,#855,.T.);
#4353=EDGE_CURVE('',#3204,#3205,#2321,.T.);
#4354=EDGE_CURVE('',#3205,#3206,#856,.T.);
#4355=EDGE_CURVE('',#3206,#3207,#857,.T.);
#4356=EDGE_CURVE('',#3207,#3208,#858,.T.);
#4357=EDGE_CURVE('',#3208,#3209,#859,.T.);
#4358=EDGE_CURVE('',#3209,#3210,#860,.T.);
#4359=EDGE_CURVE('',#3210,#3211,#861,.T.);
#4360=EDGE_CURVE('',#3211,#3212,#862,.T.);
#4361=EDGE_CURVE('',#3212,#3213,#863,.T.);
#4362=EDGE_CURVE('',#3213,#3214,#864,.T.);
#4363=EDGE_CURVE('',#3214,#3215,#865,.T.);
#4364=EDGE_CURVE('',#3215,#3216,#866,.T.);
#4365=EDGE_CURVE('',#3216,#3217,#867,.T.);
#4366=EDGE_CURVE('',#3217,#3218,#868,.T.);
#4367=EDGE_CURVE('',#3218,#3219,#869,.T.);
#4368=EDGE_CURVE('',#3219,#3220,#870,.T.);
#4369=EDGE_CURVE('',#3220,#3221,#871,.T.);
#4370=EDGE_CURVE('',#3221,#3222,#872,.T.);
#4371=EDGE_CURVE('',#3222,#3223,#873,.T.);
#4372=EDGE_CURVE('',#3223,#3224,#874,.T.);
#4373=EDGE_CURVE('',#3224,#3225,#875,.T.);
#4374=EDGE_CURVE('',#3225,#3226,#876,.T.);
#4375=EDGE_CURVE('',#3226,#3227,#877,.T.);
#4376=EDGE_CURVE('',#3227,#3228,#878,.T.);
#4377=EDGE_CURVE('',#3228,#3177,#879,.T.);
#4378=EDGE_CURVE('',#3176,#3229,#880,.T.);
#4379=EDGE_CURVE('',#3229,#3230,#881,.T.);
#4380=EDGE_CURVE('',#3230,#3231,#2322,.T.);
#4381=EDGE_CURVE('',#3232,#3231,#882,.T.);
#4382=EDGE_CURVE('',#3175,#3232,#883,.F.);
#4383=EDGE_CURVE('',#3231,#3233,#884,.T.);
#4384=EDGE_CURVE('',#3205,#3230,#885,.T.);
#4385=EDGE_CURVE('',#3234,#3204,#886,.T.);
#4386=EDGE_CURVE('',#3233,#3234,#887,.T.);
#4387=EDGE_CURVE('',#3233,#3235,#1928,.T.);
#4388=EDGE_CURVE('',#3235,#3235,#2323,.T.);
#4389=EDGE_CURVE('',#3178,#3104,#888,.T.);
#4390=EDGE_CURVE('',#3236,#3179,#889,.T.);
#4391=EDGE_CURVE('',#3236,#3103,#890,.T.);
#4392=EDGE_CURVE('',#3237,#3238,#1929,.T.);
#4393=EDGE_CURVE('',#3237,#3239,#1930,.T.);
#4394=EDGE_CURVE('',#3239,#3240,#1931,.T.);
#4395=EDGE_CURVE('',#3238,#3240,#1932,.T.);
#4396=EDGE_CURVE('',#3241,#3237,#1933,.T.);
#4397=EDGE_CURVE('',#3241,#3242,#1934,.T.);
#4398=EDGE_CURVE('',#3242,#3239,#1935,.T.);
#4399=EDGE_CURVE('',#3243,#3241,#1936,.T.);
#4400=EDGE_CURVE('',#3243,#3244,#1937,.T.);
#4401=EDGE_CURVE('',#3244,#3242,#1938,.T.);
#4402=EDGE_CURVE('',#3245,#3243,#1939,.T.);
#4403=EDGE_CURVE('',#3245,#3246,#1940,.T.);
#4404=EDGE_CURVE('',#3246,#3244,#1941,.T.);
#4405=EDGE_CURVE('',#3247,#3245,#1942,.T.);
#4406=EDGE_CURVE('',#3247,#3248,#1943,.T.);
#4407=EDGE_CURVE('',#3248,#3246,#1944,.T.);
#4408=EDGE_CURVE('',#3238,#3247,#1945,.T.);
#4409=EDGE_CURVE('',#3240,#3248,#1946,.T.);
#4410=EDGE_CURVE('',#3249,#3249,#2324,.T.);
#4411=EDGE_CURVE('',#3249,#3250,#1947,.T.);
#4412=EDGE_CURVE('',#3250,#3250,#2325,.T.);
#4413=ORIENTED_EDGE('',*,*,#3251,.F.);
#4414=ORIENTED_EDGE('',*,*,#3252,.T.);
#4415=ORIENTED_EDGE('',*,*,#3253,.F.);
#4416=ORIENTED_EDGE('',*,*,#3252,.F.);
#4417=ORIENTED_EDGE('',*,*,#3254,.F.);
#4418=ORIENTED_EDGE('',*,*,#3255,.T.);
#4419=ORIENTED_EDGE('',*,*,#3256,.F.);
#4420=ORIENTED_EDGE('',*,*,#3255,.F.);
#4421=ORIENTED_EDGE('',*,*,#3257,.F.);
#4422=ORIENTED_EDGE('',*,*,#3258,.T.);
#4423=ORIENTED_EDGE('',*,*,#3259,.F.);
#4424=ORIENTED_EDGE('',*,*,#3258,.F.);
#4425=ORIENTED_EDGE('',*,*,#3260,.F.);
#4426=ORIENTED_EDGE('',*,*,#3261,.T.);
#4427=ORIENTED_EDGE('',*,*,#3262,.F.);
#4428=ORIENTED_EDGE('',*,*,#3261,.F.);
#4429=ORIENTED_EDGE('',*,*,#3263,.T.);
#4430=ORIENTED_EDGE('',*,*,#3264,.T.);
#4431=ORIENTED_EDGE('',*,*,#3265,.F.);
#4432=ORIENTED_EDGE('',*,*,#3266,.F.);
#4433=ORIENTED_EDGE('',*,*,#3267,.T.);
#4434=ORIENTED_EDGE('',*,*,#3266,.T.);
#4435=ORIENTED_EDGE('',*,*,#3268,.F.);
#4436=ORIENTED_EDGE('',*,*,#3269,.F.);
#4437=ORIENTED_EDGE('',*,*,#3270,.T.);
#4438=ORIENTED_EDGE('',*,*,#3269,.T.);
#4439=ORIENTED_EDGE('',*,*,#3271,.F.);
#4440=ORIENTED_EDGE('',*,*,#3272,.F.);
#4441=ORIENTED_EDGE('',*,*,#3273,.T.);
#4442=ORIENTED_EDGE('',*,*,#3272,.T.);
#4443=ORIENTED_EDGE('',*,*,#3274,.F.);
#4444=ORIENTED_EDGE('',*,*,#3264,.F.);
#4445=ORIENTED_EDGE('',*,*,#3274,.T.);
#4446=ORIENTED_EDGE('',*,*,#3271,.T.);
#4447=ORIENTED_EDGE('',*,*,#3268,.T.);
#4448=ORIENTED_EDGE('',*,*,#3265,.T.);
#4449=ORIENTED_EDGE('',*,*,#3251,.T.);
#4450=ORIENTED_EDGE('',*,*,#3254,.T.);
#4451=ORIENTED_EDGE('',*,*,#3257,.T.);
#4452=ORIENTED_EDGE('',*,*,#3260,.T.);
#4453=ORIENTED_EDGE('',*,*,#3273,.F.);
#4454=ORIENTED_EDGE('',*,*,#3263,.F.);
#4455=ORIENTED_EDGE('',*,*,#3267,.F.);
#4456=ORIENTED_EDGE('',*,*,#3270,.F.);
#4457=ORIENTED_EDGE('',*,*,#3253,.T.);
#4458=ORIENTED_EDGE('',*,*,#3256,.T.);
#4459=ORIENTED_EDGE('',*,*,#3259,.T.);
#4460=ORIENTED_EDGE('',*,*,#3262,.T.);
#4461=ORIENTED_EDGE('',*,*,#3275,.F.);
#4462=ORIENTED_EDGE('',*,*,#3276,.T.);
#4463=ORIENTED_EDGE('',*,*,#3277,.F.);
#4464=ORIENTED_EDGE('',*,*,#3276,.F.);
#4465=ORIENTED_EDGE('',*,*,#3278,.F.);
#4466=ORIENTED_EDGE('',*,*,#3279,.T.);
#4467=ORIENTED_EDGE('',*,*,#3280,.F.);
#4468=ORIENTED_EDGE('',*,*,#3279,.F.);
#4469=ORIENTED_EDGE('',*,*,#3281,.F.);
#4470=ORIENTED_EDGE('',*,*,#3282,.T.);
#4471=ORIENTED_EDGE('',*,*,#3283,.F.);
#4472=ORIENTED_EDGE('',*,*,#3282,.F.);
#4473=ORIENTED_EDGE('',*,*,#3284,.F.);
#4474=ORIENTED_EDGE('',*,*,#3285,.T.);
#4475=ORIENTED_EDGE('',*,*,#3286,.F.);
#4476=ORIENTED_EDGE('',*,*,#3285,.F.);
#4477=ORIENTED_EDGE('',*,*,#3287,.F.);
#4478=ORIENTED_EDGE('',*,*,#3288,.T.);
#4479=ORIENTED_EDGE('',*,*,#3289,.F.);
#4480=ORIENTED_EDGE('',*,*,#3288,.F.);
#4481=ORIENTED_EDGE('',*,*,#3290,.T.);
#4482=ORIENTED_EDGE('',*,*,#3291,.T.);
#4483=ORIENTED_EDGE('',*,*,#3292,.F.);
#4484=ORIENTED_EDGE('',*,*,#3293,.F.);
#4485=ORIENTED_EDGE('',*,*,#3294,.T.);
#4486=ORIENTED_EDGE('',*,*,#3293,.T.);
#4487=ORIENTED_EDGE('',*,*,#3295,.F.);
#4488=ORIENTED_EDGE('',*,*,#3296,.F.);
#4489=ORIENTED_EDGE('',*,*,#3297,.T.);
#4490=ORIENTED_EDGE('',*,*,#3296,.T.);
#4491=ORIENTED_EDGE('',*,*,#3298,.F.);
#4492=ORIENTED_EDGE('',*,*,#3299,.F.);
#4493=ORIENTED_EDGE('',*,*,#3300,.T.);
#4494=ORIENTED_EDGE('',*,*,#3299,.T.);
#4495=ORIENTED_EDGE('',*,*,#3301,.F.);
#4496=ORIENTED_EDGE('',*,*,#3291,.F.);
#4497=ORIENTED_EDGE('',*,*,#3301,.T.);
#4498=ORIENTED_EDGE('',*,*,#3298,.T.);
#4499=ORIENTED_EDGE('',*,*,#3295,.T.);
#4500=ORIENTED_EDGE('',*,*,#3292,.T.);
#4501=ORIENTED_EDGE('',*,*,#3275,.T.);
#4502=ORIENTED_EDGE('',*,*,#3278,.T.);
#4503=ORIENTED_EDGE('',*,*,#3281,.T.);
#4504=ORIENTED_EDGE('',*,*,#3284,.T.);
#4505=ORIENTED_EDGE('',*,*,#3287,.T.);
#4506=ORIENTED_EDGE('',*,*,#3300,.F.);
#4507=ORIENTED_EDGE('',*,*,#3290,.F.);
#4508=ORIENTED_EDGE('',*,*,#3294,.F.);
#4509=ORIENTED_EDGE('',*,*,#3297,.F.);
#4510=ORIENTED_EDGE('',*,*,#3277,.T.);
#4511=ORIENTED_EDGE('',*,*,#3280,.T.);
#4512=ORIENTED_EDGE('',*,*,#3283,.T.);
#4513=ORIENTED_EDGE('',*,*,#3286,.T.);
#4514=ORIENTED_EDGE('',*,*,#3289,.T.);
#4515=ORIENTED_EDGE('',*,*,#3302,.T.);
#4516=ORIENTED_EDGE('',*,*,#3303,.T.);
#4517=ORIENTED_EDGE('',*,*,#3304,.F.);
#4518=ORIENTED_EDGE('',*,*,#3303,.F.);
#4519=ORIENTED_EDGE('',*,*,#3305,.F.);
#4520=ORIENTED_EDGE('',*,*,#3306,.T.);
#4521=ORIENTED_EDGE('',*,*,#3307,.T.);
#4522=ORIENTED_EDGE('',*,*,#3306,.F.);
#4523=ORIENTED_EDGE('',*,*,#3305,.T.);
#4524=ORIENTED_EDGE('',*,*,#3304,.T.);
#4525=ORIENTED_EDGE('',*,*,#3307,.F.);
#4526=ORIENTED_EDGE('',*,*,#3302,.F.);
#4527=ORIENTED_EDGE('',*,*,#3308,.F.);
#4528=ORIENTED_EDGE('',*,*,#3309,.F.);
#4529=ORIENTED_EDGE('',*,*,#3310,.F.);
#4530=ORIENTED_EDGE('',*,*,#3311,.T.);
#4531=ORIENTED_EDGE('',*,*,#3312,.F.);
#4532=ORIENTED_EDGE('',*,*,#3313,.F.);
#4533=ORIENTED_EDGE('',*,*,#3314,.F.);
#4534=ORIENTED_EDGE('',*,*,#3308,.T.);
#4535=ORIENTED_EDGE('',*,*,#3315,.T.);
#4536=ORIENTED_EDGE('',*,*,#3316,.T.);
#4537=ORIENTED_EDGE('',*,*,#3317,.F.);
#4538=ORIENTED_EDGE('',*,*,#3318,.F.);
#4539=ORIENTED_EDGE('',*,*,#3319,.F.);
#4540=ORIENTED_EDGE('',*,*,#3312,.T.);
#4541=ORIENTED_EDGE('',*,*,#3320,.T.);
#4542=ORIENTED_EDGE('',*,*,#3321,.T.);
#4543=ORIENTED_EDGE('',*,*,#3322,.F.);
#4544=ORIENTED_EDGE('',*,*,#3323,.F.);
#4545=ORIENTED_EDGE('',*,*,#3324,.F.);
#4546=ORIENTED_EDGE('',*,*,#3317,.T.);
#4547=ORIENTED_EDGE('',*,*,#3325,.T.);
#4548=ORIENTED_EDGE('',*,*,#3326,.T.);
#4549=ORIENTED_EDGE('',*,*,#3327,.F.);
#4550=ORIENTED_EDGE('',*,*,#3328,.F.);
#4551=ORIENTED_EDGE('',*,*,#3329,.F.);
#4552=ORIENTED_EDGE('',*,*,#3322,.T.);
#4553=ORIENTED_EDGE('',*,*,#3330,.T.);
#4554=ORIENTED_EDGE('',*,*,#3331,.T.);
#4555=ORIENTED_EDGE('',*,*,#3332,.F.);
#4556=ORIENTED_EDGE('',*,*,#3333,.F.);
#4557=ORIENTED_EDGE('',*,*,#3334,.F.);
#4558=ORIENTED_EDGE('',*,*,#3327,.T.);
#4559=ORIENTED_EDGE('',*,*,#3335,.T.);
#4560=ORIENTED_EDGE('',*,*,#3336,.T.);
#4561=ORIENTED_EDGE('',*,*,#3337,.F.);
#4562=ORIENTED_EDGE('',*,*,#3338,.F.);
#4563=ORIENTED_EDGE('',*,*,#3339,.F.);
#4564=ORIENTED_EDGE('',*,*,#3332,.T.);
#4565=ORIENTED_EDGE('',*,*,#3340,.T.);
#4566=ORIENTED_EDGE('',*,*,#3341,.T.);
#4567=ORIENTED_EDGE('',*,*,#3342,.F.);
#4568=ORIENTED_EDGE('',*,*,#3343,.F.);
#4569=ORIENTED_EDGE('',*,*,#3344,.F.);
#4570=ORIENTED_EDGE('',*,*,#3337,.T.);
#4571=ORIENTED_EDGE('',*,*,#3345,.T.);
#4572=ORIENTED_EDGE('',*,*,#3346,.T.);
#4573=ORIENTED_EDGE('',*,*,#3347,.F.);
#4574=ORIENTED_EDGE('',*,*,#3348,.F.);
#4575=ORIENTED_EDGE('',*,*,#3349,.F.);
#4576=ORIENTED_EDGE('',*,*,#3342,.T.);
#4577=ORIENTED_EDGE('',*,*,#3350,.T.);
#4578=ORIENTED_EDGE('',*,*,#3351,.T.);
#4579=ORIENTED_EDGE('',*,*,#3352,.F.);
#4580=ORIENTED_EDGE('',*,*,#3353,.F.);
#4581=ORIENTED_EDGE('',*,*,#3354,.F.);
#4582=ORIENTED_EDGE('',*,*,#3347,.T.);
#4583=ORIENTED_EDGE('',*,*,#3355,.T.);
#4584=ORIENTED_EDGE('',*,*,#3356,.T.);
#4585=ORIENTED_EDGE('',*,*,#3357,.F.);
#4586=ORIENTED_EDGE('',*,*,#3358,.F.);
#4587=ORIENTED_EDGE('',*,*,#3359,.F.);
#4588=ORIENTED_EDGE('',*,*,#3352,.T.);
#4589=ORIENTED_EDGE('',*,*,#3360,.T.);
#4590=ORIENTED_EDGE('',*,*,#3361,.T.);
#4591=ORIENTED_EDGE('',*,*,#3362,.F.);
#4592=ORIENTED_EDGE('',*,*,#3363,.F.);
#4593=ORIENTED_EDGE('',*,*,#3364,.F.);
#4594=ORIENTED_EDGE('',*,*,#3357,.T.);
#4595=ORIENTED_EDGE('',*,*,#3365,.T.);
#4596=ORIENTED_EDGE('',*,*,#3366,.T.);
#4597=ORIENTED_EDGE('',*,*,#3367,.F.);
#4598=ORIENTED_EDGE('',*,*,#3368,.F.);
#4599=ORIENTED_EDGE('',*,*,#3369,.F.);
#4600=ORIENTED_EDGE('',*,*,#3362,.T.);
#4601=ORIENTED_EDGE('',*,*,#3370,.T.);
#4602=ORIENTED_EDGE('',*,*,#3371,.T.);
#4603=ORIENTED_EDGE('',*,*,#3372,.F.);
#4604=ORIENTED_EDGE('',*,*,#3373,.F.);
#4605=ORIENTED_EDGE('',*,*,#3374,.F.);
#4606=ORIENTED_EDGE('',*,*,#3367,.T.);
#4607=ORIENTED_EDGE('',*,*,#3375,.T.);
#4608=ORIENTED_EDGE('',*,*,#3376,.T.);
#4609=ORIENTED_EDGE('',*,*,#3377,.F.);
#4610=ORIENTED_EDGE('',*,*,#3378,.F.);
#4611=ORIENTED_EDGE('',*,*,#3379,.F.);
#4612=ORIENTED_EDGE('',*,*,#3372,.T.);
#4613=ORIENTED_EDGE('',*,*,#3380,.T.);
#4614=ORIENTED_EDGE('',*,*,#3381,.T.);
#4615=ORIENTED_EDGE('',*,*,#3382,.F.);
#4616=ORIENTED_EDGE('',*,*,#3383,.F.);
#4617=ORIENTED_EDGE('',*,*,#3384,.F.);
#4618=ORIENTED_EDGE('',*,*,#3377,.T.);
#4619=ORIENTED_EDGE('',*,*,#3385,.T.);
#4620=ORIENTED_EDGE('',*,*,#3386,.T.);
#4621=ORIENTED_EDGE('',*,*,#3387,.F.);
#4622=ORIENTED_EDGE('',*,*,#3388,.F.);
#4623=ORIENTED_EDGE('',*,*,#3389,.F.);
#4624=ORIENTED_EDGE('',*,*,#3382,.T.);
#4625=ORIENTED_EDGE('',*,*,#3390,.T.);
#4626=ORIENTED_EDGE('',*,*,#3391,.T.);
#4627=ORIENTED_EDGE('',*,*,#3392,.F.);
#4628=ORIENTED_EDGE('',*,*,#3393,.F.);
#4629=ORIENTED_EDGE('',*,*,#3394,.F.);
#4630=ORIENTED_EDGE('',*,*,#3387,.T.);
#4631=ORIENTED_EDGE('',*,*,#3395,.T.);
#4632=ORIENTED_EDGE('',*,*,#3396,.T.);
#4633=ORIENTED_EDGE('',*,*,#3397,.F.);
#4634=ORIENTED_EDGE('',*,*,#3398,.F.);
#4635=ORIENTED_EDGE('',*,*,#3399,.F.);
#4636=ORIENTED_EDGE('',*,*,#3392,.T.);
#4637=ORIENTED_EDGE('',*,*,#3400,.T.);
#4638=ORIENTED_EDGE('',*,*,#3401,.T.);
#4639=ORIENTED_EDGE('',*,*,#3402,.F.);
#4640=ORIENTED_EDGE('',*,*,#3403,.F.);
#4641=ORIENTED_EDGE('',*,*,#3404,.F.);
#4642=ORIENTED_EDGE('',*,*,#3397,.T.);
#4643=ORIENTED_EDGE('',*,*,#3405,.T.);
#4644=ORIENTED_EDGE('',*,*,#3406,.T.);
#4645=ORIENTED_EDGE('',*,*,#3407,.F.);
#4646=ORIENTED_EDGE('',*,*,#3408,.F.);
#4647=ORIENTED_EDGE('',*,*,#3409,.F.);
#4648=ORIENTED_EDGE('',*,*,#3402,.T.);
#4649=ORIENTED_EDGE('',*,*,#3410,.T.);
#4650=ORIENTED_EDGE('',*,*,#3411,.T.);
#4651=ORIENTED_EDGE('',*,*,#3412,.F.);
#4652=ORIENTED_EDGE('',*,*,#3413,.F.);
#4653=ORIENTED_EDGE('',*,*,#3414,.F.);
#4654=ORIENTED_EDGE('',*,*,#3407,.T.);
#4655=ORIENTED_EDGE('',*,*,#3415,.T.);
#4656=ORIENTED_EDGE('',*,*,#3416,.T.);
#4657=ORIENTED_EDGE('',*,*,#3417,.F.);
#4658=ORIENTED_EDGE('',*,*,#3418,.F.);
#4659=ORIENTED_EDGE('',*,*,#3419,.F.);
#4660=ORIENTED_EDGE('',*,*,#3412,.T.);
#4661=ORIENTED_EDGE('',*,*,#3420,.T.);
#4662=ORIENTED_EDGE('',*,*,#3421,.T.);
#4663=ORIENTED_EDGE('',*,*,#3422,.F.);
#4664=ORIENTED_EDGE('',*,*,#3423,.F.);
#4665=ORIENTED_EDGE('',*,*,#3424,.F.);
#4666=ORIENTED_EDGE('',*,*,#3417,.T.);
#4667=ORIENTED_EDGE('',*,*,#3425,.T.);
#4668=ORIENTED_EDGE('',*,*,#3426,.T.);
#4669=ORIENTED_EDGE('',*,*,#3427,.F.);
#4670=ORIENTED_EDGE('',*,*,#3428,.F.);
#4671=ORIENTED_EDGE('',*,*,#3429,.F.);
#4672=ORIENTED_EDGE('',*,*,#3422,.T.);
#4673=ORIENTED_EDGE('',*,*,#3430,.T.);
#4674=ORIENTED_EDGE('',*,*,#3431,.T.);
#4675=ORIENTED_EDGE('',*,*,#3432,.F.);
#4676=ORIENTED_EDGE('',*,*,#3433,.F.);
#4677=ORIENTED_EDGE('',*,*,#3434,.F.);
#4678=ORIENTED_EDGE('',*,*,#3427,.T.);
#4679=ORIENTED_EDGE('',*,*,#3435,.T.);
#4680=ORIENTED_EDGE('',*,*,#3436,.T.);
#4681=ORIENTED_EDGE('',*,*,#3437,.F.);
#4682=ORIENTED_EDGE('',*,*,#3438,.F.);
#4683=ORIENTED_EDGE('',*,*,#3439,.F.);
#4684=ORIENTED_EDGE('',*,*,#3432,.T.);
#4685=ORIENTED_EDGE('',*,*,#3440,.T.);
#4686=ORIENTED_EDGE('',*,*,#3441,.T.);
#4687=ORIENTED_EDGE('',*,*,#3442,.F.);
#4688=ORIENTED_EDGE('',*,*,#3443,.F.);
#4689=ORIENTED_EDGE('',*,*,#3444,.F.);
#4690=ORIENTED_EDGE('',*,*,#3437,.T.);
#4691=ORIENTED_EDGE('',*,*,#3445,.T.);
#4692=ORIENTED_EDGE('',*,*,#3446,.T.);
#4693=ORIENTED_EDGE('',*,*,#3447,.F.);
#4694=ORIENTED_EDGE('',*,*,#3448,.F.);
#4695=ORIENTED_EDGE('',*,*,#3449,.F.);
#4696=ORIENTED_EDGE('',*,*,#3442,.T.);
#4697=ORIENTED_EDGE('',*,*,#3450,.T.);
#4698=ORIENTED_EDGE('',*,*,#3451,.T.);
#4699=ORIENTED_EDGE('',*,*,#3452,.F.);
#4700=ORIENTED_EDGE('',*,*,#3453,.F.);
#4701=ORIENTED_EDGE('',*,*,#3454,.F.);
#4702=ORIENTED_EDGE('',*,*,#3447,.T.);
#4703=ORIENTED_EDGE('',*,*,#3455,.T.);
#4704=ORIENTED_EDGE('',*,*,#3456,.T.);
#4705=ORIENTED_EDGE('',*,*,#3457,.F.);
#4706=ORIENTED_EDGE('',*,*,#3458,.F.);
#4707=ORIENTED_EDGE('',*,*,#3459,.F.);
#4708=ORIENTED_EDGE('',*,*,#3452,.T.);
#4709=ORIENTED_EDGE('',*,*,#3460,.T.);
#4710=ORIENTED_EDGE('',*,*,#3461,.T.);
#4711=ORIENTED_EDGE('',*,*,#3462,.F.);
#4712=ORIENTED_EDGE('',*,*,#3463,.F.);
#4713=ORIENTED_EDGE('',*,*,#3464,.F.);
#4714=ORIENTED_EDGE('',*,*,#3457,.T.);
#4715=ORIENTED_EDGE('',*,*,#3465,.T.);
#4716=ORIENTED_EDGE('',*,*,#3466,.T.);
#4717=ORIENTED_EDGE('',*,*,#3467,.F.);
#4718=ORIENTED_EDGE('',*,*,#3468,.F.);
#4719=ORIENTED_EDGE('',*,*,#3469,.F.);
#4720=ORIENTED_EDGE('',*,*,#3462,.T.);
#4721=ORIENTED_EDGE('',*,*,#3470,.T.);
#4722=ORIENTED_EDGE('',*,*,#3471,.T.);
#4723=ORIENTED_EDGE('',*,*,#3472,.F.);
#4724=ORIENTED_EDGE('',*,*,#3473,.F.);
#4725=ORIENTED_EDGE('',*,*,#3474,.F.);
#4726=ORIENTED_EDGE('',*,*,#3467,.T.);
#4727=ORIENTED_EDGE('',*,*,#3475,.T.);
#4728=ORIENTED_EDGE('',*,*,#3476,.T.);
#4729=ORIENTED_EDGE('',*,*,#3477,.F.);
#4730=ORIENTED_EDGE('',*,*,#3478,.F.);
#4731=ORIENTED_EDGE('',*,*,#3479,.F.);
#4732=ORIENTED_EDGE('',*,*,#3472,.T.);
#4733=ORIENTED_EDGE('',*,*,#3480,.T.);
#4734=ORIENTED_EDGE('',*,*,#3481,.T.);
#4735=ORIENTED_EDGE('',*,*,#3482,.F.);
#4736=ORIENTED_EDGE('',*,*,#3483,.F.);
#4737=ORIENTED_EDGE('',*,*,#3484,.F.);
#4738=ORIENTED_EDGE('',*,*,#3477,.T.);
#4739=ORIENTED_EDGE('',*,*,#3485,.T.);
#4740=ORIENTED_EDGE('',*,*,#3486,.T.);
#4741=ORIENTED_EDGE('',*,*,#3487,.F.);
#4742=ORIENTED_EDGE('',*,*,#3488,.F.);
#4743=ORIENTED_EDGE('',*,*,#3489,.F.);
#4744=ORIENTED_EDGE('',*,*,#3482,.T.);
#4745=ORIENTED_EDGE('',*,*,#3490,.T.);
#4746=ORIENTED_EDGE('',*,*,#3491,.T.);
#4747=ORIENTED_EDGE('',*,*,#3492,.F.);
#4748=ORIENTED_EDGE('',*,*,#3493,.F.);
#4749=ORIENTED_EDGE('',*,*,#3494,.F.);
#4750=ORIENTED_EDGE('',*,*,#3487,.T.);
#4751=ORIENTED_EDGE('',*,*,#3495,.T.);
#4752=ORIENTED_EDGE('',*,*,#3496,.T.);
#4753=ORIENTED_EDGE('',*,*,#3497,.F.);
#4754=ORIENTED_EDGE('',*,*,#3498,.F.);
#4755=ORIENTED_EDGE('',*,*,#3499,.F.);
#4756=ORIENTED_EDGE('',*,*,#3492,.T.);
#4757=ORIENTED_EDGE('',*,*,#3500,.T.);
#4758=ORIENTED_EDGE('',*,*,#3501,.T.);
#4759=ORIENTED_EDGE('',*,*,#3502,.F.);
#4760=ORIENTED_EDGE('',*,*,#3503,.F.);
#4761=ORIENTED_EDGE('',*,*,#3504,.F.);
#4762=ORIENTED_EDGE('',*,*,#3497,.T.);
#4763=ORIENTED_EDGE('',*,*,#3505,.T.);
#4764=ORIENTED_EDGE('',*,*,#3506,.T.);
#4765=ORIENTED_EDGE('',*,*,#3507,.F.);
#4766=ORIENTED_EDGE('',*,*,#3508,.F.);
#4767=ORIENTED_EDGE('',*,*,#3509,.F.);
#4768=ORIENTED_EDGE('',*,*,#3502,.T.);
#4769=ORIENTED_EDGE('',*,*,#3510,.T.);
#4770=ORIENTED_EDGE('',*,*,#3511,.T.);
#4771=ORIENTED_EDGE('',*,*,#3512,.F.);
#4772=ORIENTED_EDGE('',*,*,#3513,.F.);
#4773=ORIENTED_EDGE('',*,*,#3514,.F.);
#4774=ORIENTED_EDGE('',*,*,#3507,.T.);
#4775=ORIENTED_EDGE('',*,*,#3515,.T.);
#4776=ORIENTED_EDGE('',*,*,#3516,.T.);
#4777=ORIENTED_EDGE('',*,*,#3517,.F.);
#4778=ORIENTED_EDGE('',*,*,#3518,.F.);
#4779=ORIENTED_EDGE('',*,*,#3519,.F.);
#4780=ORIENTED_EDGE('',*,*,#3512,.T.);
#4781=ORIENTED_EDGE('',*,*,#3520,.T.);
#4782=ORIENTED_EDGE('',*,*,#3521,.T.);
#4783=ORIENTED_EDGE('',*,*,#3522,.F.);
#4784=ORIENTED_EDGE('',*,*,#3523,.F.);
#4785=ORIENTED_EDGE('',*,*,#3524,.F.);
#4786=ORIENTED_EDGE('',*,*,#3517,.T.);
#4787=ORIENTED_EDGE('',*,*,#3525,.T.);
#4788=ORIENTED_EDGE('',*,*,#3526,.T.);
#4789=ORIENTED_EDGE('',*,*,#3527,.F.);
#4790=ORIENTED_EDGE('',*,*,#3528,.F.);
#4791=ORIENTED_EDGE('',*,*,#3529,.F.);
#4792=ORIENTED_EDGE('',*,*,#3522,.T.);
#4793=ORIENTED_EDGE('',*,*,#3530,.T.);
#4794=ORIENTED_EDGE('',*,*,#3531,.T.);
#4795=ORIENTED_EDGE('',*,*,#3532,.F.);
#4796=ORIENTED_EDGE('',*,*,#3533,.F.);
#4797=ORIENTED_EDGE('',*,*,#3534,.F.);
#4798=ORIENTED_EDGE('',*,*,#3527,.T.);
#4799=ORIENTED_EDGE('',*,*,#3535,.T.);
#4800=ORIENTED_EDGE('',*,*,#3536,.T.);
#4801=ORIENTED_EDGE('',*,*,#3537,.F.);
#4802=ORIENTED_EDGE('',*,*,#3538,.F.);
#4803=ORIENTED_EDGE('',*,*,#3539,.F.);
#4804=ORIENTED_EDGE('',*,*,#3532,.T.);
#4805=ORIENTED_EDGE('',*,*,#3540,.T.);
#4806=ORIENTED_EDGE('',*,*,#3541,.T.);
#4807=ORIENTED_EDGE('',*,*,#3542,.F.);
#4808=ORIENTED_EDGE('',*,*,#3543,.F.);
#4809=ORIENTED_EDGE('',*,*,#3544,.F.);
#4810=ORIENTED_EDGE('',*,*,#3537,.T.);
#4811=ORIENTED_EDGE('',*,*,#3545,.T.);
#4812=ORIENTED_EDGE('',*,*,#3546,.T.);
#4813=ORIENTED_EDGE('',*,*,#3547,.F.);
#4814=ORIENTED_EDGE('',*,*,#3548,.F.);
#4815=ORIENTED_EDGE('',*,*,#3549,.F.);
#4816=ORIENTED_EDGE('',*,*,#3542,.T.);
#4817=ORIENTED_EDGE('',*,*,#3550,.T.);
#4818=ORIENTED_EDGE('',*,*,#3551,.T.);
#4819=ORIENTED_EDGE('',*,*,#3552,.F.);
#4820=ORIENTED_EDGE('',*,*,#3553,.F.);
#4821=ORIENTED_EDGE('',*,*,#3554,.F.);
#4822=ORIENTED_EDGE('',*,*,#3547,.T.);
#4823=ORIENTED_EDGE('',*,*,#3555,.T.);
#4824=ORIENTED_EDGE('',*,*,#3556,.T.);
#4825=ORIENTED_EDGE('',*,*,#3557,.F.);
#4826=ORIENTED_EDGE('',*,*,#3558,.F.);
#4827=ORIENTED_EDGE('',*,*,#3559,.F.);
#4828=ORIENTED_EDGE('',*,*,#3552,.T.);
#4829=ORIENTED_EDGE('',*,*,#3560,.T.);
#4830=ORIENTED_EDGE('',*,*,#3561,.T.);
#4831=ORIENTED_EDGE('',*,*,#3562,.F.);
#4832=ORIENTED_EDGE('',*,*,#3563,.F.);
#4833=ORIENTED_EDGE('',*,*,#3564,.F.);
#4834=ORIENTED_EDGE('',*,*,#3557,.T.);
#4835=ORIENTED_EDGE('',*,*,#3565,.T.);
#4836=ORIENTED_EDGE('',*,*,#3566,.T.);
#4837=ORIENTED_EDGE('',*,*,#3567,.F.);
#4838=ORIENTED_EDGE('',*,*,#3568,.F.);
#4839=ORIENTED_EDGE('',*,*,#3569,.F.);
#4840=ORIENTED_EDGE('',*,*,#3562,.T.);
#4841=ORIENTED_EDGE('',*,*,#3570,.T.);
#4842=ORIENTED_EDGE('',*,*,#3571,.T.);
#4843=ORIENTED_EDGE('',*,*,#3572,.F.);
#4844=ORIENTED_EDGE('',*,*,#3573,.F.);
#4845=ORIENTED_EDGE('',*,*,#3574,.F.);
#4846=ORIENTED_EDGE('',*,*,#3567,.T.);
#4847=ORIENTED_EDGE('',*,*,#3575,.T.);
#4848=ORIENTED_EDGE('',*,*,#3576,.T.);
#4849=ORIENTED_EDGE('',*,*,#3577,.F.);
#4850=ORIENTED_EDGE('',*,*,#3578,.F.);
#4851=ORIENTED_EDGE('',*,*,#3579,.F.);
#4852=ORIENTED_EDGE('',*,*,#3572,.T.);
#4853=ORIENTED_EDGE('',*,*,#3580,.T.);
#4854=ORIENTED_EDGE('',*,*,#3581,.T.);
#4855=ORIENTED_EDGE('',*,*,#3582,.F.);
#4856=ORIENTED_EDGE('',*,*,#3583,.F.);
#4857=ORIENTED_EDGE('',*,*,#3584,.F.);
#4858=ORIENTED_EDGE('',*,*,#3577,.T.);
#4859=ORIENTED_EDGE('',*,*,#3585,.T.);
#4860=ORIENTED_EDGE('',*,*,#3586,.T.);
#4861=ORIENTED_EDGE('',*,*,#3587,.F.);
#4862=ORIENTED_EDGE('',*,*,#3588,.F.);
#4863=ORIENTED_EDGE('',*,*,#3589,.F.);
#4864=ORIENTED_EDGE('',*,*,#3582,.T.);
#4865=ORIENTED_EDGE('',*,*,#3590,.T.);
#4866=ORIENTED_EDGE('',*,*,#3591,.T.);
#4867=ORIENTED_EDGE('',*,*,#3592,.F.);
#4868=ORIENTED_EDGE('',*,*,#3593,.F.);
#4869=ORIENTED_EDGE('',*,*,#3594,.F.);
#4870=ORIENTED_EDGE('',*,*,#3587,.T.);
#4871=ORIENTED_EDGE('',*,*,#3595,.T.);
#4872=ORIENTED_EDGE('',*,*,#3596,.T.);
#4873=ORIENTED_EDGE('',*,*,#3597,.F.);
#4874=ORIENTED_EDGE('',*,*,#3598,.F.);
#4875=ORIENTED_EDGE('',*,*,#3599,.F.);
#4876=ORIENTED_EDGE('',*,*,#3592,.T.);
#4877=ORIENTED_EDGE('',*,*,#3600,.T.);
#4878=ORIENTED_EDGE('',*,*,#3601,.T.);
#4879=ORIENTED_EDGE('',*,*,#3602,.F.);
#4880=ORIENTED_EDGE('',*,*,#3603,.F.);
#4881=ORIENTED_EDGE('',*,*,#3604,.F.);
#4882=ORIENTED_EDGE('',*,*,#3597,.T.);
#4883=ORIENTED_EDGE('',*,*,#3605,.T.);
#4884=ORIENTED_EDGE('',*,*,#3606,.T.);
#4885=ORIENTED_EDGE('',*,*,#3607,.F.);
#4886=ORIENTED_EDGE('',*,*,#3608,.F.);
#4887=ORIENTED_EDGE('',*,*,#3609,.F.);
#4888=ORIENTED_EDGE('',*,*,#3602,.T.);
#4889=ORIENTED_EDGE('',*,*,#3610,.T.);
#4890=ORIENTED_EDGE('',*,*,#3611,.T.);
#4891=ORIENTED_EDGE('',*,*,#3612,.F.);
#4892=ORIENTED_EDGE('',*,*,#3613,.F.);
#4893=ORIENTED_EDGE('',*,*,#3614,.F.);
#4894=ORIENTED_EDGE('',*,*,#3607,.T.);
#4895=ORIENTED_EDGE('',*,*,#3615,.T.);
#4896=ORIENTED_EDGE('',*,*,#3616,.T.);
#4897=ORIENTED_EDGE('',*,*,#3617,.F.);
#4898=ORIENTED_EDGE('',*,*,#3618,.F.);
#4899=ORIENTED_EDGE('',*,*,#3619,.F.);
#4900=ORIENTED_EDGE('',*,*,#3612,.T.);
#4901=ORIENTED_EDGE('',*,*,#3620,.T.);
#4902=ORIENTED_EDGE('',*,*,#3621,.T.);
#4903=ORIENTED_EDGE('',*,*,#3622,.F.);
#4904=ORIENTED_EDGE('',*,*,#3623,.F.);
#4905=ORIENTED_EDGE('',*,*,#3624,.F.);
#4906=ORIENTED_EDGE('',*,*,#3617,.T.);
#4907=ORIENTED_EDGE('',*,*,#3625,.T.);
#4908=ORIENTED_EDGE('',*,*,#3626,.T.);
#4909=ORIENTED_EDGE('',*,*,#3627,.F.);
#4910=ORIENTED_EDGE('',*,*,#3628,.F.);
#4911=ORIENTED_EDGE('',*,*,#3629,.F.);
#4912=ORIENTED_EDGE('',*,*,#3622,.T.);
#4913=ORIENTED_EDGE('',*,*,#3630,.T.);
#4914=ORIENTED_EDGE('',*,*,#3631,.T.);
#4915=ORIENTED_EDGE('',*,*,#3632,.F.);
#4916=ORIENTED_EDGE('',*,*,#3633,.F.);
#4917=ORIENTED_EDGE('',*,*,#3634,.F.);
#4918=ORIENTED_EDGE('',*,*,#3627,.T.);
#4919=ORIENTED_EDGE('',*,*,#3635,.T.);
#4920=ORIENTED_EDGE('',*,*,#3636,.T.);
#4921=ORIENTED_EDGE('',*,*,#3637,.F.);
#4922=ORIENTED_EDGE('',*,*,#3638,.F.);
#4923=ORIENTED_EDGE('',*,*,#3639,.F.);
#4924=ORIENTED_EDGE('',*,*,#3632,.T.);
#4925=ORIENTED_EDGE('',*,*,#3640,.T.);
#4926=ORIENTED_EDGE('',*,*,#3641,.T.);
#4927=ORIENTED_EDGE('',*,*,#3642,.F.);
#4928=ORIENTED_EDGE('',*,*,#3643,.F.);
#4929=ORIENTED_EDGE('',*,*,#3644,.F.);
#4930=ORIENTED_EDGE('',*,*,#3637,.T.);
#4931=ORIENTED_EDGE('',*,*,#3645,.T.);
#4932=ORIENTED_EDGE('',*,*,#3646,.T.);
#4933=ORIENTED_EDGE('',*,*,#3647,.F.);
#4934=ORIENTED_EDGE('',*,*,#3648,.F.);
#4935=ORIENTED_EDGE('',*,*,#3649,.F.);
#4936=ORIENTED_EDGE('',*,*,#3642,.T.);
#4937=ORIENTED_EDGE('',*,*,#3650,.T.);
#4938=ORIENTED_EDGE('',*,*,#3651,.T.);
#4939=ORIENTED_EDGE('',*,*,#3652,.F.);
#4940=ORIENTED_EDGE('',*,*,#3653,.F.);
#4941=ORIENTED_EDGE('',*,*,#3654,.F.);
#4942=ORIENTED_EDGE('',*,*,#3647,.T.);
#4943=ORIENTED_EDGE('',*,*,#3655,.T.);
#4944=ORIENTED_EDGE('',*,*,#3656,.T.);
#4945=ORIENTED_EDGE('',*,*,#3657,.F.);
#4946=ORIENTED_EDGE('',*,*,#3658,.F.);
#4947=ORIENTED_EDGE('',*,*,#3659,.F.);
#4948=ORIENTED_EDGE('',*,*,#3652,.T.);
#4949=ORIENTED_EDGE('',*,*,#3660,.T.);
#4950=ORIENTED_EDGE('',*,*,#3661,.T.);
#4951=ORIENTED_EDGE('',*,*,#3662,.F.);
#4952=ORIENTED_EDGE('',*,*,#3663,.F.);
#4953=ORIENTED_EDGE('',*,*,#3664,.F.);
#4954=ORIENTED_EDGE('',*,*,#3657,.T.);
#4955=ORIENTED_EDGE('',*,*,#3665,.T.);
#4956=ORIENTED_EDGE('',*,*,#3666,.T.);
#4957=ORIENTED_EDGE('',*,*,#3667,.F.);
#4958=ORIENTED_EDGE('',*,*,#3668,.F.);
#4959=ORIENTED_EDGE('',*,*,#3669,.F.);
#4960=ORIENTED_EDGE('',*,*,#3662,.T.);
#4961=ORIENTED_EDGE('',*,*,#3670,.T.);
#4962=ORIENTED_EDGE('',*,*,#3671,.T.);
#4963=ORIENTED_EDGE('',*,*,#3672,.F.);
#4964=ORIENTED_EDGE('',*,*,#3673,.F.);
#4965=ORIENTED_EDGE('',*,*,#3674,.F.);
#4966=ORIENTED_EDGE('',*,*,#3667,.T.);
#4967=ORIENTED_EDGE('',*,*,#3675,.T.);
#4968=ORIENTED_EDGE('',*,*,#3676,.T.);
#4969=ORIENTED_EDGE('',*,*,#3677,.F.);
#4970=ORIENTED_EDGE('',*,*,#3678,.F.);
#4971=ORIENTED_EDGE('',*,*,#3679,.F.);
#4972=ORIENTED_EDGE('',*,*,#3672,.T.);
#4973=ORIENTED_EDGE('',*,*,#3680,.T.);
#4974=ORIENTED_EDGE('',*,*,#3681,.T.);
#4975=ORIENTED_EDGE('',*,*,#3682,.F.);
#4976=ORIENTED_EDGE('',*,*,#3683,.F.);
#4977=ORIENTED_EDGE('',*,*,#3684,.F.);
#4978=ORIENTED_EDGE('',*,*,#3677,.T.);
#4979=ORIENTED_EDGE('',*,*,#3685,.T.);
#4980=ORIENTED_EDGE('',*,*,#3686,.T.);
#4981=ORIENTED_EDGE('',*,*,#3687,.F.);
#4982=ORIENTED_EDGE('',*,*,#3688,.F.);
#4983=ORIENTED_EDGE('',*,*,#3689,.F.);
#4984=ORIENTED_EDGE('',*,*,#3682,.T.);
#4985=ORIENTED_EDGE('',*,*,#3690,.T.);
#4986=ORIENTED_EDGE('',*,*,#3691,.T.);
#4987=ORIENTED_EDGE('',*,*,#3687,.T.);
#4988=ORIENTED_EDGE('',*,*,#3692,.T.);
#4989=ORIENTED_EDGE('',*,*,#3693,.T.);
#4990=ORIENTED_EDGE('',*,*,#3694,.F.);
#4991=ORIENTED_EDGE('',*,*,#3695,.F.);
#4992=ORIENTED_EDGE('',*,*,#3696,.F.);
#4993=ORIENTED_EDGE('',*,*,#3697,.T.);
#4994=ORIENTED_EDGE('',*,*,#3698,.T.);
#4995=ORIENTED_EDGE('',*,*,#3699,.T.);
#4996=ORIENTED_EDGE('',*,*,#3700,.T.);
#4997=ORIENTED_EDGE('',*,*,#3701,.T.);
#4998=ORIENTED_EDGE('',*,*,#3702,.T.);
#4999=ORIENTED_EDGE('',*,*,#3703,.T.);
#5000=ORIENTED_EDGE('',*,*,#3704,.T.);
#5001=ORIENTED_EDGE('',*,*,#3705,.T.);
#5002=ORIENTED_EDGE('',*,*,#3706,.T.);
#5003=ORIENTED_EDGE('',*,*,#3707,.T.);
#5004=ORIENTED_EDGE('',*,*,#3708,.T.);
#5005=ORIENTED_EDGE('',*,*,#3709,.T.);
#5006=ORIENTED_EDGE('',*,*,#3710,.T.);
#5007=ORIENTED_EDGE('',*,*,#3711,.T.);
#5008=ORIENTED_EDGE('',*,*,#3712,.T.);
#5009=ORIENTED_EDGE('',*,*,#3713,.T.);
#5010=ORIENTED_EDGE('',*,*,#3714,.T.);
#5011=ORIENTED_EDGE('',*,*,#3715,.T.);
#5012=ORIENTED_EDGE('',*,*,#3716,.T.);
#5013=ORIENTED_EDGE('',*,*,#3717,.T.);
#5014=ORIENTED_EDGE('',*,*,#3718,.T.);
#5015=ORIENTED_EDGE('',*,*,#3719,.T.);
#5016=ORIENTED_EDGE('',*,*,#3720,.T.);
#5017=ORIENTED_EDGE('',*,*,#3721,.T.);
#5018=ORIENTED_EDGE('',*,*,#3722,.T.);
#5019=ORIENTED_EDGE('',*,*,#3723,.T.);
#5020=ORIENTED_EDGE('',*,*,#3724,.T.);
#5021=ORIENTED_EDGE('',*,*,#3725,.T.);
#5022=ORIENTED_EDGE('',*,*,#3726,.T.);
#5023=ORIENTED_EDGE('',*,*,#3727,.T.);
#5024=ORIENTED_EDGE('',*,*,#3728,.T.);
#5025=ORIENTED_EDGE('',*,*,#3729,.T.);
#5026=ORIENTED_EDGE('',*,*,#3730,.T.);
#5027=ORIENTED_EDGE('',*,*,#3731,.T.);
#5028=ORIENTED_EDGE('',*,*,#3732,.T.);
#5029=ORIENTED_EDGE('',*,*,#3733,.T.);
#5030=ORIENTED_EDGE('',*,*,#3734,.T.);
#5031=ORIENTED_EDGE('',*,*,#3735,.T.);
#5032=ORIENTED_EDGE('',*,*,#3736,.T.);
#5033=ORIENTED_EDGE('',*,*,#3737,.T.);
#5034=ORIENTED_EDGE('',*,*,#3738,.T.);
#5035=ORIENTED_EDGE('',*,*,#3739,.T.);
#5036=ORIENTED_EDGE('',*,*,#3740,.T.);
#5037=ORIENTED_EDGE('',*,*,#3741,.T.);
#5038=ORIENTED_EDGE('',*,*,#3742,.T.);
#5039=ORIENTED_EDGE('',*,*,#3743,.T.);
#5040=ORIENTED_EDGE('',*,*,#3744,.T.);
#5041=ORIENTED_EDGE('',*,*,#3745,.T.);
#5042=ORIENTED_EDGE('',*,*,#3746,.T.);
#5043=ORIENTED_EDGE('',*,*,#3747,.T.);
#5044=ORIENTED_EDGE('',*,*,#3748,.T.);
#5045=ORIENTED_EDGE('',*,*,#3749,.T.);
#5046=ORIENTED_EDGE('',*,*,#3750,.T.);
#5047=ORIENTED_EDGE('',*,*,#3751,.T.);
#5048=ORIENTED_EDGE('',*,*,#3752,.T.);
#5049=ORIENTED_EDGE('',*,*,#3753,.T.);
#5050=ORIENTED_EDGE('',*,*,#3754,.T.);
#5051=ORIENTED_EDGE('',*,*,#3755,.T.);
#5052=ORIENTED_EDGE('',*,*,#3756,.T.);
#5053=ORIENTED_EDGE('',*,*,#3757,.T.);
#5054=ORIENTED_EDGE('',*,*,#3758,.T.);
#5055=ORIENTED_EDGE('',*,*,#3759,.T.);
#5056=ORIENTED_EDGE('',*,*,#3760,.T.);
#5057=ORIENTED_EDGE('',*,*,#3761,.T.);
#5058=ORIENTED_EDGE('',*,*,#3762,.T.);
#5059=ORIENTED_EDGE('',*,*,#3763,.T.);
#5060=ORIENTED_EDGE('',*,*,#3764,.T.);
#5061=ORIENTED_EDGE('',*,*,#3765,.T.);
#5062=ORIENTED_EDGE('',*,*,#3766,.T.);
#5063=ORIENTED_EDGE('',*,*,#3767,.T.);
#5064=ORIENTED_EDGE('',*,*,#3768,.T.);
#5065=ORIENTED_EDGE('',*,*,#3769,.T.);
#5066=ORIENTED_EDGE('',*,*,#3770,.T.);
#5067=ORIENTED_EDGE('',*,*,#3771,.T.);
#5068=ORIENTED_EDGE('',*,*,#3772,.T.);
#5069=ORIENTED_EDGE('',*,*,#3773,.T.);
#5070=ORIENTED_EDGE('',*,*,#3774,.T.);
#5071=ORIENTED_EDGE('',*,*,#3775,.T.);
#5072=ORIENTED_EDGE('',*,*,#3776,.T.);
#5073=ORIENTED_EDGE('',*,*,#3777,.T.);
#5074=ORIENTED_EDGE('',*,*,#3778,.T.);
#5075=ORIENTED_EDGE('',*,*,#3779,.T.);
#5076=ORIENTED_EDGE('',*,*,#3780,.T.);
#5077=ORIENTED_EDGE('',*,*,#3781,.T.);
#5078=ORIENTED_EDGE('',*,*,#3782,.T.);
#5079=ORIENTED_EDGE('',*,*,#3783,.T.);
#5080=ORIENTED_EDGE('',*,*,#3784,.T.);
#5081=ORIENTED_EDGE('',*,*,#3785,.T.);
#5082=ORIENTED_EDGE('',*,*,#3786,.T.);
#5083=ORIENTED_EDGE('',*,*,#3787,.T.);
#5084=ORIENTED_EDGE('',*,*,#3788,.T.);
#5085=ORIENTED_EDGE('',*,*,#3789,.T.);
#5086=ORIENTED_EDGE('',*,*,#3790,.T.);
#5087=ORIENTED_EDGE('',*,*,#3791,.T.);
#5088=ORIENTED_EDGE('',*,*,#3792,.T.);
#5089=ORIENTED_EDGE('',*,*,#3793,.T.);
#5090=ORIENTED_EDGE('',*,*,#3794,.T.);
#5091=ORIENTED_EDGE('',*,*,#3795,.T.);
#5092=ORIENTED_EDGE('',*,*,#3796,.T.);
#5093=ORIENTED_EDGE('',*,*,#3797,.T.);
#5094=ORIENTED_EDGE('',*,*,#3798,.T.);
#5095=ORIENTED_EDGE('',*,*,#3799,.T.);
#5096=ORIENTED_EDGE('',*,*,#3800,.T.);
#5097=ORIENTED_EDGE('',*,*,#3801,.T.);
#5098=ORIENTED_EDGE('',*,*,#3802,.T.);
#5099=ORIENTED_EDGE('',*,*,#3803,.T.);
#5100=ORIENTED_EDGE('',*,*,#3804,.T.);
#5101=ORIENTED_EDGE('',*,*,#3805,.T.);
#5102=ORIENTED_EDGE('',*,*,#3806,.T.);
#5103=ORIENTED_EDGE('',*,*,#3807,.T.);
#5104=ORIENTED_EDGE('',*,*,#3808,.T.);
#5105=ORIENTED_EDGE('',*,*,#3809,.T.);
#5106=ORIENTED_EDGE('',*,*,#3810,.T.);
#5107=ORIENTED_EDGE('',*,*,#3811,.T.);
#5108=ORIENTED_EDGE('',*,*,#3812,.T.);
#5109=ORIENTED_EDGE('',*,*,#3813,.T.);
#5110=ORIENTED_EDGE('',*,*,#3814,.T.);
#5111=ORIENTED_EDGE('',*,*,#3815,.T.);
#5112=ORIENTED_EDGE('',*,*,#3816,.T.);
#5113=ORIENTED_EDGE('',*,*,#3817,.T.);
#5114=ORIENTED_EDGE('',*,*,#3818,.T.);
#5115=ORIENTED_EDGE('',*,*,#3819,.T.);
#5116=ORIENTED_EDGE('',*,*,#3820,.T.);
#5117=ORIENTED_EDGE('',*,*,#3821,.T.);
#5118=ORIENTED_EDGE('',*,*,#3822,.T.);
#5119=ORIENTED_EDGE('',*,*,#3823,.T.);
#5120=ORIENTED_EDGE('',*,*,#3824,.T.);
#5121=ORIENTED_EDGE('',*,*,#3825,.T.);
#5122=ORIENTED_EDGE('',*,*,#3826,.T.);
#5123=ORIENTED_EDGE('',*,*,#3827,.T.);
#5124=ORIENTED_EDGE('',*,*,#3828,.T.);
#5125=ORIENTED_EDGE('',*,*,#3829,.T.);
#5126=ORIENTED_EDGE('',*,*,#3830,.T.);
#5127=ORIENTED_EDGE('',*,*,#3831,.T.);
#5128=ORIENTED_EDGE('',*,*,#3832,.T.);
#5129=ORIENTED_EDGE('',*,*,#3833,.T.);
#5130=ORIENTED_EDGE('',*,*,#3834,.T.);
#5131=ORIENTED_EDGE('',*,*,#3835,.T.);
#5132=ORIENTED_EDGE('',*,*,#3836,.T.);
#5133=ORIENTED_EDGE('',*,*,#3837,.T.);
#5134=ORIENTED_EDGE('',*,*,#3838,.T.);
#5135=ORIENTED_EDGE('',*,*,#3839,.T.);
#5136=ORIENTED_EDGE('',*,*,#3840,.F.);
#5137=ORIENTED_EDGE('',*,*,#3841,.T.);
#5138=ORIENTED_EDGE('',*,*,#3842,.T.);
#5139=ORIENTED_EDGE('',*,*,#3841,.F.);
#5140=ORIENTED_EDGE('',*,*,#3843,.F.);
#5141=ORIENTED_EDGE('',*,*,#3842,.F.);
#5142=ORIENTED_EDGE('',*,*,#3844,.F.);
#5143=ORIENTED_EDGE('',*,*,#3840,.T.);
#5144=ORIENTED_EDGE('',*,*,#3845,.F.);
#5145=ORIENTED_EDGE('',*,*,#3846,.T.);
#5146=ORIENTED_EDGE('',*,*,#3844,.T.);
#5147=ORIENTED_EDGE('',*,*,#3846,.F.);
#5148=ORIENTED_EDGE('',*,*,#3843,.T.);
#5149=ORIENTED_EDGE('',*,*,#3847,.T.);
#5150=ORIENTED_EDGE('',*,*,#3848,.F.);
#5151=ORIENTED_EDGE('',*,*,#3847,.F.);
#5152=ORIENTED_EDGE('',*,*,#3845,.T.);
#5153=ORIENTED_EDGE('',*,*,#3849,.F.);
#5154=ORIENTED_EDGE('',*,*,#3850,.T.);
#5155=ORIENTED_EDGE('',*,*,#3851,.T.);
#5156=ORIENTED_EDGE('',*,*,#3694,.T.);
#5157=ORIENTED_EDGE('',*,*,#3852,.T.);
#5158=ORIENTED_EDGE('',*,*,#3853,.F.);
#5159=ORIENTED_EDGE('',*,*,#3854,.T.);
#5160=ORIENTED_EDGE('',*,*,#3849,.T.);
#5161=ORIENTED_EDGE('',*,*,#3854,.F.);
#5162=ORIENTED_EDGE('',*,*,#3853,.T.);
#5163=ORIENTED_EDGE('',*,*,#3848,.T.);
#5164=ORIENTED_EDGE('',*,*,#3855,.F.);
#5165=ORIENTED_EDGE('',*,*,#3856,.T.);
#5166=ORIENTED_EDGE('',*,*,#3857,.F.);
#5167=ORIENTED_EDGE('',*,*,#3856,.F.);
#5168=ORIENTED_EDGE('',*,*,#3858,.F.);
#5169=ORIENTED_EDGE('',*,*,#3859,.T.);
#5170=ORIENTED_EDGE('',*,*,#3860,.F.);
#5171=ORIENTED_EDGE('',*,*,#3859,.F.);
#5172=ORIENTED_EDGE('',*,*,#3861,.F.);
#5173=ORIENTED_EDGE('',*,*,#3862,.T.);
#5174=ORIENTED_EDGE('',*,*,#3863,.F.);
#5175=ORIENTED_EDGE('',*,*,#3862,.F.);
#5176=ORIENTED_EDGE('',*,*,#3864,.F.);
#5177=ORIENTED_EDGE('',*,*,#3865,.T.);
#5178=ORIENTED_EDGE('',*,*,#3866,.F.);
#5179=ORIENTED_EDGE('',*,*,#3865,.F.);
#5180=ORIENTED_EDGE('',*,*,#3867,.F.);
#5181=ORIENTED_EDGE('',*,*,#3850,.F.);
#5182=ORIENTED_EDGE('',*,*,#3868,.F.);
#5183=ORIENTED_EDGE('',*,*,#3777,.F.);
#5184=ORIENTED_EDGE('',*,*,#3868,.T.);
#5185=ORIENTED_EDGE('',*,*,#3852,.F.);
#5186=ORIENTED_EDGE('',*,*,#3693,.F.);
#5187=ORIENTED_EDGE('',*,*,#3692,.F.);
#5188=ORIENTED_EDGE('',*,*,#3691,.F.);
#5189=ORIENTED_EDGE('',*,*,#3690,.F.);
#5190=ORIENTED_EDGE('',*,*,#3686,.F.);
#5191=ORIENTED_EDGE('',*,*,#3685,.F.);
#5192=ORIENTED_EDGE('',*,*,#3681,.F.);
#5193=ORIENTED_EDGE('',*,*,#3680,.F.);
#5194=ORIENTED_EDGE('',*,*,#3676,.F.);
#5195=ORIENTED_EDGE('',*,*,#3675,.F.);
#5196=ORIENTED_EDGE('',*,*,#3671,.F.);
#5197=ORIENTED_EDGE('',*,*,#3670,.F.);
#5198=ORIENTED_EDGE('',*,*,#3666,.F.);
#5199=ORIENTED_EDGE('',*,*,#3665,.F.);
#5200=ORIENTED_EDGE('',*,*,#3661,.F.);
#5201=ORIENTED_EDGE('',*,*,#3660,.F.);
#5202=ORIENTED_EDGE('',*,*,#3656,.F.);
#5203=ORIENTED_EDGE('',*,*,#3655,.F.);
#5204=ORIENTED_EDGE('',*,*,#3651,.F.);
#5205=ORIENTED_EDGE('',*,*,#3650,.F.);
#5206=ORIENTED_EDGE('',*,*,#3646,.F.);
#5207=ORIENTED_EDGE('',*,*,#3645,.F.);
#5208=ORIENTED_EDGE('',*,*,#3641,.F.);
#5209=ORIENTED_EDGE('',*,*,#3640,.F.);
#5210=ORIENTED_EDGE('',*,*,#3636,.F.);
#5211=ORIENTED_EDGE('',*,*,#3635,.F.);
#5212=ORIENTED_EDGE('',*,*,#3631,.F.);
#5213=ORIENTED_EDGE('',*,*,#3630,.F.);
#5214=ORIENTED_EDGE('',*,*,#3626,.F.);
#5215=ORIENTED_EDGE('',*,*,#3625,.F.);
#5216=ORIENTED_EDGE('',*,*,#3621,.F.);
#5217=ORIENTED_EDGE('',*,*,#3620,.F.);
#5218=ORIENTED_EDGE('',*,*,#3616,.F.);
#5219=ORIENTED_EDGE('',*,*,#3615,.F.);
#5220=ORIENTED_EDGE('',*,*,#3611,.F.);
#5221=ORIENTED_EDGE('',*,*,#3610,.F.);
#5222=ORIENTED_EDGE('',*,*,#3606,.F.);
#5223=ORIENTED_EDGE('',*,*,#3605,.F.);
#5224=ORIENTED_EDGE('',*,*,#3601,.F.);
#5225=ORIENTED_EDGE('',*,*,#3600,.F.);
#5226=ORIENTED_EDGE('',*,*,#3596,.F.);
#5227=ORIENTED_EDGE('',*,*,#3595,.F.);
#5228=ORIENTED_EDGE('',*,*,#3591,.F.);
#5229=ORIENTED_EDGE('',*,*,#3590,.F.);
#5230=ORIENTED_EDGE('',*,*,#3586,.F.);
#5231=ORIENTED_EDGE('',*,*,#3585,.F.);
#5232=ORIENTED_EDGE('',*,*,#3581,.F.);
#5233=ORIENTED_EDGE('',*,*,#3580,.F.);
#5234=ORIENTED_EDGE('',*,*,#3576,.F.);
#5235=ORIENTED_EDGE('',*,*,#3575,.F.);
#5236=ORIENTED_EDGE('',*,*,#3571,.F.);
#5237=ORIENTED_EDGE('',*,*,#3570,.F.);
#5238=ORIENTED_EDGE('',*,*,#3566,.F.);
#5239=ORIENTED_EDGE('',*,*,#3565,.F.);
#5240=ORIENTED_EDGE('',*,*,#3561,.F.);
#5241=ORIENTED_EDGE('',*,*,#3560,.F.);
#5242=ORIENTED_EDGE('',*,*,#3556,.F.);
#5243=ORIENTED_EDGE('',*,*,#3555,.F.);
#5244=ORIENTED_EDGE('',*,*,#3551,.F.);
#5245=ORIENTED_EDGE('',*,*,#3550,.F.);
#5246=ORIENTED_EDGE('',*,*,#3546,.F.);
#5247=ORIENTED_EDGE('',*,*,#3545,.F.);
#5248=ORIENTED_EDGE('',*,*,#3541,.F.);
#5249=ORIENTED_EDGE('',*,*,#3540,.F.);
#5250=ORIENTED_EDGE('',*,*,#3536,.F.);
#5251=ORIENTED_EDGE('',*,*,#3535,.F.);
#5252=ORIENTED_EDGE('',*,*,#3531,.F.);
#5253=ORIENTED_EDGE('',*,*,#3530,.F.);
#5254=ORIENTED_EDGE('',*,*,#3526,.F.);
#5255=ORIENTED_EDGE('',*,*,#3525,.F.);
#5256=ORIENTED_EDGE('',*,*,#3521,.F.);
#5257=ORIENTED_EDGE('',*,*,#3520,.F.);
#5258=ORIENTED_EDGE('',*,*,#3516,.F.);
#5259=ORIENTED_EDGE('',*,*,#3515,.F.);
#5260=ORIENTED_EDGE('',*,*,#3511,.F.);
#5261=ORIENTED_EDGE('',*,*,#3510,.F.);
#5262=ORIENTED_EDGE('',*,*,#3506,.F.);
#5263=ORIENTED_EDGE('',*,*,#3505,.F.);
#5264=ORIENTED_EDGE('',*,*,#3501,.F.);
#5265=ORIENTED_EDGE('',*,*,#3500,.F.);
#5266=ORIENTED_EDGE('',*,*,#3496,.F.);
#5267=ORIENTED_EDGE('',*,*,#3495,.F.);
#5268=ORIENTED_EDGE('',*,*,#3491,.F.);
#5269=ORIENTED_EDGE('',*,*,#3490,.F.);
#5270=ORIENTED_EDGE('',*,*,#3486,.F.);
#5271=ORIENTED_EDGE('',*,*,#3485,.F.);
#5272=ORIENTED_EDGE('',*,*,#3481,.F.);
#5273=ORIENTED_EDGE('',*,*,#3480,.F.);
#5274=ORIENTED_EDGE('',*,*,#3476,.F.);
#5275=ORIENTED_EDGE('',*,*,#3475,.F.);
#5276=ORIENTED_EDGE('',*,*,#3471,.F.);
#5277=ORIENTED_EDGE('',*,*,#3470,.F.);
#5278=ORIENTED_EDGE('',*,*,#3466,.F.);
#5279=ORIENTED_EDGE('',*,*,#3465,.F.);
#5280=ORIENTED_EDGE('',*,*,#3461,.F.);
#5281=ORIENTED_EDGE('',*,*,#3460,.F.);
#5282=ORIENTED_EDGE('',*,*,#3456,.F.);
#5283=ORIENTED_EDGE('',*,*,#3455,.F.);
#5284=ORIENTED_EDGE('',*,*,#3451,.F.);
#5285=ORIENTED_EDGE('',*,*,#3450,.F.);
#5286=ORIENTED_EDGE('',*,*,#3446,.F.);
#5287=ORIENTED_EDGE('',*,*,#3445,.F.);
#5288=ORIENTED_EDGE('',*,*,#3441,.F.);
#5289=ORIENTED_EDGE('',*,*,#3440,.F.);
#5290=ORIENTED_EDGE('',*,*,#3436,.F.);
#5291=ORIENTED_EDGE('',*,*,#3435,.F.);
#5292=ORIENTED_EDGE('',*,*,#3431,.F.);
#5293=ORIENTED_EDGE('',*,*,#3430,.F.);
#5294=ORIENTED_EDGE('',*,*,#3426,.F.);
#5295=ORIENTED_EDGE('',*,*,#3425,.F.);
#5296=ORIENTED_EDGE('',*,*,#3421,.F.);
#5297=ORIENTED_EDGE('',*,*,#3420,.F.);
#5298=ORIENTED_EDGE('',*,*,#3416,.F.);
#5299=ORIENTED_EDGE('',*,*,#3415,.F.);
#5300=ORIENTED_EDGE('',*,*,#3411,.F.);
#5301=ORIENTED_EDGE('',*,*,#3410,.F.);
#5302=ORIENTED_EDGE('',*,*,#3406,.F.);
#5303=ORIENTED_EDGE('',*,*,#3405,.F.);
#5304=ORIENTED_EDGE('',*,*,#3401,.F.);
#5305=ORIENTED_EDGE('',*,*,#3400,.F.);
#5306=ORIENTED_EDGE('',*,*,#3396,.F.);
#5307=ORIENTED_EDGE('',*,*,#3395,.F.);
#5308=ORIENTED_EDGE('',*,*,#3391,.F.);
#5309=ORIENTED_EDGE('',*,*,#3390,.F.);
#5310=ORIENTED_EDGE('',*,*,#3386,.F.);
#5311=ORIENTED_EDGE('',*,*,#3385,.F.);
#5312=ORIENTED_EDGE('',*,*,#3381,.F.);
#5313=ORIENTED_EDGE('',*,*,#3380,.F.);
#5314=ORIENTED_EDGE('',*,*,#3376,.F.);
#5315=ORIENTED_EDGE('',*,*,#3375,.F.);
#5316=ORIENTED_EDGE('',*,*,#3371,.F.);
#5317=ORIENTED_EDGE('',*,*,#3370,.F.);
#5318=ORIENTED_EDGE('',*,*,#3366,.F.);
#5319=ORIENTED_EDGE('',*,*,#3365,.F.);
#5320=ORIENTED_EDGE('',*,*,#3361,.F.);
#5321=ORIENTED_EDGE('',*,*,#3360,.F.);
#5322=ORIENTED_EDGE('',*,*,#3356,.F.);
#5323=ORIENTED_EDGE('',*,*,#3355,.F.);
#5324=ORIENTED_EDGE('',*,*,#3351,.F.);
#5325=ORIENTED_EDGE('',*,*,#3350,.F.);
#5326=ORIENTED_EDGE('',*,*,#3346,.F.);
#5327=ORIENTED_EDGE('',*,*,#3345,.F.);
#5328=ORIENTED_EDGE('',*,*,#3341,.F.);
#5329=ORIENTED_EDGE('',*,*,#3340,.F.);
#5330=ORIENTED_EDGE('',*,*,#3336,.F.);
#5331=ORIENTED_EDGE('',*,*,#3335,.F.);
#5332=ORIENTED_EDGE('',*,*,#3331,.F.);
#5333=ORIENTED_EDGE('',*,*,#3330,.F.);
#5334=ORIENTED_EDGE('',*,*,#3326,.F.);
#5335=ORIENTED_EDGE('',*,*,#3325,.F.);
#5336=ORIENTED_EDGE('',*,*,#3321,.F.);
#5337=ORIENTED_EDGE('',*,*,#3320,.F.);
#5338=ORIENTED_EDGE('',*,*,#3316,.F.);
#5339=ORIENTED_EDGE('',*,*,#3315,.F.);
#5340=ORIENTED_EDGE('',*,*,#3311,.F.);
#5341=ORIENTED_EDGE('',*,*,#3869,.F.);
#5342=ORIENTED_EDGE('',*,*,#3697,.F.);
#5343=ORIENTED_EDGE('',*,*,#3839,.F.);
#5344=ORIENTED_EDGE('',*,*,#3838,.F.);
#5345=ORIENTED_EDGE('',*,*,#3837,.F.);
#5346=ORIENTED_EDGE('',*,*,#3836,.F.);
#5347=ORIENTED_EDGE('',*,*,#3835,.F.);
#5348=ORIENTED_EDGE('',*,*,#3834,.F.);
#5349=ORIENTED_EDGE('',*,*,#3833,.F.);
#5350=ORIENTED_EDGE('',*,*,#3832,.F.);
#5351=ORIENTED_EDGE('',*,*,#3831,.F.);
#5352=ORIENTED_EDGE('',*,*,#3830,.F.);
#5353=ORIENTED_EDGE('',*,*,#3829,.F.);
#5354=ORIENTED_EDGE('',*,*,#3828,.F.);
#5355=ORIENTED_EDGE('',*,*,#3827,.F.);
#5356=ORIENTED_EDGE('',*,*,#3826,.F.);
#5357=ORIENTED_EDGE('',*,*,#3825,.F.);
#5358=ORIENTED_EDGE('',*,*,#3824,.F.);
#5359=ORIENTED_EDGE('',*,*,#3823,.F.);
#5360=ORIENTED_EDGE('',*,*,#3822,.F.);
#5361=ORIENTED_EDGE('',*,*,#3821,.F.);
#5362=ORIENTED_EDGE('',*,*,#3820,.F.);
#5363=ORIENTED_EDGE('',*,*,#3819,.F.);
#5364=ORIENTED_EDGE('',*,*,#3818,.F.);
#5365=ORIENTED_EDGE('',*,*,#3817,.F.);
#5366=ORIENTED_EDGE('',*,*,#3816,.F.);
#5367=ORIENTED_EDGE('',*,*,#3815,.F.);
#5368=ORIENTED_EDGE('',*,*,#3814,.F.);
#5369=ORIENTED_EDGE('',*,*,#3813,.F.);
#5370=ORIENTED_EDGE('',*,*,#3812,.F.);
#5371=ORIENTED_EDGE('',*,*,#3811,.F.);
#5372=ORIENTED_EDGE('',*,*,#3810,.F.);
#5373=ORIENTED_EDGE('',*,*,#3809,.F.);
#5374=ORIENTED_EDGE('',*,*,#3808,.F.);
#5375=ORIENTED_EDGE('',*,*,#3807,.F.);
#5376=ORIENTED_EDGE('',*,*,#3806,.F.);
#5377=ORIENTED_EDGE('',*,*,#3805,.F.);
#5378=ORIENTED_EDGE('',*,*,#3804,.F.);
#5379=ORIENTED_EDGE('',*,*,#3803,.F.);
#5380=ORIENTED_EDGE('',*,*,#3802,.F.);
#5381=ORIENTED_EDGE('',*,*,#3801,.F.);
#5382=ORIENTED_EDGE('',*,*,#3800,.F.);
#5383=ORIENTED_EDGE('',*,*,#3799,.F.);
#5384=ORIENTED_EDGE('',*,*,#3798,.F.);
#5385=ORIENTED_EDGE('',*,*,#3797,.F.);
#5386=ORIENTED_EDGE('',*,*,#3796,.F.);
#5387=ORIENTED_EDGE('',*,*,#3795,.F.);
#5388=ORIENTED_EDGE('',*,*,#3794,.F.);
#5389=ORIENTED_EDGE('',*,*,#3793,.F.);
#5390=ORIENTED_EDGE('',*,*,#3792,.F.);
#5391=ORIENTED_EDGE('',*,*,#3791,.F.);
#5392=ORIENTED_EDGE('',*,*,#3790,.F.);
#5393=ORIENTED_EDGE('',*,*,#3789,.F.);
#5394=ORIENTED_EDGE('',*,*,#3788,.F.);
#5395=ORIENTED_EDGE('',*,*,#3787,.F.);
#5396=ORIENTED_EDGE('',*,*,#3786,.F.);
#5397=ORIENTED_EDGE('',*,*,#3785,.F.);
#5398=ORIENTED_EDGE('',*,*,#3784,.F.);
#5399=ORIENTED_EDGE('',*,*,#3783,.F.);
#5400=ORIENTED_EDGE('',*,*,#3782,.F.);
#5401=ORIENTED_EDGE('',*,*,#3781,.F.);
#5402=ORIENTED_EDGE('',*,*,#3780,.F.);
#5403=ORIENTED_EDGE('',*,*,#3779,.F.);
#5404=ORIENTED_EDGE('',*,*,#3778,.F.);
#5405=ORIENTED_EDGE('',*,*,#3867,.T.);
#5406=ORIENTED_EDGE('',*,*,#3776,.F.);
#5407=ORIENTED_EDGE('',*,*,#3775,.F.);
#5408=ORIENTED_EDGE('',*,*,#3774,.F.);
#5409=ORIENTED_EDGE('',*,*,#3773,.F.);
#5410=ORIENTED_EDGE('',*,*,#3772,.F.);
#5411=ORIENTED_EDGE('',*,*,#3771,.F.);
#5412=ORIENTED_EDGE('',*,*,#3770,.F.);
#5413=ORIENTED_EDGE('',*,*,#3769,.F.);
#5414=ORIENTED_EDGE('',*,*,#3768,.F.);
#5415=ORIENTED_EDGE('',*,*,#3767,.F.);
#5416=ORIENTED_EDGE('',*,*,#3766,.F.);
#5417=ORIENTED_EDGE('',*,*,#3765,.F.);
#5418=ORIENTED_EDGE('',*,*,#3764,.F.);
#5419=ORIENTED_EDGE('',*,*,#3763,.F.);
#5420=ORIENTED_EDGE('',*,*,#3762,.F.);
#5421=ORIENTED_EDGE('',*,*,#3761,.F.);
#5422=ORIENTED_EDGE('',*,*,#3760,.F.);
#5423=ORIENTED_EDGE('',*,*,#3759,.F.);
#5424=ORIENTED_EDGE('',*,*,#3758,.F.);
#5425=ORIENTED_EDGE('',*,*,#3757,.F.);
#5426=ORIENTED_EDGE('',*,*,#3756,.F.);
#5427=ORIENTED_EDGE('',*,*,#3755,.F.);
#5428=ORIENTED_EDGE('',*,*,#3754,.F.);
#5429=ORIENTED_EDGE('',*,*,#3753,.F.);
#5430=ORIENTED_EDGE('',*,*,#3752,.F.);
#5431=ORIENTED_EDGE('',*,*,#3751,.F.);
#5432=ORIENTED_EDGE('',*,*,#3750,.F.);
#5433=ORIENTED_EDGE('',*,*,#3749,.F.);
#5434=ORIENTED_EDGE('',*,*,#3748,.F.);
#5435=ORIENTED_EDGE('',*,*,#3747,.F.);
#5436=ORIENTED_EDGE('',*,*,#3746,.F.);
#5437=ORIENTED_EDGE('',*,*,#3745,.F.);
#5438=ORIENTED_EDGE('',*,*,#3744,.F.);
#5439=ORIENTED_EDGE('',*,*,#3743,.F.);
#5440=ORIENTED_EDGE('',*,*,#3742,.F.);
#5441=ORIENTED_EDGE('',*,*,#3741,.F.);
#5442=ORIENTED_EDGE('',*,*,#3740,.F.);
#5443=ORIENTED_EDGE('',*,*,#3739,.F.);
#5444=ORIENTED_EDGE('',*,*,#3738,.F.);
#5445=ORIENTED_EDGE('',*,*,#3737,.F.);
#5446=ORIENTED_EDGE('',*,*,#3736,.F.);
#5447=ORIENTED_EDGE('',*,*,#3735,.F.);
#5448=ORIENTED_EDGE('',*,*,#3734,.F.);
#5449=ORIENTED_EDGE('',*,*,#3733,.F.);
#5450=ORIENTED_EDGE('',*,*,#3732,.F.);
#5451=ORIENTED_EDGE('',*,*,#3731,.F.);
#5452=ORIENTED_EDGE('',*,*,#3730,.F.);
#5453=ORIENTED_EDGE('',*,*,#3729,.F.);
#5454=ORIENTED_EDGE('',*,*,#3728,.F.);
#5455=ORIENTED_EDGE('',*,*,#3727,.F.);
#5456=ORIENTED_EDGE('',*,*,#3726,.F.);
#5457=ORIENTED_EDGE('',*,*,#3725,.F.);
#5458=ORIENTED_EDGE('',*,*,#3724,.F.);
#5459=ORIENTED_EDGE('',*,*,#3723,.F.);
#5460=ORIENTED_EDGE('',*,*,#3722,.F.);
#5461=ORIENTED_EDGE('',*,*,#3721,.F.);
#5462=ORIENTED_EDGE('',*,*,#3720,.F.);
#5463=ORIENTED_EDGE('',*,*,#3719,.F.);
#5464=ORIENTED_EDGE('',*,*,#3718,.F.);
#5465=ORIENTED_EDGE('',*,*,#3717,.F.);
#5466=ORIENTED_EDGE('',*,*,#3716,.F.);
#5467=ORIENTED_EDGE('',*,*,#3715,.F.);
#5468=ORIENTED_EDGE('',*,*,#3714,.F.);
#5469=ORIENTED_EDGE('',*,*,#3713,.F.);
#5470=ORIENTED_EDGE('',*,*,#3712,.F.);
#5471=ORIENTED_EDGE('',*,*,#3711,.F.);
#5472=ORIENTED_EDGE('',*,*,#3710,.F.);
#5473=ORIENTED_EDGE('',*,*,#3709,.F.);
#5474=ORIENTED_EDGE('',*,*,#3708,.F.);
#5475=ORIENTED_EDGE('',*,*,#3707,.F.);
#5476=ORIENTED_EDGE('',*,*,#3706,.F.);
#5477=ORIENTED_EDGE('',*,*,#3705,.F.);
#5478=ORIENTED_EDGE('',*,*,#3704,.F.);
#5479=ORIENTED_EDGE('',*,*,#3703,.F.);
#5480=ORIENTED_EDGE('',*,*,#3702,.F.);
#5481=ORIENTED_EDGE('',*,*,#3701,.F.);
#5482=ORIENTED_EDGE('',*,*,#3700,.F.);
#5483=ORIENTED_EDGE('',*,*,#3699,.F.);
#5484=ORIENTED_EDGE('',*,*,#3870,.F.);
#5485=ORIENTED_EDGE('',*,*,#3309,.T.);
#5486=ORIENTED_EDGE('',*,*,#3314,.T.);
#5487=ORIENTED_EDGE('',*,*,#3313,.T.);
#5488=ORIENTED_EDGE('',*,*,#3319,.T.);
#5489=ORIENTED_EDGE('',*,*,#3318,.T.);
#5490=ORIENTED_EDGE('',*,*,#3324,.T.);
#5491=ORIENTED_EDGE('',*,*,#3323,.T.);
#5492=ORIENTED_EDGE('',*,*,#3329,.T.);
#5493=ORIENTED_EDGE('',*,*,#3328,.T.);
#5494=ORIENTED_EDGE('',*,*,#3334,.T.);
#5495=ORIENTED_EDGE('',*,*,#3333,.T.);
#5496=ORIENTED_EDGE('',*,*,#3339,.T.);
#5497=ORIENTED_EDGE('',*,*,#3338,.T.);
#5498=ORIENTED_EDGE('',*,*,#3344,.T.);
#5499=ORIENTED_EDGE('',*,*,#3343,.T.);
#5500=ORIENTED_EDGE('',*,*,#3349,.T.);
#5501=ORIENTED_EDGE('',*,*,#3348,.T.);
#5502=ORIENTED_EDGE('',*,*,#3354,.T.);
#5503=ORIENTED_EDGE('',*,*,#3353,.T.);
#5504=ORIENTED_EDGE('',*,*,#3359,.T.);
#5505=ORIENTED_EDGE('',*,*,#3358,.T.);
#5506=ORIENTED_EDGE('',*,*,#3364,.T.);
#5507=ORIENTED_EDGE('',*,*,#3363,.T.);
#5508=ORIENTED_EDGE('',*,*,#3369,.T.);
#5509=ORIENTED_EDGE('',*,*,#3368,.T.);
#5510=ORIENTED_EDGE('',*,*,#3374,.T.);
#5511=ORIENTED_EDGE('',*,*,#3373,.T.);
#5512=ORIENTED_EDGE('',*,*,#3379,.T.);
#5513=ORIENTED_EDGE('',*,*,#3378,.T.);
#5514=ORIENTED_EDGE('',*,*,#3384,.T.);
#5515=ORIENTED_EDGE('',*,*,#3383,.T.);
#5516=ORIENTED_EDGE('',*,*,#3389,.T.);
#5517=ORIENTED_EDGE('',*,*,#3388,.T.);
#5518=ORIENTED_EDGE('',*,*,#3394,.T.);
#5519=ORIENTED_EDGE('',*,*,#3393,.T.);
#5520=ORIENTED_EDGE('',*,*,#3399,.T.);
#5521=ORIENTED_EDGE('',*,*,#3398,.T.);
#5522=ORIENTED_EDGE('',*,*,#3404,.T.);
#5523=ORIENTED_EDGE('',*,*,#3403,.T.);
#5524=ORIENTED_EDGE('',*,*,#3409,.T.);
#5525=ORIENTED_EDGE('',*,*,#3408,.T.);
#5526=ORIENTED_EDGE('',*,*,#3414,.T.);
#5527=ORIENTED_EDGE('',*,*,#3413,.T.);
#5528=ORIENTED_EDGE('',*,*,#3419,.T.);
#5529=ORIENTED_EDGE('',*,*,#3418,.T.);
#5530=ORIENTED_EDGE('',*,*,#3424,.T.);
#5531=ORIENTED_EDGE('',*,*,#3423,.T.);
#5532=ORIENTED_EDGE('',*,*,#3429,.T.);
#5533=ORIENTED_EDGE('',*,*,#3428,.T.);
#5534=ORIENTED_EDGE('',*,*,#3434,.T.);
#5535=ORIENTED_EDGE('',*,*,#3433,.T.);
#5536=ORIENTED_EDGE('',*,*,#3439,.T.);
#5537=ORIENTED_EDGE('',*,*,#3438,.T.);
#5538=ORIENTED_EDGE('',*,*,#3444,.T.);
#5539=ORIENTED_EDGE('',*,*,#3443,.T.);
#5540=ORIENTED_EDGE('',*,*,#3449,.T.);
#5541=ORIENTED_EDGE('',*,*,#3448,.T.);
#5542=ORIENTED_EDGE('',*,*,#3454,.T.);
#5543=ORIENTED_EDGE('',*,*,#3453,.T.);
#5544=ORIENTED_EDGE('',*,*,#3459,.T.);
#5545=ORIENTED_EDGE('',*,*,#3458,.T.);
#5546=ORIENTED_EDGE('',*,*,#3464,.T.);
#5547=ORIENTED_EDGE('',*,*,#3463,.T.);
#5548=ORIENTED_EDGE('',*,*,#3469,.T.);
#5549=ORIENTED_EDGE('',*,*,#3468,.T.);
#5550=ORIENTED_EDGE('',*,*,#3474,.T.);
#5551=ORIENTED_EDGE('',*,*,#3473,.T.);
#5552=ORIENTED_EDGE('',*,*,#3479,.T.);
#5553=ORIENTED_EDGE('',*,*,#3478,.T.);
#5554=ORIENTED_EDGE('',*,*,#3484,.T.);
#5555=ORIENTED_EDGE('',*,*,#3483,.T.);
#5556=ORIENTED_EDGE('',*,*,#3489,.T.);
#5557=ORIENTED_EDGE('',*,*,#3488,.T.);
#5558=ORIENTED_EDGE('',*,*,#3494,.T.);
#5559=ORIENTED_EDGE('',*,*,#3493,.T.);
#5560=ORIENTED_EDGE('',*,*,#3499,.T.);
#5561=ORIENTED_EDGE('',*,*,#3498,.T.);
#5562=ORIENTED_EDGE('',*,*,#3504,.T.);
#5563=ORIENTED_EDGE('',*,*,#3503,.T.);
#5564=ORIENTED_EDGE('',*,*,#3509,.T.);
#5565=ORIENTED_EDGE('',*,*,#3508,.T.);
#5566=ORIENTED_EDGE('',*,*,#3514,.T.);
#5567=ORIENTED_EDGE('',*,*,#3513,.T.);
#5568=ORIENTED_EDGE('',*,*,#3519,.T.);
#5569=ORIENTED_EDGE('',*,*,#3518,.T.);
#5570=ORIENTED_EDGE('',*,*,#3524,.T.);
#5571=ORIENTED_EDGE('',*,*,#3523,.T.);
#5572=ORIENTED_EDGE('',*,*,#3529,.T.);
#5573=ORIENTED_EDGE('',*,*,#3528,.T.);
#5574=ORIENTED_EDGE('',*,*,#3534,.T.);
#5575=ORIENTED_EDGE('',*,*,#3533,.T.);
#5576=ORIENTED_EDGE('',*,*,#3539,.T.);
#5577=ORIENTED_EDGE('',*,*,#3538,.T.);
#5578=ORIENTED_EDGE('',*,*,#3544,.T.);
#5579=ORIENTED_EDGE('',*,*,#3543,.T.);
#5580=ORIENTED_EDGE('',*,*,#3549,.T.);
#5581=ORIENTED_EDGE('',*,*,#3548,.T.);
#5582=ORIENTED_EDGE('',*,*,#3554,.T.);
#5583=ORIENTED_EDGE('',*,*,#3553,.T.);
#5584=ORIENTED_EDGE('',*,*,#3559,.T.);
#5585=ORIENTED_EDGE('',*,*,#3558,.T.);
#5586=ORIENTED_EDGE('',*,*,#3564,.T.);
#5587=ORIENTED_EDGE('',*,*,#3563,.T.);
#5588=ORIENTED_EDGE('',*,*,#3569,.T.);
#5589=ORIENTED_EDGE('',*,*,#3568,.T.);
#5590=ORIENTED_EDGE('',*,*,#3574,.T.);
#5591=ORIENTED_EDGE('',*,*,#3573,.T.);
#5592=ORIENTED_EDGE('',*,*,#3579,.T.);
#5593=ORIENTED_EDGE('',*,*,#3578,.T.);
#5594=ORIENTED_EDGE('',*,*,#3584,.T.);
#5595=ORIENTED_EDGE('',*,*,#3583,.T.);
#5596=ORIENTED_EDGE('',*,*,#3589,.T.);
#5597=ORIENTED_EDGE('',*,*,#3588,.T.);
#5598=ORIENTED_EDGE('',*,*,#3594,.T.);
#5599=ORIENTED_EDGE('',*,*,#3593,.T.);
#5600=ORIENTED_EDGE('',*,*,#3599,.T.);
#5601=ORIENTED_EDGE('',*,*,#3598,.T.);
#5602=ORIENTED_EDGE('',*,*,#3604,.T.);
#5603=ORIENTED_EDGE('',*,*,#3603,.T.);
#5604=ORIENTED_EDGE('',*,*,#3609,.T.);
#5605=ORIENTED_EDGE('',*,*,#3608,.T.);
#5606=ORIENTED_EDGE('',*,*,#3614,.T.);
#5607=ORIENTED_EDGE('',*,*,#3613,.T.);
#5608=ORIENTED_EDGE('',*,*,#3619,.T.);
#5609=ORIENTED_EDGE('',*,*,#3618,.T.);
#5610=ORIENTED_EDGE('',*,*,#3624,.T.);
#5611=ORIENTED_EDGE('',*,*,#3623,.T.);
#5612=ORIENTED_EDGE('',*,*,#3629,.T.);
#5613=ORIENTED_EDGE('',*,*,#3628,.T.);
#5614=ORIENTED_EDGE('',*,*,#3634,.T.);
#5615=ORIENTED_EDGE('',*,*,#3633,.T.);
#5616=ORIENTED_EDGE('',*,*,#3639,.T.);
#5617=ORIENTED_EDGE('',*,*,#3638,.T.);
#5618=ORIENTED_EDGE('',*,*,#3644,.T.);
#5619=ORIENTED_EDGE('',*,*,#3643,.T.);
#5620=ORIENTED_EDGE('',*,*,#3649,.T.);
#5621=ORIENTED_EDGE('',*,*,#3648,.T.);
#5622=ORIENTED_EDGE('',*,*,#3654,.T.);
#5623=ORIENTED_EDGE('',*,*,#3653,.T.);
#5624=ORIENTED_EDGE('',*,*,#3659,.T.);
#5625=ORIENTED_EDGE('',*,*,#3658,.T.);
#5626=ORIENTED_EDGE('',*,*,#3664,.T.);
#5627=ORIENTED_EDGE('',*,*,#3663,.T.);
#5628=ORIENTED_EDGE('',*,*,#3669,.T.);
#5629=ORIENTED_EDGE('',*,*,#3668,.T.);
#5630=ORIENTED_EDGE('',*,*,#3674,.T.);
#5631=ORIENTED_EDGE('',*,*,#3673,.T.);
#5632=ORIENTED_EDGE('',*,*,#3679,.T.);
#5633=ORIENTED_EDGE('',*,*,#3678,.T.);
#5634=ORIENTED_EDGE('',*,*,#3684,.T.);
#5635=ORIENTED_EDGE('',*,*,#3683,.T.);
#5636=ORIENTED_EDGE('',*,*,#3689,.T.);
#5637=ORIENTED_EDGE('',*,*,#3688,.T.);
#5638=ORIENTED_EDGE('',*,*,#3696,.T.);
#5639=ORIENTED_EDGE('',*,*,#3695,.T.);
#5640=ORIENTED_EDGE('',*,*,#3851,.F.);
#5641=ORIENTED_EDGE('',*,*,#3871,.F.);
#5642=ORIENTED_EDGE('',*,*,#3872,.T.);
#5643=ORIENTED_EDGE('',*,*,#3873,.T.);
#5644=ORIENTED_EDGE('',*,*,#3874,.F.);
#5645=ORIENTED_EDGE('',*,*,#3875,.F.);
#5646=ORIENTED_EDGE('',*,*,#3876,.T.);
#5647=ORIENTED_EDGE('',*,*,#3877,.T.);
#5648=ORIENTED_EDGE('',*,*,#3872,.F.);
#5649=ORIENTED_EDGE('',*,*,#3878,.F.);
#5650=ORIENTED_EDGE('',*,*,#3879,.T.);
#5651=ORIENTED_EDGE('',*,*,#3880,.T.);
#5652=ORIENTED_EDGE('',*,*,#3876,.F.);
#5653=ORIENTED_EDGE('',*,*,#3881,.F.);
#5654=ORIENTED_EDGE('',*,*,#3882,.T.);
#5655=ORIENTED_EDGE('',*,*,#3883,.T.);
#5656=ORIENTED_EDGE('',*,*,#3879,.F.);
#5657=ORIENTED_EDGE('',*,*,#3884,.F.);
#5658=ORIENTED_EDGE('',*,*,#3885,.T.);
#5659=ORIENTED_EDGE('',*,*,#3886,.T.);
#5660=ORIENTED_EDGE('',*,*,#3882,.F.);
#5661=ORIENTED_EDGE('',*,*,#3887,.F.);
#5662=ORIENTED_EDGE('',*,*,#3874,.T.);
#5663=ORIENTED_EDGE('',*,*,#3888,.T.);
#5664=ORIENTED_EDGE('',*,*,#3885,.F.);
#5665=ORIENTED_EDGE('',*,*,#3888,.F.);
#5666=ORIENTED_EDGE('',*,*,#3873,.F.);
#5667=ORIENTED_EDGE('',*,*,#3877,.F.);
#5668=ORIENTED_EDGE('',*,*,#3880,.F.);
#5669=ORIENTED_EDGE('',*,*,#3883,.F.);
#5670=ORIENTED_EDGE('',*,*,#3886,.F.);
#5671=ORIENTED_EDGE('',*,*,#3889,.T.);
#5672=ORIENTED_EDGE('',*,*,#3869,.T.);
#5673=ORIENTED_EDGE('',*,*,#3310,.T.);
#5674=ORIENTED_EDGE('',*,*,#3870,.T.);
#5675=ORIENTED_EDGE('',*,*,#3698,.F.);
#5676=ORIENTED_EDGE('',*,*,#3864,.T.);
#5677=ORIENTED_EDGE('',*,*,#3861,.T.);
#5678=ORIENTED_EDGE('',*,*,#3858,.T.);
#5679=ORIENTED_EDGE('',*,*,#3855,.T.);
#5680=ORIENTED_EDGE('',*,*,#3889,.F.);
#5681=ORIENTED_EDGE('',*,*,#3890,.T.);
#5682=ORIENTED_EDGE('',*,*,#3891,.T.);
#5683=ORIENTED_EDGE('',*,*,#3890,.F.);
#5684=ORIENTED_EDGE('',*,*,#3891,.F.);
#5685=ORIENTED_EDGE('',*,*,#3871,.T.);
#5686=ORIENTED_EDGE('',*,*,#3887,.T.);
#5687=ORIENTED_EDGE('',*,*,#3884,.T.);
#5688=ORIENTED_EDGE('',*,*,#3881,.T.);
#5689=ORIENTED_EDGE('',*,*,#3878,.T.);
#5690=ORIENTED_EDGE('',*,*,#3875,.T.);
#5691=ORIENTED_EDGE('',*,*,#3866,.T.);
#5692=ORIENTED_EDGE('',*,*,#3863,.T.);
#5693=ORIENTED_EDGE('',*,*,#3860,.T.);
#5694=ORIENTED_EDGE('',*,*,#3857,.T.);
#5695=ORIENTED_EDGE('',*,*,#3892,.F.);
#5696=ORIENTED_EDGE('',*,*,#3893,.F.);
#5697=ORIENTED_EDGE('',*,*,#3894,.F.);
#5698=ORIENTED_EDGE('',*,*,#3895,.F.);
#5699=ORIENTED_EDGE('',*,*,#3896,.F.);
#5700=ORIENTED_EDGE('',*,*,#3897,.F.);
#5701=ORIENTED_EDGE('',*,*,#3898,.F.);
#5702=ORIENTED_EDGE('',*,*,#3899,.F.);
#5703=ORIENTED_EDGE('',*,*,#3899,.T.);
#5704=ORIENTED_EDGE('',*,*,#3900,.F.);
#5705=ORIENTED_EDGE('',*,*,#3893,.T.);
#5706=ORIENTED_EDGE('',*,*,#3901,.F.);
#5707=ORIENTED_EDGE('',*,*,#3896,.T.);
#5708=ORIENTED_EDGE('',*,*,#3901,.T.);
#5709=ORIENTED_EDGE('',*,*,#3892,.T.);
#5710=ORIENTED_EDGE('',*,*,#3902,.F.);
#5711=ORIENTED_EDGE('',*,*,#3898,.T.);
#5712=ORIENTED_EDGE('',*,*,#3903,.F.);
#5713=ORIENTED_EDGE('',*,*,#3894,.T.);
#5714=ORIENTED_EDGE('',*,*,#3900,.T.);
#5715=ORIENTED_EDGE('',*,*,#3897,.T.);
#5716=ORIENTED_EDGE('',*,*,#3902,.T.);
#5717=ORIENTED_EDGE('',*,*,#3895,.T.);
#5718=ORIENTED_EDGE('',*,*,#3903,.T.);
#5719=ORIENTED_EDGE('',*,*,#3904,.T.);
#5720=ORIENTED_EDGE('',*,*,#3905,.T.);
#5721=ORIENTED_EDGE('',*,*,#3906,.F.);
#5722=ORIENTED_EDGE('',*,*,#3907,.F.);
#5723=ORIENTED_EDGE('',*,*,#3908,.T.);
#5724=ORIENTED_EDGE('',*,*,#3909,.T.);
#5725=ORIENTED_EDGE('',*,*,#3910,.T.);
#5726=ORIENTED_EDGE('',*,*,#3904,.F.);
#5727=ORIENTED_EDGE('',*,*,#3911,.F.);
#5728=ORIENTED_EDGE('',*,*,#3912,.F.);
#5729=ORIENTED_EDGE('',*,*,#3913,.T.);
#5730=ORIENTED_EDGE('',*,*,#3914,.T.);
#5731=ORIENTED_EDGE('',*,*,#3915,.T.);
#5732=ORIENTED_EDGE('',*,*,#3908,.F.);
#5733=ORIENTED_EDGE('',*,*,#3916,.F.);
#5734=ORIENTED_EDGE('',*,*,#3917,.F.);
#5735=ORIENTED_EDGE('',*,*,#3918,.T.);
#5736=ORIENTED_EDGE('',*,*,#3919,.T.);
#5737=ORIENTED_EDGE('',*,*,#3920,.T.);
#5738=ORIENTED_EDGE('',*,*,#3913,.F.);
#5739=ORIENTED_EDGE('',*,*,#3921,.F.);
#5740=ORIENTED_EDGE('',*,*,#3922,.F.);
#5741=ORIENTED_EDGE('',*,*,#3923,.T.);
#5742=ORIENTED_EDGE('',*,*,#3924,.T.);
#5743=ORIENTED_EDGE('',*,*,#3925,.T.);
#5744=ORIENTED_EDGE('',*,*,#3918,.F.);
#5745=ORIENTED_EDGE('',*,*,#3926,.F.);
#5746=ORIENTED_EDGE('',*,*,#3927,.F.);
#5747=ORIENTED_EDGE('',*,*,#3928,.T.);
#5748=ORIENTED_EDGE('',*,*,#3929,.T.);
#5749=ORIENTED_EDGE('',*,*,#3930,.T.);
#5750=ORIENTED_EDGE('',*,*,#3923,.F.);
#5751=ORIENTED_EDGE('',*,*,#3931,.F.);
#5752=ORIENTED_EDGE('',*,*,#3932,.F.);
#5753=ORIENTED_EDGE('',*,*,#3933,.T.);
#5754=ORIENTED_EDGE('',*,*,#3934,.T.);
#5755=ORIENTED_EDGE('',*,*,#3935,.T.);
#5756=ORIENTED_EDGE('',*,*,#3928,.F.);
#5757=ORIENTED_EDGE('',*,*,#3936,.F.);
#5758=ORIENTED_EDGE('',*,*,#3937,.F.);
#5759=ORIENTED_EDGE('',*,*,#3938,.T.);
#5760=ORIENTED_EDGE('',*,*,#3939,.T.);
#5761=ORIENTED_EDGE('',*,*,#3940,.T.);
#5762=ORIENTED_EDGE('',*,*,#3933,.F.);
#5763=ORIENTED_EDGE('',*,*,#3941,.F.);
#5764=ORIENTED_EDGE('',*,*,#3942,.F.);
#5765=ORIENTED_EDGE('',*,*,#3943,.T.);
#5766=ORIENTED_EDGE('',*,*,#3944,.T.);
#5767=ORIENTED_EDGE('',*,*,#3945,.T.);
#5768=ORIENTED_EDGE('',*,*,#3938,.F.);
#5769=ORIENTED_EDGE('',*,*,#3946,.F.);
#5770=ORIENTED_EDGE('',*,*,#3947,.F.);
#5771=ORIENTED_EDGE('',*,*,#3948,.F.);
#5772=ORIENTED_EDGE('',*,*,#3949,.F.);
#5773=ORIENTED_EDGE('',*,*,#3950,.F.);
#5774=ORIENTED_EDGE('',*,*,#3951,.F.);
#5775=ORIENTED_EDGE('',*,*,#3952,.T.);
#5776=ORIENTED_EDGE('',*,*,#3953,.T.);
#5777=ORIENTED_EDGE('',*,*,#3954,.T.);
#5778=ORIENTED_EDGE('',*,*,#3955,.T.);
#5779=ORIENTED_EDGE('',*,*,#3956,.F.);
#5780=ORIENTED_EDGE('',*,*,#3957,.T.);
#5781=ORIENTED_EDGE('',*,*,#3958,.T.);
#5782=ORIENTED_EDGE('',*,*,#3959,.T.);
#5783=ORIENTED_EDGE('',*,*,#3954,.F.);
#5784=ORIENTED_EDGE('',*,*,#3960,.T.);
#5785=ORIENTED_EDGE('',*,*,#3961,.T.);
#5786=ORIENTED_EDGE('',*,*,#3962,.T.);
#5787=ORIENTED_EDGE('',*,*,#3963,.T.);
#5788=ORIENTED_EDGE('',*,*,#3958,.F.);
#5789=ORIENTED_EDGE('',*,*,#3964,.T.);
#5790=ORIENTED_EDGE('',*,*,#3965,.T.);
#5791=ORIENTED_EDGE('',*,*,#3966,.T.);
#5792=ORIENTED_EDGE('',*,*,#3967,.T.);
#5793=ORIENTED_EDGE('',*,*,#3968,.T.);
#5794=ORIENTED_EDGE('',*,*,#3961,.F.);
#5795=ORIENTED_EDGE('',*,*,#3969,.T.);
#5796=ORIENTED_EDGE('',*,*,#3970,.T.);
#5797=ORIENTED_EDGE('',*,*,#3971,.T.);
#5798=ORIENTED_EDGE('',*,*,#3972,.T.);
#5799=ORIENTED_EDGE('',*,*,#3973,.T.);
#5800=ORIENTED_EDGE('',*,*,#3966,.F.);
#5801=ORIENTED_EDGE('',*,*,#3974,.T.);
#5802=ORIENTED_EDGE('',*,*,#3975,.T.);
#5803=ORIENTED_EDGE('',*,*,#3976,.T.);
#5804=ORIENTED_EDGE('',*,*,#3971,.F.);
#5805=ORIENTED_EDGE('',*,*,#3977,.T.);
#5806=ORIENTED_EDGE('',*,*,#3978,.T.);
#5807=ORIENTED_EDGE('',*,*,#3979,.T.);
#5808=ORIENTED_EDGE('',*,*,#3980,.T.);
#5809=ORIENTED_EDGE('',*,*,#3981,.T.);
#5810=ORIENTED_EDGE('',*,*,#3975,.F.);
#5811=ORIENTED_EDGE('',*,*,#3982,.T.);
#5812=ORIENTED_EDGE('',*,*,#3983,.T.);
#5813=ORIENTED_EDGE('',*,*,#3984,.T.);
#5814=ORIENTED_EDGE('',*,*,#3985,.T.);
#5815=ORIENTED_EDGE('',*,*,#3979,.F.);
#5816=ORIENTED_EDGE('',*,*,#3986,.T.);
#5817=ORIENTED_EDGE('',*,*,#3987,.T.);
#5818=ORIENTED_EDGE('',*,*,#3988,.T.);
#5819=ORIENTED_EDGE('',*,*,#3989,.T.);
#5820=ORIENTED_EDGE('',*,*,#3990,.T.);
#5821=ORIENTED_EDGE('',*,*,#3984,.F.);
#5822=ORIENTED_EDGE('',*,*,#3991,.T.);
#5823=ORIENTED_EDGE('',*,*,#3992,.T.);
#5824=ORIENTED_EDGE('',*,*,#3993,.F.);
#5825=ORIENTED_EDGE('',*,*,#3994,.T.);
#5826=ORIENTED_EDGE('',*,*,#3995,.F.);
#5827=ORIENTED_EDGE('',*,*,#3996,.T.);
#5828=ORIENTED_EDGE('',*,*,#3997,.T.);
#5829=ORIENTED_EDGE('',*,*,#3993,.T.);
#5830=ORIENTED_EDGE('',*,*,#3998,.T.);
#5831=ORIENTED_EDGE('',*,*,#3988,.F.);
#5832=ORIENTED_EDGE('',*,*,#3999,.T.);
#5833=ORIENTED_EDGE('',*,*,#4000,.T.);
#5834=ORIENTED_EDGE('',*,*,#3948,.T.);
#5835=ORIENTED_EDGE('',*,*,#4001,.T.);
#5836=ORIENTED_EDGE('',*,*,#4002,.T.);
#5837=ORIENTED_EDGE('',*,*,#3943,.F.);
#5838=ORIENTED_EDGE('',*,*,#4003,.F.);
#5839=ORIENTED_EDGE('',*,*,#4004,.F.);
#5840=ORIENTED_EDGE('',*,*,#4005,.F.);
#5841=ORIENTED_EDGE('',*,*,#4006,.T.);
#5842=ORIENTED_EDGE('',*,*,#4007,.F.);
#5843=ORIENTED_EDGE('',*,*,#4006,.F.);
#5844=ORIENTED_EDGE('',*,*,#4008,.F.);
#5845=ORIENTED_EDGE('',*,*,#4009,.T.);
#5846=ORIENTED_EDGE('',*,*,#4010,.F.);
#5847=ORIENTED_EDGE('',*,*,#4009,.F.);
#5848=ORIENTED_EDGE('',*,*,#4011,.F.);
#5849=ORIENTED_EDGE('',*,*,#3905,.F.);
#5850=ORIENTED_EDGE('',*,*,#3910,.F.);
#5851=ORIENTED_EDGE('',*,*,#3909,.F.);
#5852=ORIENTED_EDGE('',*,*,#3915,.F.);
#5853=ORIENTED_EDGE('',*,*,#3914,.F.);
#5854=ORIENTED_EDGE('',*,*,#3920,.F.);
#5855=ORIENTED_EDGE('',*,*,#3919,.F.);
#5856=ORIENTED_EDGE('',*,*,#3925,.F.);
#5857=ORIENTED_EDGE('',*,*,#3924,.F.);
#5858=ORIENTED_EDGE('',*,*,#3930,.F.);
#5859=ORIENTED_EDGE('',*,*,#3929,.F.);
#5860=ORIENTED_EDGE('',*,*,#3935,.F.);
#5861=ORIENTED_EDGE('',*,*,#3934,.F.);
#5862=ORIENTED_EDGE('',*,*,#3940,.F.);
#5863=ORIENTED_EDGE('',*,*,#3939,.F.);
#5864=ORIENTED_EDGE('',*,*,#3945,.F.);
#5865=ORIENTED_EDGE('',*,*,#3944,.F.);
#5866=ORIENTED_EDGE('',*,*,#4002,.F.);
#5867=ORIENTED_EDGE('',*,*,#4001,.F.);
#5868=ORIENTED_EDGE('',*,*,#3953,.F.);
#5869=ORIENTED_EDGE('',*,*,#3952,.F.);
#5870=ORIENTED_EDGE('',*,*,#4012,.F.);
#5871=ORIENTED_EDGE('',*,*,#3994,.F.);
#5872=ORIENTED_EDGE('',*,*,#4000,.F.);
#5873=ORIENTED_EDGE('',*,*,#3999,.F.);
#5874=ORIENTED_EDGE('',*,*,#3992,.F.);
#5875=ORIENTED_EDGE('',*,*,#3991,.F.);
#5876=ORIENTED_EDGE('',*,*,#3987,.F.);
#5877=ORIENTED_EDGE('',*,*,#3986,.F.);
#5878=ORIENTED_EDGE('',*,*,#3983,.F.);
#5879=ORIENTED_EDGE('',*,*,#3982,.F.);
#5880=ORIENTED_EDGE('',*,*,#3978,.F.);
#5881=ORIENTED_EDGE('',*,*,#3977,.F.);
#5882=ORIENTED_EDGE('',*,*,#3974,.F.);
#5883=ORIENTED_EDGE('',*,*,#3970,.F.);
#5884=ORIENTED_EDGE('',*,*,#3969,.F.);
#5885=ORIENTED_EDGE('',*,*,#3965,.F.);
#5886=ORIENTED_EDGE('',*,*,#3964,.F.);
#5887=ORIENTED_EDGE('',*,*,#3960,.F.);
#5888=ORIENTED_EDGE('',*,*,#3957,.F.);
#5889=ORIENTED_EDGE('',*,*,#4013,.F.);
#5890=ORIENTED_EDGE('',*,*,#4014,.F.);
#5891=ORIENTED_EDGE('',*,*,#3955,.F.);
#5892=ORIENTED_EDGE('',*,*,#3959,.F.);
#5893=ORIENTED_EDGE('',*,*,#3963,.F.);
#5894=ORIENTED_EDGE('',*,*,#3962,.F.);
#5895=ORIENTED_EDGE('',*,*,#3968,.F.);
#5896=ORIENTED_EDGE('',*,*,#3967,.F.);
#5897=ORIENTED_EDGE('',*,*,#3973,.F.);
#5898=ORIENTED_EDGE('',*,*,#3972,.F.);
#5899=ORIENTED_EDGE('',*,*,#3976,.F.);
#5900=ORIENTED_EDGE('',*,*,#3981,.F.);
#5901=ORIENTED_EDGE('',*,*,#3980,.F.);
#5902=ORIENTED_EDGE('',*,*,#3985,.F.);
#5903=ORIENTED_EDGE('',*,*,#3990,.F.);
#5904=ORIENTED_EDGE('',*,*,#3989,.F.);
#5905=ORIENTED_EDGE('',*,*,#3998,.F.);
#5906=ORIENTED_EDGE('',*,*,#3997,.F.);
#5907=ORIENTED_EDGE('',*,*,#3996,.F.);
#5908=ORIENTED_EDGE('',*,*,#4015,.F.);
#5909=ORIENTED_EDGE('',*,*,#3950,.T.);
#5910=ORIENTED_EDGE('',*,*,#3949,.T.);
#5911=ORIENTED_EDGE('',*,*,#4004,.T.);
#5912=ORIENTED_EDGE('',*,*,#4003,.T.);
#5913=ORIENTED_EDGE('',*,*,#3947,.T.);
#5914=ORIENTED_EDGE('',*,*,#3946,.T.);
#5915=ORIENTED_EDGE('',*,*,#3942,.T.);
#5916=ORIENTED_EDGE('',*,*,#3941,.T.);
#5917=ORIENTED_EDGE('',*,*,#3937,.T.);
#5918=ORIENTED_EDGE('',*,*,#3936,.T.);
#5919=ORIENTED_EDGE('',*,*,#3932,.T.);
#5920=ORIENTED_EDGE('',*,*,#3931,.T.);
#5921=ORIENTED_EDGE('',*,*,#3927,.T.);
#5922=ORIENTED_EDGE('',*,*,#3926,.T.);
#5923=ORIENTED_EDGE('',*,*,#3922,.T.);
#5924=ORIENTED_EDGE('',*,*,#3921,.T.);
#5925=ORIENTED_EDGE('',*,*,#3917,.T.);
#5926=ORIENTED_EDGE('',*,*,#3916,.T.);
#5927=ORIENTED_EDGE('',*,*,#3912,.T.);
#5928=ORIENTED_EDGE('',*,*,#3911,.T.);
#5929=ORIENTED_EDGE('',*,*,#3907,.T.);
#5930=ORIENTED_EDGE('',*,*,#4016,.T.);
#5931=ORIENTED_EDGE('',*,*,#4017,.T.);
#5932=ORIENTED_EDGE('',*,*,#4018,.T.);
#5933=ORIENTED_EDGE('',*,*,#4019,.T.);
#5934=ORIENTED_EDGE('',*,*,#4005,.T.);
#5935=ORIENTED_EDGE('',*,*,#4008,.T.);
#5936=ORIENTED_EDGE('',*,*,#4020,.T.);
#5937=ORIENTED_EDGE('',*,*,#4021,.T.);
#5938=ORIENTED_EDGE('',*,*,#4012,.T.);
#5939=ORIENTED_EDGE('',*,*,#3951,.T.);
#5940=ORIENTED_EDGE('',*,*,#4015,.T.);
#5941=ORIENTED_EDGE('',*,*,#3995,.T.);
#5942=ORIENTED_EDGE('',*,*,#4021,.F.);
#5943=ORIENTED_EDGE('',*,*,#4022,.T.);
#5944=ORIENTED_EDGE('',*,*,#4023,.F.);
#5945=ORIENTED_EDGE('',*,*,#4022,.F.);
#5946=ORIENTED_EDGE('',*,*,#4020,.F.);
#5947=ORIENTED_EDGE('',*,*,#4024,.T.);
#5948=ORIENTED_EDGE('',*,*,#4025,.F.);
#5949=ORIENTED_EDGE('',*,*,#4024,.F.);
#5950=ORIENTED_EDGE('',*,*,#4026,.T.);
#5951=ORIENTED_EDGE('',*,*,#4027,.T.);
#5952=ORIENTED_EDGE('',*,*,#4019,.F.);
#5953=ORIENTED_EDGE('',*,*,#4028,.F.);
#5954=ORIENTED_EDGE('',*,*,#4029,.T.);
#5955=ORIENTED_EDGE('',*,*,#4028,.T.);
#5956=ORIENTED_EDGE('',*,*,#4018,.F.);
#5957=ORIENTED_EDGE('',*,*,#4030,.F.);
#5958=ORIENTED_EDGE('',*,*,#4031,.T.);
#5959=ORIENTED_EDGE('',*,*,#4030,.T.);
#5960=ORIENTED_EDGE('',*,*,#4017,.F.);
#5961=ORIENTED_EDGE('',*,*,#4032,.F.);
#5962=ORIENTED_EDGE('',*,*,#4033,.T.);
#5963=ORIENTED_EDGE('',*,*,#4032,.T.);
#5964=ORIENTED_EDGE('',*,*,#4016,.F.);
#5965=ORIENTED_EDGE('',*,*,#4027,.F.);
#5966=ORIENTED_EDGE('',*,*,#4033,.F.);
#5967=ORIENTED_EDGE('',*,*,#4026,.F.);
#5968=ORIENTED_EDGE('',*,*,#4029,.F.);
#5969=ORIENTED_EDGE('',*,*,#4031,.F.);
#5970=ORIENTED_EDGE('',*,*,#4007,.T.);
#5971=ORIENTED_EDGE('',*,*,#4010,.T.);
#5972=ORIENTED_EDGE('',*,*,#4011,.T.);
#5973=ORIENTED_EDGE('',*,*,#4013,.T.);
#5974=ORIENTED_EDGE('',*,*,#3956,.T.);
#5975=ORIENTED_EDGE('',*,*,#4014,.T.);
#5976=ORIENTED_EDGE('',*,*,#3906,.T.);
#5977=ORIENTED_EDGE('',*,*,#4023,.T.);
#5978=ORIENTED_EDGE('',*,*,#4025,.T.);
#5979=ORIENTED_EDGE('',*,*,#4034,.T.);
#5980=ORIENTED_EDGE('',*,*,#4035,.T.);
#5981=ORIENTED_EDGE('',*,*,#4036,.F.);
#5982=ORIENTED_EDGE('',*,*,#4037,.F.);
#5983=ORIENTED_EDGE('',*,*,#4038,.T.);
#5984=ORIENTED_EDGE('',*,*,#4039,.T.);
#5985=ORIENTED_EDGE('',*,*,#4040,.T.);
#5986=ORIENTED_EDGE('',*,*,#4034,.F.);
#5987=ORIENTED_EDGE('',*,*,#4041,.F.);
#5988=ORIENTED_EDGE('',*,*,#4042,.F.);
#5989=ORIENTED_EDGE('',*,*,#4043,.T.);
#5990=ORIENTED_EDGE('',*,*,#4044,.T.);
#5991=ORIENTED_EDGE('',*,*,#4045,.T.);
#5992=ORIENTED_EDGE('',*,*,#4038,.F.);
#5993=ORIENTED_EDGE('',*,*,#4046,.F.);
#5994=ORIENTED_EDGE('',*,*,#4047,.F.);
#5995=ORIENTED_EDGE('',*,*,#4048,.T.);
#5996=ORIENTED_EDGE('',*,*,#4049,.T.);
#5997=ORIENTED_EDGE('',*,*,#4050,.T.);
#5998=ORIENTED_EDGE('',*,*,#4043,.F.);
#5999=ORIENTED_EDGE('',*,*,#4051,.F.);
#6000=ORIENTED_EDGE('',*,*,#4052,.F.);
#6001=ORIENTED_EDGE('',*,*,#4053,.T.);
#6002=ORIENTED_EDGE('',*,*,#4054,.T.);
#6003=ORIENTED_EDGE('',*,*,#4055,.T.);
#6004=ORIENTED_EDGE('',*,*,#4048,.F.);
#6005=ORIENTED_EDGE('',*,*,#4056,.F.);
#6006=ORIENTED_EDGE('',*,*,#4057,.F.);
#6007=ORIENTED_EDGE('',*,*,#4058,.F.);
#6008=ORIENTED_EDGE('',*,*,#4059,.F.);
#6009=ORIENTED_EDGE('',*,*,#4060,.F.);
#6010=ORIENTED_EDGE('',*,*,#4061,.F.);
#6011=ORIENTED_EDGE('',*,*,#4062,.T.);
#6012=ORIENTED_EDGE('',*,*,#4063,.T.);
#6013=ORIENTED_EDGE('',*,*,#4064,.T.);
#6014=ORIENTED_EDGE('',*,*,#4065,.T.);
#6015=ORIENTED_EDGE('',*,*,#4066,.F.);
#6016=ORIENTED_EDGE('',*,*,#4067,.F.);
#6017=ORIENTED_EDGE('',*,*,#4068,.T.);
#6018=ORIENTED_EDGE('',*,*,#4069,.T.);
#6019=ORIENTED_EDGE('',*,*,#4070,.T.);
#6020=ORIENTED_EDGE('',*,*,#4064,.F.);
#6021=ORIENTED_EDGE('',*,*,#4071,.F.);
#6022=ORIENTED_EDGE('',*,*,#4072,.F.);
#6023=ORIENTED_EDGE('',*,*,#4073,.T.);
#6024=ORIENTED_EDGE('',*,*,#4074,.T.);
#6025=ORIENTED_EDGE('',*,*,#4075,.T.);
#6026=ORIENTED_EDGE('',*,*,#4068,.F.);
#6027=ORIENTED_EDGE('',*,*,#4076,.F.);
#6028=ORIENTED_EDGE('',*,*,#4077,.F.);
#6029=ORIENTED_EDGE('',*,*,#4078,.T.);
#6030=ORIENTED_EDGE('',*,*,#4079,.T.);
#6031=ORIENTED_EDGE('',*,*,#4080,.T.);
#6032=ORIENTED_EDGE('',*,*,#4073,.F.);
#6033=ORIENTED_EDGE('',*,*,#4081,.F.);
#6034=ORIENTED_EDGE('',*,*,#4082,.F.);
#6035=ORIENTED_EDGE('',*,*,#4083,.T.);
#6036=ORIENTED_EDGE('',*,*,#4084,.T.);
#6037=ORIENTED_EDGE('',*,*,#4085,.T.);
#6038=ORIENTED_EDGE('',*,*,#4078,.F.);
#6039=ORIENTED_EDGE('',*,*,#4086,.F.);
#6040=ORIENTED_EDGE('',*,*,#4087,.F.);
#6041=ORIENTED_EDGE('',*,*,#4088,.F.);
#6042=ORIENTED_EDGE('',*,*,#4089,.F.);
#6043=ORIENTED_EDGE('',*,*,#4090,.F.);
#6044=ORIENTED_EDGE('',*,*,#4091,.F.);
#6045=ORIENTED_EDGE('',*,*,#4092,.T.);
#6046=ORIENTED_EDGE('',*,*,#4093,.T.);
#6047=ORIENTED_EDGE('',*,*,#4094,.T.);
#6048=ORIENTED_EDGE('',*,*,#4095,.T.);
#6049=ORIENTED_EDGE('',*,*,#4096,.F.);
#6050=ORIENTED_EDGE('',*,*,#4097,.T.);
#6051=ORIENTED_EDGE('',*,*,#4098,.T.);
#6052=ORIENTED_EDGE('',*,*,#4099,.T.);
#6053=ORIENTED_EDGE('',*,*,#4100,.T.);
#6054=ORIENTED_EDGE('',*,*,#4094,.F.);
#6055=ORIENTED_EDGE('',*,*,#4101,.T.);
#6056=ORIENTED_EDGE('',*,*,#4102,.T.);
#6057=ORIENTED_EDGE('',*,*,#4103,.T.);
#6058=ORIENTED_EDGE('',*,*,#4104,.T.);
#6059=ORIENTED_EDGE('',*,*,#4098,.F.);
#6060=ORIENTED_EDGE('',*,*,#4105,.T.);
#6061=ORIENTED_EDGE('',*,*,#4106,.T.);
#6062=ORIENTED_EDGE('',*,*,#4107,.T.);
#6063=ORIENTED_EDGE('',*,*,#4108,.T.);
#6064=ORIENTED_EDGE('',*,*,#4109,.T.);
#6065=ORIENTED_EDGE('',*,*,#4102,.F.);
#6066=ORIENTED_EDGE('',*,*,#4110,.T.);
#6067=ORIENTED_EDGE('',*,*,#4111,.T.);
#6068=ORIENTED_EDGE('',*,*,#4112,.T.);
#6069=ORIENTED_EDGE('',*,*,#4113,.T.);
#6070=ORIENTED_EDGE('',*,*,#4107,.F.);
#6071=ORIENTED_EDGE('',*,*,#4114,.T.);
#6072=ORIENTED_EDGE('',*,*,#4115,.T.);
#6073=ORIENTED_EDGE('',*,*,#4116,.F.);
#6074=ORIENTED_EDGE('',*,*,#4117,.T.);
#6075=ORIENTED_EDGE('',*,*,#4118,.T.);
#6076=ORIENTED_EDGE('',*,*,#4119,.F.);
#6077=ORIENTED_EDGE('',*,*,#4120,.T.);
#6078=ORIENTED_EDGE('',*,*,#4121,.T.);
#6079=ORIENTED_EDGE('',*,*,#4122,.T.);
#6080=ORIENTED_EDGE('',*,*,#4123,.T.);
#6081=ORIENTED_EDGE('',*,*,#4124,.F.);
#6082=ORIENTED_EDGE('',*,*,#4125,.T.);
#6083=ORIENTED_EDGE('',*,*,#4126,.T.);
#6084=ORIENTED_EDGE('',*,*,#4127,.T.);
#6085=ORIENTED_EDGE('',*,*,#4128,.T.);
#6086=ORIENTED_EDGE('',*,*,#4122,.F.);
#6087=ORIENTED_EDGE('',*,*,#4129,.T.);
#6088=ORIENTED_EDGE('',*,*,#4130,.T.);
#6089=ORIENTED_EDGE('',*,*,#4131,.T.);
#6090=ORIENTED_EDGE('',*,*,#4132,.T.);
#6091=ORIENTED_EDGE('',*,*,#4126,.F.);
#6092=ORIENTED_EDGE('',*,*,#4133,.T.);
#6093=ORIENTED_EDGE('',*,*,#4134,.T.);
#6094=ORIENTED_EDGE('',*,*,#4135,.T.);
#6095=ORIENTED_EDGE('',*,*,#4136,.T.);
#6096=ORIENTED_EDGE('',*,*,#4137,.T.);
#6097=ORIENTED_EDGE('',*,*,#4130,.F.);
#6098=ORIENTED_EDGE('',*,*,#4138,.T.);
#6099=ORIENTED_EDGE('',*,*,#4139,.T.);
#6100=ORIENTED_EDGE('',*,*,#4140,.T.);
#6101=ORIENTED_EDGE('',*,*,#4141,.T.);
#6102=ORIENTED_EDGE('',*,*,#4135,.F.);
#6103=ORIENTED_EDGE('',*,*,#4142,.T.);
#6104=ORIENTED_EDGE('',*,*,#4143,.T.);
#6105=ORIENTED_EDGE('',*,*,#4144,.F.);
#6106=ORIENTED_EDGE('',*,*,#4145,.T.);
#6107=ORIENTED_EDGE('',*,*,#4146,.T.);
#6108=ORIENTED_EDGE('',*,*,#4147,.F.);
#6109=ORIENTED_EDGE('',*,*,#4148,.T.);
#6110=ORIENTED_EDGE('',*,*,#4149,.T.);
#6111=ORIENTED_EDGE('',*,*,#4144,.T.);
#6112=ORIENTED_EDGE('',*,*,#4150,.T.);
#6113=ORIENTED_EDGE('',*,*,#4151,.T.);
#6114=ORIENTED_EDGE('',*,*,#4139,.F.);
#6115=ORIENTED_EDGE('',*,*,#4152,.T.);
#6116=ORIENTED_EDGE('',*,*,#4153,.T.);
#6117=ORIENTED_EDGE('',*,*,#4116,.T.);
#6118=ORIENTED_EDGE('',*,*,#4154,.T.);
#6119=ORIENTED_EDGE('',*,*,#4155,.T.);
#6120=ORIENTED_EDGE('',*,*,#4111,.F.);
#6121=ORIENTED_EDGE('',*,*,#4156,.T.);
#6122=ORIENTED_EDGE('',*,*,#4157,.T.);
#6123=ORIENTED_EDGE('',*,*,#4088,.T.);
#6124=ORIENTED_EDGE('',*,*,#4158,.T.);
#6125=ORIENTED_EDGE('',*,*,#4159,.T.);
#6126=ORIENTED_EDGE('',*,*,#4083,.F.);
#6127=ORIENTED_EDGE('',*,*,#4160,.F.);
#6128=ORIENTED_EDGE('',*,*,#4161,.F.);
#6129=ORIENTED_EDGE('',*,*,#4058,.T.);
#6130=ORIENTED_EDGE('',*,*,#4162,.T.);
#6131=ORIENTED_EDGE('',*,*,#4163,.T.);
#6132=ORIENTED_EDGE('',*,*,#4053,.F.);
#6133=ORIENTED_EDGE('',*,*,#4164,.F.);
#6134=ORIENTED_EDGE('',*,*,#4165,.F.);
#6135=ORIENTED_EDGE('',*,*,#4166,.F.);
#6136=ORIENTED_EDGE('',*,*,#4035,.F.);
#6137=ORIENTED_EDGE('',*,*,#4040,.F.);
#6138=ORIENTED_EDGE('',*,*,#4039,.F.);
#6139=ORIENTED_EDGE('',*,*,#4045,.F.);
#6140=ORIENTED_EDGE('',*,*,#4044,.F.);
#6141=ORIENTED_EDGE('',*,*,#4050,.F.);
#6142=ORIENTED_EDGE('',*,*,#4049,.F.);
#6143=ORIENTED_EDGE('',*,*,#4055,.F.);
#6144=ORIENTED_EDGE('',*,*,#4054,.F.);
#6145=ORIENTED_EDGE('',*,*,#4163,.F.);
#6146=ORIENTED_EDGE('',*,*,#4162,.F.);
#6147=ORIENTED_EDGE('',*,*,#4063,.F.);
#6148=ORIENTED_EDGE('',*,*,#4062,.F.);
#6149=ORIENTED_EDGE('',*,*,#4167,.F.);
#6150=ORIENTED_EDGE('',*,*,#4146,.F.);
#6151=ORIENTED_EDGE('',*,*,#4145,.F.);
#6152=ORIENTED_EDGE('',*,*,#4153,.F.);
#6153=ORIENTED_EDGE('',*,*,#4152,.F.);
#6154=ORIENTED_EDGE('',*,*,#4143,.F.);
#6155=ORIENTED_EDGE('',*,*,#4142,.F.);
#6156=ORIENTED_EDGE('',*,*,#4138,.F.);
#6157=ORIENTED_EDGE('',*,*,#4134,.F.);
#6158=ORIENTED_EDGE('',*,*,#4133,.F.);
#6159=ORIENTED_EDGE('',*,*,#4129,.F.);
#6160=ORIENTED_EDGE('',*,*,#4125,.F.);
#6161=ORIENTED_EDGE('',*,*,#4168,.F.);
#6162=ORIENTED_EDGE('',*,*,#4169,.F.);
#6163=ORIENTED_EDGE('',*,*,#4123,.F.);
#6164=ORIENTED_EDGE('',*,*,#4128,.F.);
#6165=ORIENTED_EDGE('',*,*,#4127,.F.);
#6166=ORIENTED_EDGE('',*,*,#4132,.F.);
#6167=ORIENTED_EDGE('',*,*,#4131,.F.);
#6168=ORIENTED_EDGE('',*,*,#4137,.F.);
#6169=ORIENTED_EDGE('',*,*,#4136,.F.);
#6170=ORIENTED_EDGE('',*,*,#4141,.F.);
#6171=ORIENTED_EDGE('',*,*,#4140,.F.);
#6172=ORIENTED_EDGE('',*,*,#4151,.F.);
#6173=ORIENTED_EDGE('',*,*,#4150,.F.);
#6174=ORIENTED_EDGE('',*,*,#4149,.F.);
#6175=ORIENTED_EDGE('',*,*,#4148,.F.);
#6176=ORIENTED_EDGE('',*,*,#4170,.F.);
#6177=ORIENTED_EDGE('',*,*,#4060,.T.);
#6178=ORIENTED_EDGE('',*,*,#4059,.T.);
#6179=ORIENTED_EDGE('',*,*,#4165,.T.);
#6180=ORIENTED_EDGE('',*,*,#4164,.T.);
#6181=ORIENTED_EDGE('',*,*,#4057,.T.);
#6182=ORIENTED_EDGE('',*,*,#4056,.T.);
#6183=ORIENTED_EDGE('',*,*,#4052,.T.);
#6184=ORIENTED_EDGE('',*,*,#4051,.T.);
#6185=ORIENTED_EDGE('',*,*,#4047,.T.);
#6186=ORIENTED_EDGE('',*,*,#4046,.T.);
#6187=ORIENTED_EDGE('',*,*,#4042,.T.);
#6188=ORIENTED_EDGE('',*,*,#4041,.T.);
#6189=ORIENTED_EDGE('',*,*,#4037,.T.);
#6190=ORIENTED_EDGE('',*,*,#4171,.T.);
#6191=ORIENTED_EDGE('',*,*,#4172,.T.);
#6192=ORIENTED_EDGE('',*,*,#4173,.T.);
#6193=ORIENTED_EDGE('',*,*,#4174,.T.);
#6194=ORIENTED_EDGE('',*,*,#4175,.T.);
#6195=ORIENTED_EDGE('',*,*,#4091,.T.);
#6196=ORIENTED_EDGE('',*,*,#4176,.T.);
#6197=ORIENTED_EDGE('',*,*,#4119,.T.);
#6198=ORIENTED_EDGE('',*,*,#4167,.T.);
#6199=ORIENTED_EDGE('',*,*,#4061,.T.);
#6200=ORIENTED_EDGE('',*,*,#4170,.T.);
#6201=ORIENTED_EDGE('',*,*,#4147,.T.);
#6202=ORIENTED_EDGE('',*,*,#4177,.T.);
#6203=ORIENTED_EDGE('',*,*,#4178,.F.);
#6204=ORIENTED_EDGE('',*,*,#4065,.F.);
#6205=ORIENTED_EDGE('',*,*,#4070,.F.);
#6206=ORIENTED_EDGE('',*,*,#4069,.F.);
#6207=ORIENTED_EDGE('',*,*,#4075,.F.);
#6208=ORIENTED_EDGE('',*,*,#4074,.F.);
#6209=ORIENTED_EDGE('',*,*,#4080,.F.);
#6210=ORIENTED_EDGE('',*,*,#4079,.F.);
#6211=ORIENTED_EDGE('',*,*,#4085,.F.);
#6212=ORIENTED_EDGE('',*,*,#4084,.F.);
#6213=ORIENTED_EDGE('',*,*,#4159,.F.);
#6214=ORIENTED_EDGE('',*,*,#4158,.F.);
#6215=ORIENTED_EDGE('',*,*,#4093,.F.);
#6216=ORIENTED_EDGE('',*,*,#4092,.F.);
#6217=ORIENTED_EDGE('',*,*,#4175,.F.);
#6218=ORIENTED_EDGE('',*,*,#4118,.F.);
#6219=ORIENTED_EDGE('',*,*,#4117,.F.);
#6220=ORIENTED_EDGE('',*,*,#4157,.F.);
#6221=ORIENTED_EDGE('',*,*,#4156,.F.);
#6222=ORIENTED_EDGE('',*,*,#4115,.F.);
#6223=ORIENTED_EDGE('',*,*,#4114,.F.);
#6224=ORIENTED_EDGE('',*,*,#4110,.F.);
#6225=ORIENTED_EDGE('',*,*,#4106,.F.);
#6226=ORIENTED_EDGE('',*,*,#4105,.F.);
#6227=ORIENTED_EDGE('',*,*,#4101,.F.);
#6228=ORIENTED_EDGE('',*,*,#4097,.F.);
#6229=ORIENTED_EDGE('',*,*,#4179,.F.);
#6230=ORIENTED_EDGE('',*,*,#4180,.F.);
#6231=ORIENTED_EDGE('',*,*,#4095,.F.);
#6232=ORIENTED_EDGE('',*,*,#4100,.F.);
#6233=ORIENTED_EDGE('',*,*,#4099,.F.);
#6234=ORIENTED_EDGE('',*,*,#4104,.F.);
#6235=ORIENTED_EDGE('',*,*,#4103,.F.);
#6236=ORIENTED_EDGE('',*,*,#4109,.F.);
#6237=ORIENTED_EDGE('',*,*,#4108,.F.);
#6238=ORIENTED_EDGE('',*,*,#4113,.F.);
#6239=ORIENTED_EDGE('',*,*,#4112,.F.);
#6240=ORIENTED_EDGE('',*,*,#4155,.F.);
#6241=ORIENTED_EDGE('',*,*,#4154,.F.);
#6242=ORIENTED_EDGE('',*,*,#4121,.F.);
#6243=ORIENTED_EDGE('',*,*,#4120,.F.);
#6244=ORIENTED_EDGE('',*,*,#4176,.F.);
#6245=ORIENTED_EDGE('',*,*,#4090,.T.);
#6246=ORIENTED_EDGE('',*,*,#4089,.T.);
#6247=ORIENTED_EDGE('',*,*,#4161,.T.);
#6248=ORIENTED_EDGE('',*,*,#4160,.T.);
#6249=ORIENTED_EDGE('',*,*,#4087,.T.);
#6250=ORIENTED_EDGE('',*,*,#4086,.T.);
#6251=ORIENTED_EDGE('',*,*,#4082,.T.);
#6252=ORIENTED_EDGE('',*,*,#4081,.T.);
#6253=ORIENTED_EDGE('',*,*,#4077,.T.);
#6254=ORIENTED_EDGE('',*,*,#4076,.T.);
#6255=ORIENTED_EDGE('',*,*,#4072,.T.);
#6256=ORIENTED_EDGE('',*,*,#4071,.T.);
#6257=ORIENTED_EDGE('',*,*,#4067,.T.);
#6258=ORIENTED_EDGE('',*,*,#4177,.F.);
#6259=ORIENTED_EDGE('',*,*,#4181,.T.);
#6260=ORIENTED_EDGE('',*,*,#4182,.F.);
#6261=ORIENTED_EDGE('',*,*,#4181,.F.);
#6262=ORIENTED_EDGE('',*,*,#4183,.T.);
#6263=ORIENTED_EDGE('',*,*,#4184,.T.);
#6264=ORIENTED_EDGE('',*,*,#4174,.F.);
#6265=ORIENTED_EDGE('',*,*,#4185,.F.);
#6266=ORIENTED_EDGE('',*,*,#4186,.T.);
#6267=ORIENTED_EDGE('',*,*,#4185,.T.);
#6268=ORIENTED_EDGE('',*,*,#4173,.F.);
#6269=ORIENTED_EDGE('',*,*,#4187,.F.);
#6270=ORIENTED_EDGE('',*,*,#4188,.T.);
#6271=ORIENTED_EDGE('',*,*,#4187,.T.);
#6272=ORIENTED_EDGE('',*,*,#4172,.F.);
#6273=ORIENTED_EDGE('',*,*,#4189,.F.);
#6274=ORIENTED_EDGE('',*,*,#4190,.T.);
#6275=ORIENTED_EDGE('',*,*,#4189,.T.);
#6276=ORIENTED_EDGE('',*,*,#4171,.F.);
#6277=ORIENTED_EDGE('',*,*,#4184,.F.);
#6278=ORIENTED_EDGE('',*,*,#4190,.F.);
#6279=ORIENTED_EDGE('',*,*,#4183,.F.);
#6280=ORIENTED_EDGE('',*,*,#4186,.F.);
#6281=ORIENTED_EDGE('',*,*,#4188,.F.);
#6282=ORIENTED_EDGE('',*,*,#4166,.T.);
#6283=ORIENTED_EDGE('',*,*,#4168,.T.);
#6284=ORIENTED_EDGE('',*,*,#4124,.T.);
#6285=ORIENTED_EDGE('',*,*,#4169,.T.);
#6286=ORIENTED_EDGE('',*,*,#4036,.T.);
#6287=ORIENTED_EDGE('',*,*,#4178,.T.);
#6288=ORIENTED_EDGE('',*,*,#4179,.T.);
#6289=ORIENTED_EDGE('',*,*,#4096,.T.);
#6290=ORIENTED_EDGE('',*,*,#4180,.T.);
#6291=ORIENTED_EDGE('',*,*,#4066,.T.);
#6292=ORIENTED_EDGE('',*,*,#4182,.T.);
#6293=ORIENTED_EDGE('',*,*,#4191,.F.);
#6294=ORIENTED_EDGE('',*,*,#4192,.T.);
#6295=ORIENTED_EDGE('',*,*,#4193,.T.);
#6296=ORIENTED_EDGE('',*,*,#4192,.F.);
#6297=ORIENTED_EDGE('',*,*,#4194,.F.);
#6298=ORIENTED_EDGE('',*,*,#4193,.F.);
#6299=ORIENTED_EDGE('',*,*,#4195,.F.);
#6300=ORIENTED_EDGE('',*,*,#4191,.T.);
#6301=ORIENTED_EDGE('',*,*,#4196,.F.);
#6302=ORIENTED_EDGE('',*,*,#4197,.T.);
#6303=ORIENTED_EDGE('',*,*,#4195,.T.);
#6304=ORIENTED_EDGE('',*,*,#4197,.F.);
#6305=ORIENTED_EDGE('',*,*,#4198,.T.);
#6306=ORIENTED_EDGE('',*,*,#4199,.F.);
#6307=ORIENTED_EDGE('',*,*,#4198,.F.);
#6308=ORIENTED_EDGE('',*,*,#4200,.T.);
#6309=ORIENTED_EDGE('',*,*,#4201,.T.);
#6310=ORIENTED_EDGE('',*,*,#4200,.F.);
#6311=ORIENTED_EDGE('',*,*,#4201,.F.);
#6312=ORIENTED_EDGE('',*,*,#4194,.T.);
#6313=ORIENTED_EDGE('',*,*,#4202,.T.);
#6314=ORIENTED_EDGE('',*,*,#4199,.T.);
#6315=ORIENTED_EDGE('',*,*,#4202,.F.);
#6316=ORIENTED_EDGE('',*,*,#4196,.T.);
#6317=ORIENTED_EDGE('',*,*,#4203,.F.);
#6318=ORIENTED_EDGE('',*,*,#4204,.F.);
#6319=ORIENTED_EDGE('',*,*,#4205,.F.);
#6320=ORIENTED_EDGE('',*,*,#4206,.F.);
#6321=ORIENTED_EDGE('',*,*,#4207,.F.);
#6322=ORIENTED_EDGE('',*,*,#4208,.F.);
#6323=ORIENTED_EDGE('',*,*,#4209,.F.);
#6324=ORIENTED_EDGE('',*,*,#4210,.F.);
#6325=ORIENTED_EDGE('',*,*,#4210,.T.);
#6326=ORIENTED_EDGE('',*,*,#4211,.F.);
#6327=ORIENTED_EDGE('',*,*,#4204,.T.);
#6328=ORIENTED_EDGE('',*,*,#4212,.F.);
#6329=ORIENTED_EDGE('',*,*,#4207,.T.);
#6330=ORIENTED_EDGE('',*,*,#4212,.T.);
#6331=ORIENTED_EDGE('',*,*,#4203,.T.);
#6332=ORIENTED_EDGE('',*,*,#4213,.F.);
#6333=ORIENTED_EDGE('',*,*,#4209,.T.);
#6334=ORIENTED_EDGE('',*,*,#4214,.F.);
#6335=ORIENTED_EDGE('',*,*,#4205,.T.);
#6336=ORIENTED_EDGE('',*,*,#4211,.T.);
#6337=ORIENTED_EDGE('',*,*,#4208,.T.);
#6338=ORIENTED_EDGE('',*,*,#4213,.T.);
#6339=ORIENTED_EDGE('',*,*,#4206,.T.);
#6340=ORIENTED_EDGE('',*,*,#4214,.T.);
#6341=ORIENTED_EDGE('',*,*,#4215,.T.);
#6342=ORIENTED_EDGE('',*,*,#4216,.T.);
#6343=ORIENTED_EDGE('',*,*,#4217,.F.);
#6344=ORIENTED_EDGE('',*,*,#4216,.F.);
#6345=ORIENTED_EDGE('',*,*,#4218,.F.);
#6346=ORIENTED_EDGE('',*,*,#4219,.T.);
#6347=ORIENTED_EDGE('',*,*,#4220,.T.);
#6348=ORIENTED_EDGE('',*,*,#4219,.F.);
#6349=ORIENTED_EDGE('',*,*,#4218,.T.);
#6350=ORIENTED_EDGE('',*,*,#4217,.T.);
#6351=ORIENTED_EDGE('',*,*,#4220,.F.);
#6352=ORIENTED_EDGE('',*,*,#4215,.F.);
#6353=ORIENTED_EDGE('',*,*,#4221,.T.);
#6354=ORIENTED_EDGE('',*,*,#4222,.T.);
#6355=ORIENTED_EDGE('',*,*,#4223,.F.);
#6356=ORIENTED_EDGE('',*,*,#4222,.F.);
#6357=ORIENTED_EDGE('',*,*,#4224,.F.);
#6358=ORIENTED_EDGE('',*,*,#4225,.T.);
#6359=ORIENTED_EDGE('',*,*,#4226,.T.);
#6360=ORIENTED_EDGE('',*,*,#4225,.F.);
#6361=ORIENTED_EDGE('',*,*,#4224,.T.);
#6362=ORIENTED_EDGE('',*,*,#4223,.T.);
#6363=ORIENTED_EDGE('',*,*,#4226,.F.);
#6364=ORIENTED_EDGE('',*,*,#4221,.F.);
#6365=ORIENTED_EDGE('',*,*,#4227,.F.);
#6366=ORIENTED_EDGE('',*,*,#4228,.F.);
#6367=ORIENTED_EDGE('',*,*,#4229,.F.);
#6368=ORIENTED_EDGE('',*,*,#4230,.T.);
#6369=ORIENTED_EDGE('',*,*,#4231,.F.);
#6370=ORIENTED_EDGE('',*,*,#4232,.F.);
#6371=ORIENTED_EDGE('',*,*,#4227,.T.);
#6372=ORIENTED_EDGE('',*,*,#4233,.T.);
#6373=ORIENTED_EDGE('',*,*,#4234,.T.);
#6374=ORIENTED_EDGE('',*,*,#4235,.F.);
#6375=ORIENTED_EDGE('',*,*,#4236,.F.);
#6376=ORIENTED_EDGE('',*,*,#4237,.F.);
#6377=ORIENTED_EDGE('',*,*,#4231,.T.);
#6378=ORIENTED_EDGE('',*,*,#4238,.T.);
#6379=ORIENTED_EDGE('',*,*,#4239,.F.);
#6380=ORIENTED_EDGE('',*,*,#4240,.F.);
#6381=ORIENTED_EDGE('',*,*,#4235,.T.);
#6382=ORIENTED_EDGE('',*,*,#4241,.T.);
#6383=ORIENTED_EDGE('',*,*,#4242,.T.);
#6384=ORIENTED_EDGE('',*,*,#4243,.F.);
#6385=ORIENTED_EDGE('',*,*,#4244,.F.);
#6386=ORIENTED_EDGE('',*,*,#4245,.F.);
#6387=ORIENTED_EDGE('',*,*,#4239,.T.);
#6388=ORIENTED_EDGE('',*,*,#4246,.T.);
#6389=ORIENTED_EDGE('',*,*,#4247,.T.);
#6390=ORIENTED_EDGE('',*,*,#4248,.F.);
#6391=ORIENTED_EDGE('',*,*,#4249,.F.);
#6392=ORIENTED_EDGE('',*,*,#4250,.F.);
#6393=ORIENTED_EDGE('',*,*,#4243,.T.);
#6394=ORIENTED_EDGE('',*,*,#4251,.T.);
#6395=ORIENTED_EDGE('',*,*,#4252,.F.);
#6396=ORIENTED_EDGE('',*,*,#4253,.F.);
#6397=ORIENTED_EDGE('',*,*,#4254,.F.);
#6398=ORIENTED_EDGE('',*,*,#4248,.T.);
#6399=ORIENTED_EDGE('',*,*,#4255,.T.);
#6400=ORIENTED_EDGE('',*,*,#4256,.T.);
#6401=ORIENTED_EDGE('',*,*,#4257,.F.);
#6402=ORIENTED_EDGE('',*,*,#4258,.F.);
#6403=ORIENTED_EDGE('',*,*,#4252,.T.);
#6404=ORIENTED_EDGE('',*,*,#4259,.T.);
#6405=ORIENTED_EDGE('',*,*,#4260,.F.);
#6406=ORIENTED_EDGE('',*,*,#4261,.F.);
#6407=ORIENTED_EDGE('',*,*,#4262,.F.);
#6408=ORIENTED_EDGE('',*,*,#4257,.T.);
#6409=ORIENTED_EDGE('',*,*,#4263,.T.);
#6410=ORIENTED_EDGE('',*,*,#4264,.T.);
#6411=ORIENTED_EDGE('',*,*,#4265,.F.);
#6412=ORIENTED_EDGE('',*,*,#4266,.F.);
#6413=ORIENTED_EDGE('',*,*,#4260,.T.);
#6414=ORIENTED_EDGE('',*,*,#4267,.T.);
#6415=ORIENTED_EDGE('',*,*,#4268,.F.);
#6416=ORIENTED_EDGE('',*,*,#4269,.F.);
#6417=ORIENTED_EDGE('',*,*,#4270,.F.);
#6418=ORIENTED_EDGE('',*,*,#4265,.T.);
#6419=ORIENTED_EDGE('',*,*,#4271,.T.);
#6420=ORIENTED_EDGE('',*,*,#4272,.T.);
#6421=ORIENTED_EDGE('',*,*,#4273,.F.);
#6422=ORIENTED_EDGE('',*,*,#4274,.F.);
#6423=ORIENTED_EDGE('',*,*,#4275,.F.);
#6424=ORIENTED_EDGE('',*,*,#4268,.T.);
#6425=ORIENTED_EDGE('',*,*,#4276,.T.);
#6426=ORIENTED_EDGE('',*,*,#4277,.T.);
#6427=ORIENTED_EDGE('',*,*,#4278,.F.);
#6428=ORIENTED_EDGE('',*,*,#4279,.F.);
#6429=ORIENTED_EDGE('',*,*,#4280,.F.);
#6430=ORIENTED_EDGE('',*,*,#4273,.T.);
#6431=ORIENTED_EDGE('',*,*,#4281,.T.);
#6432=ORIENTED_EDGE('',*,*,#4282,.F.);
#6433=ORIENTED_EDGE('',*,*,#4283,.F.);
#6434=ORIENTED_EDGE('',*,*,#4278,.T.);
#6435=ORIENTED_EDGE('',*,*,#4284,.T.);
#6436=ORIENTED_EDGE('',*,*,#4285,.T.);
#6437=ORIENTED_EDGE('',*,*,#4286,.F.);
#6438=ORIENTED_EDGE('',*,*,#4287,.F.);
#6439=ORIENTED_EDGE('',*,*,#4288,.F.);
#6440=ORIENTED_EDGE('',*,*,#4282,.T.);
#6441=ORIENTED_EDGE('',*,*,#4289,.T.);
#6442=ORIENTED_EDGE('',*,*,#4290,.F.);
#6443=ORIENTED_EDGE('',*,*,#4291,.F.);
#6444=ORIENTED_EDGE('',*,*,#4286,.T.);
#6445=ORIENTED_EDGE('',*,*,#4292,.T.);
#6446=ORIENTED_EDGE('',*,*,#4293,.T.);
#6447=ORIENTED_EDGE('',*,*,#4294,.F.);
#6448=ORIENTED_EDGE('',*,*,#4295,.F.);
#6449=ORIENTED_EDGE('',*,*,#4296,.F.);
#6450=ORIENTED_EDGE('',*,*,#4290,.T.);
#6451=ORIENTED_EDGE('',*,*,#4297,.T.);
#6452=ORIENTED_EDGE('',*,*,#4298,.F.);
#6453=ORIENTED_EDGE('',*,*,#4299,.F.);
#6454=ORIENTED_EDGE('',*,*,#4294,.T.);
#6455=ORIENTED_EDGE('',*,*,#4300,.T.);
#6456=ORIENTED_EDGE('',*,*,#4301,.T.);
#6457=ORIENTED_EDGE('',*,*,#4302,.F.);
#6458=ORIENTED_EDGE('',*,*,#4303,.F.);
#6459=ORIENTED_EDGE('',*,*,#4304,.F.);
#6460=ORIENTED_EDGE('',*,*,#4298,.T.);
#6461=ORIENTED_EDGE('',*,*,#4305,.T.);
#6462=ORIENTED_EDGE('',*,*,#4306,.T.);
#6463=ORIENTED_EDGE('',*,*,#4307,.F.);
#6464=ORIENTED_EDGE('',*,*,#4308,.F.);
#6465=ORIENTED_EDGE('',*,*,#4302,.T.);
#6466=ORIENTED_EDGE('',*,*,#4309,.T.);
#6467=ORIENTED_EDGE('',*,*,#4310,.F.);
#6468=ORIENTED_EDGE('',*,*,#4311,.F.);
#6469=ORIENTED_EDGE('',*,*,#4312,.F.);
#6470=ORIENTED_EDGE('',*,*,#4307,.T.);
#6471=ORIENTED_EDGE('',*,*,#4313,.T.);
#6472=ORIENTED_EDGE('',*,*,#4314,.T.);
#6473=ORIENTED_EDGE('',*,*,#4315,.F.);
#6474=ORIENTED_EDGE('',*,*,#4316,.F.);
#6475=ORIENTED_EDGE('',*,*,#4310,.T.);
#6476=ORIENTED_EDGE('',*,*,#4317,.T.);
#6477=ORIENTED_EDGE('',*,*,#4318,.F.);
#6478=ORIENTED_EDGE('',*,*,#4319,.F.);
#6479=ORIENTED_EDGE('',*,*,#4320,.F.);
#6480=ORIENTED_EDGE('',*,*,#4315,.T.);
#6481=ORIENTED_EDGE('',*,*,#4321,.T.);
#6482=ORIENTED_EDGE('',*,*,#4322,.T.);
#6483=ORIENTED_EDGE('',*,*,#4323,.F.);
#6484=ORIENTED_EDGE('',*,*,#4324,.F.);
#6485=ORIENTED_EDGE('',*,*,#4318,.T.);
#6486=ORIENTED_EDGE('',*,*,#4325,.T.);
#6487=ORIENTED_EDGE('',*,*,#4326,.T.);
#6488=ORIENTED_EDGE('',*,*,#4327,.T.);
#6489=ORIENTED_EDGE('',*,*,#4328,.T.);
#6490=ORIENTED_EDGE('',*,*,#4329,.T.);
#6491=ORIENTED_EDGE('',*,*,#4330,.T.);
#6492=ORIENTED_EDGE('',*,*,#4331,.T.);
#6493=ORIENTED_EDGE('',*,*,#4332,.T.);
#6494=ORIENTED_EDGE('',*,*,#4333,.T.);
#6495=ORIENTED_EDGE('',*,*,#4334,.T.);
#6496=ORIENTED_EDGE('',*,*,#4335,.T.);
#6497=ORIENTED_EDGE('',*,*,#4336,.T.);
#6498=ORIENTED_EDGE('',*,*,#4337,.T.);
#6499=ORIENTED_EDGE('',*,*,#4338,.T.);
#6500=ORIENTED_EDGE('',*,*,#4339,.T.);
#6501=ORIENTED_EDGE('',*,*,#4340,.T.);
#6502=ORIENTED_EDGE('',*,*,#4341,.T.);
#6503=ORIENTED_EDGE('',*,*,#4342,.T.);
#6504=ORIENTED_EDGE('',*,*,#4343,.T.);
#6505=ORIENTED_EDGE('',*,*,#4344,.T.);
#6506=ORIENTED_EDGE('',*,*,#4345,.T.);
#6507=ORIENTED_EDGE('',*,*,#4346,.T.);
#6508=ORIENTED_EDGE('',*,*,#4347,.T.);
#6509=ORIENTED_EDGE('',*,*,#4348,.T.);
#6510=ORIENTED_EDGE('',*,*,#4349,.T.);
#6511=ORIENTED_EDGE('',*,*,#4350,.T.);
#6512=ORIENTED_EDGE('',*,*,#4351,.T.);
#6513=ORIENTED_EDGE('',*,*,#4352,.T.);
#6514=ORIENTED_EDGE('',*,*,#4353,.T.);
#6515=ORIENTED_EDGE('',*,*,#4354,.T.);
#6516=ORIENTED_EDGE('',*,*,#4355,.T.);
#6517=ORIENTED_EDGE('',*,*,#4356,.T.);
#6518=ORIENTED_EDGE('',*,*,#4357,.T.);
#6519=ORIENTED_EDGE('',*,*,#4358,.T.);
#6520=ORIENTED_EDGE('',*,*,#4359,.T.);
#6521=ORIENTED_EDGE('',*,*,#4360,.T.);
#6522=ORIENTED_EDGE('',*,*,#4361,.T.);
#6523=ORIENTED_EDGE('',*,*,#4362,.T.);
#6524=ORIENTED_EDGE('',*,*,#4363,.T.);
#6525=ORIENTED_EDGE('',*,*,#4364,.T.);
#6526=ORIENTED_EDGE('',*,*,#4365,.T.);
#6527=ORIENTED_EDGE('',*,*,#4366,.T.);
#6528=ORIENTED_EDGE('',*,*,#4367,.T.);
#6529=ORIENTED_EDGE('',*,*,#4368,.T.);
#6530=ORIENTED_EDGE('',*,*,#4369,.T.);
#6531=ORIENTED_EDGE('',*,*,#4370,.T.);
#6532=ORIENTED_EDGE('',*,*,#4371,.T.);
#6533=ORIENTED_EDGE('',*,*,#4372,.T.);
#6534=ORIENTED_EDGE('',*,*,#4373,.T.);
#6535=ORIENTED_EDGE('',*,*,#4374,.T.);
#6536=ORIENTED_EDGE('',*,*,#4375,.T.);
#6537=ORIENTED_EDGE('',*,*,#4376,.T.);
#6538=ORIENTED_EDGE('',*,*,#4377,.T.);
#6539=ORIENTED_EDGE('',*,*,#4323,.T.);
#6540=ORIENTED_EDGE('',*,*,#4378,.T.);
#6541=ORIENTED_EDGE('',*,*,#4379,.T.);
#6542=ORIENTED_EDGE('',*,*,#4380,.T.);
#6543=ORIENTED_EDGE('',*,*,#4381,.F.);
#6544=ORIENTED_EDGE('',*,*,#4382,.F.);
#6545=ORIENTED_EDGE('',*,*,#4383,.F.);
#6546=ORIENTED_EDGE('',*,*,#4380,.F.);
#6547=ORIENTED_EDGE('',*,*,#4384,.F.);
#6548=ORIENTED_EDGE('',*,*,#4353,.F.);
#6549=ORIENTED_EDGE('',*,*,#4385,.F.);
#6550=ORIENTED_EDGE('',*,*,#4386,.F.);
#6551=ORIENTED_EDGE('',*,*,#4387,.T.);
#6552=ORIENTED_EDGE('',*,*,#4388,.F.);
#6553=ORIENTED_EDGE('',*,*,#4387,.F.);
#6554=ORIENTED_EDGE('',*,*,#4384,.T.);
#6555=ORIENTED_EDGE('',*,*,#4379,.F.);
#6556=ORIENTED_EDGE('',*,*,#4378,.F.);
#6557=ORIENTED_EDGE('',*,*,#4325,.F.);
#6558=ORIENTED_EDGE('',*,*,#4322,.F.);
#6559=ORIENTED_EDGE('',*,*,#4321,.F.);
#6560=ORIENTED_EDGE('',*,*,#4317,.F.);
#6561=ORIENTED_EDGE('',*,*,#4314,.F.);
#6562=ORIENTED_EDGE('',*,*,#4313,.F.);
#6563=ORIENTED_EDGE('',*,*,#4309,.F.);
#6564=ORIENTED_EDGE('',*,*,#4306,.F.);
#6565=ORIENTED_EDGE('',*,*,#4305,.F.);
#6566=ORIENTED_EDGE('',*,*,#4301,.F.);
#6567=ORIENTED_EDGE('',*,*,#4300,.F.);
#6568=ORIENTED_EDGE('',*,*,#4297,.F.);
#6569=ORIENTED_EDGE('',*,*,#4293,.F.);
#6570=ORIENTED_EDGE('',*,*,#4292,.F.);
#6571=ORIENTED_EDGE('',*,*,#4289,.F.);
#6572=ORIENTED_EDGE('',*,*,#4285,.F.);
#6573=ORIENTED_EDGE('',*,*,#4284,.F.);
#6574=ORIENTED_EDGE('',*,*,#4281,.F.);
#6575=ORIENTED_EDGE('',*,*,#4277,.F.);
#6576=ORIENTED_EDGE('',*,*,#4276,.F.);
#6577=ORIENTED_EDGE('',*,*,#4272,.F.);
#6578=ORIENTED_EDGE('',*,*,#4271,.F.);
#6579=ORIENTED_EDGE('',*,*,#4267,.F.);
#6580=ORIENTED_EDGE('',*,*,#4264,.F.);
#6581=ORIENTED_EDGE('',*,*,#4263,.F.);
#6582=ORIENTED_EDGE('',*,*,#4259,.F.);
#6583=ORIENTED_EDGE('',*,*,#4256,.F.);
#6584=ORIENTED_EDGE('',*,*,#4255,.F.);
#6585=ORIENTED_EDGE('',*,*,#4251,.F.);
#6586=ORIENTED_EDGE('',*,*,#4247,.F.);
#6587=ORIENTED_EDGE('',*,*,#4246,.F.);
#6588=ORIENTED_EDGE('',*,*,#4242,.F.);
#6589=ORIENTED_EDGE('',*,*,#4241,.F.);
#6590=ORIENTED_EDGE('',*,*,#4238,.F.);
#6591=ORIENTED_EDGE('',*,*,#4234,.F.);
#6592=ORIENTED_EDGE('',*,*,#4233,.F.);
#6593=ORIENTED_EDGE('',*,*,#4230,.F.);
#6594=ORIENTED_EDGE('',*,*,#4389,.F.);
#6595=ORIENTED_EDGE('',*,*,#4326,.F.);
#6596=ORIENTED_EDGE('',*,*,#4377,.F.);
#6597=ORIENTED_EDGE('',*,*,#4376,.F.);
#6598=ORIENTED_EDGE('',*,*,#4375,.F.);
#6599=ORIENTED_EDGE('',*,*,#4374,.F.);
#6600=ORIENTED_EDGE('',*,*,#4373,.F.);
#6601=ORIENTED_EDGE('',*,*,#4372,.F.);
#6602=ORIENTED_EDGE('',*,*,#4371,.F.);
#6603=ORIENTED_EDGE('',*,*,#4370,.F.);
#6604=ORIENTED_EDGE('',*,*,#4369,.F.);
#6605=ORIENTED_EDGE('',*,*,#4368,.F.);
#6606=ORIENTED_EDGE('',*,*,#4367,.F.);
#6607=ORIENTED_EDGE('',*,*,#4366,.F.);
#6608=ORIENTED_EDGE('',*,*,#4365,.F.);
#6609=ORIENTED_EDGE('',*,*,#4364,.F.);
#6610=ORIENTED_EDGE('',*,*,#4363,.F.);
#6611=ORIENTED_EDGE('',*,*,#4362,.F.);
#6612=ORIENTED_EDGE('',*,*,#4361,.F.);
#6613=ORIENTED_EDGE('',*,*,#4360,.F.);
#6614=ORIENTED_EDGE('',*,*,#4359,.F.);
#6615=ORIENTED_EDGE('',*,*,#4358,.F.);
#6616=ORIENTED_EDGE('',*,*,#4357,.F.);
#6617=ORIENTED_EDGE('',*,*,#4356,.F.);
#6618=ORIENTED_EDGE('',*,*,#4355,.F.);
#6619=ORIENTED_EDGE('',*,*,#4354,.F.);
#6620=ORIENTED_EDGE('',*,*,#4383,.T.);
#6621=ORIENTED_EDGE('',*,*,#4386,.T.);
#6622=ORIENTED_EDGE('',*,*,#4385,.T.);
#6623=ORIENTED_EDGE('',*,*,#4352,.F.);
#6624=ORIENTED_EDGE('',*,*,#4351,.F.);
#6625=ORIENTED_EDGE('',*,*,#4350,.F.);
#6626=ORIENTED_EDGE('',*,*,#4349,.F.);
#6627=ORIENTED_EDGE('',*,*,#4348,.F.);
#6628=ORIENTED_EDGE('',*,*,#4347,.F.);
#6629=ORIENTED_EDGE('',*,*,#4346,.F.);
#6630=ORIENTED_EDGE('',*,*,#4345,.F.);
#6631=ORIENTED_EDGE('',*,*,#4344,.F.);
#6632=ORIENTED_EDGE('',*,*,#4343,.F.);
#6633=ORIENTED_EDGE('',*,*,#4342,.F.);
#6634=ORIENTED_EDGE('',*,*,#4341,.F.);
#6635=ORIENTED_EDGE('',*,*,#4340,.F.);
#6636=ORIENTED_EDGE('',*,*,#4339,.F.);
#6637=ORIENTED_EDGE('',*,*,#4338,.F.);
#6638=ORIENTED_EDGE('',*,*,#4337,.F.);
#6639=ORIENTED_EDGE('',*,*,#4336,.F.);
#6640=ORIENTED_EDGE('',*,*,#4335,.F.);
#6641=ORIENTED_EDGE('',*,*,#4334,.F.);
#6642=ORIENTED_EDGE('',*,*,#4333,.F.);
#6643=ORIENTED_EDGE('',*,*,#4332,.F.);
#6644=ORIENTED_EDGE('',*,*,#4331,.F.);
#6645=ORIENTED_EDGE('',*,*,#4330,.F.);
#6646=ORIENTED_EDGE('',*,*,#4329,.F.);
#6647=ORIENTED_EDGE('',*,*,#4328,.F.);
#6648=ORIENTED_EDGE('',*,*,#4390,.F.);
#6649=ORIENTED_EDGE('',*,*,#4391,.T.);
#6650=ORIENTED_EDGE('',*,*,#4228,.T.);
#6651=ORIENTED_EDGE('',*,*,#4232,.T.);
#6652=ORIENTED_EDGE('',*,*,#4237,.T.);
#6653=ORIENTED_EDGE('',*,*,#4236,.T.);
#6654=ORIENTED_EDGE('',*,*,#4240,.T.);
#6655=ORIENTED_EDGE('',*,*,#4245,.T.);
#6656=ORIENTED_EDGE('',*,*,#4244,.T.);
#6657=ORIENTED_EDGE('',*,*,#4250,.T.);
#6658=ORIENTED_EDGE('',*,*,#4249,.T.);
#6659=ORIENTED_EDGE('',*,*,#4254,.T.);
#6660=ORIENTED_EDGE('',*,*,#4253,.T.);
#6661=ORIENTED_EDGE('',*,*,#4258,.T.);
#6662=ORIENTED_EDGE('',*,*,#4262,.T.);
#6663=ORIENTED_EDGE('',*,*,#4261,.T.);
#6664=ORIENTED_EDGE('',*,*,#4266,.T.);
#6665=ORIENTED_EDGE('',*,*,#4270,.T.);
#6666=ORIENTED_EDGE('',*,*,#4269,.T.);
#6667=ORIENTED_EDGE('',*,*,#4275,.T.);
#6668=ORIENTED_EDGE('',*,*,#4274,.T.);
#6669=ORIENTED_EDGE('',*,*,#4280,.T.);
#6670=ORIENTED_EDGE('',*,*,#4279,.T.);
#6671=ORIENTED_EDGE('',*,*,#4283,.T.);
#6672=ORIENTED_EDGE('',*,*,#4288,.T.);
#6673=ORIENTED_EDGE('',*,*,#4287,.T.);
#6674=ORIENTED_EDGE('',*,*,#4291,.T.);
#6675=ORIENTED_EDGE('',*,*,#4296,.T.);
#6676=ORIENTED_EDGE('',*,*,#4295,.T.);
#6677=ORIENTED_EDGE('',*,*,#4299,.T.);
#6678=ORIENTED_EDGE('',*,*,#4304,.T.);
#6679=ORIENTED_EDGE('',*,*,#4303,.T.);
#6680=ORIENTED_EDGE('',*,*,#4308,.T.);
#6681=ORIENTED_EDGE('',*,*,#4312,.T.);
#6682=ORIENTED_EDGE('',*,*,#4311,.T.);
#6683=ORIENTED_EDGE('',*,*,#4316,.T.);
#6684=ORIENTED_EDGE('',*,*,#4320,.T.);
#6685=ORIENTED_EDGE('',*,*,#4319,.T.);
#6686=ORIENTED_EDGE('',*,*,#4324,.T.);
#6687=ORIENTED_EDGE('',*,*,#4382,.T.);
#6688=ORIENTED_EDGE('',*,*,#4381,.T.);
#6689=ORIENTED_EDGE('',*,*,#4392,.F.);
#6690=ORIENTED_EDGE('',*,*,#4393,.T.);
#6691=ORIENTED_EDGE('',*,*,#4394,.T.);
#6692=ORIENTED_EDGE('',*,*,#4395,.F.);
#6693=ORIENTED_EDGE('',*,*,#4396,.F.);
#6694=ORIENTED_EDGE('',*,*,#4397,.T.);
#6695=ORIENTED_EDGE('',*,*,#4398,.T.);
#6696=ORIENTED_EDGE('',*,*,#4393,.F.);
#6697=ORIENTED_EDGE('',*,*,#4399,.F.);
#6698=ORIENTED_EDGE('',*,*,#4400,.T.);
#6699=ORIENTED_EDGE('',*,*,#4401,.T.);
#6700=ORIENTED_EDGE('',*,*,#4397,.F.);
#6701=ORIENTED_EDGE('',*,*,#4402,.F.);
#6702=ORIENTED_EDGE('',*,*,#4403,.T.);
#6703=ORIENTED_EDGE('',*,*,#4404,.T.);
#6704=ORIENTED_EDGE('',*,*,#4400,.F.);
#6705=ORIENTED_EDGE('',*,*,#4405,.F.);
#6706=ORIENTED_EDGE('',*,*,#4406,.T.);
#6707=ORIENTED_EDGE('',*,*,#4407,.T.);
#6708=ORIENTED_EDGE('',*,*,#4403,.F.);
#6709=ORIENTED_EDGE('',*,*,#4408,.F.);
#6710=ORIENTED_EDGE('',*,*,#4395,.T.);
#6711=ORIENTED_EDGE('',*,*,#4409,.T.);
#6712=ORIENTED_EDGE('',*,*,#4406,.F.);
#6713=ORIENTED_EDGE('',*,*,#4409,.F.);
#6714=ORIENTED_EDGE('',*,*,#4394,.F.);
#6715=ORIENTED_EDGE('',*,*,#4398,.F.);
#6716=ORIENTED_EDGE('',*,*,#4401,.F.);
#6717=ORIENTED_EDGE('',*,*,#4404,.F.);
#6718=ORIENTED_EDGE('',*,*,#4407,.F.);
#6719=ORIENTED_EDGE('',*,*,#4410,.T.);
#6720=ORIENTED_EDGE('',*,*,#4389,.T.);
#6721=ORIENTED_EDGE('',*,*,#4229,.T.);
#6722=ORIENTED_EDGE('',*,*,#4391,.F.);
#6723=ORIENTED_EDGE('',*,*,#4390,.T.);
#6724=ORIENTED_EDGE('',*,*,#4327,.F.);
#6725=ORIENTED_EDGE('',*,*,#4410,.F.);
#6726=ORIENTED_EDGE('',*,*,#4411,.T.);
#6727=ORIENTED_EDGE('',*,*,#4412,.T.);
#6728=ORIENTED_EDGE('',*,*,#4411,.F.);
#6729=ORIENTED_EDGE('',*,*,#4412,.F.);
#6730=ORIENTED_EDGE('',*,*,#4392,.T.);
#6731=ORIENTED_EDGE('',*,*,#4408,.T.);
#6732=ORIENTED_EDGE('',*,*,#4405,.T.);
#6733=ORIENTED_EDGE('',*,*,#4402,.T.);
#6734=ORIENTED_EDGE('',*,*,#4399,.T.);
#6735=ORIENTED_EDGE('',*,*,#4396,.T.);
#6736=ORIENTED_EDGE('',*,*,#4388,.T.);
#6737=CYLINDRICAL_SURFACE('',#7349,4.5);
#6738=CYLINDRICAL_SURFACE('',#7352,4.5);
#6739=CYLINDRICAL_SURFACE('',#7355,4.5);
#6740=CYLINDRICAL_SURFACE('',#7358,4.5);
#6741=CYLINDRICAL_SURFACE('',#7368,3.5);
#6742=CYLINDRICAL_SURFACE('',#7371,3.5);
#6743=CYLINDRICAL_SURFACE('',#7374,7.);
#6744=CYLINDRICAL_SURFACE('',#7377,8.);
#6745=CYLINDRICAL_SURFACE('',#7380,8.);
#6746=CYLINDRICAL_SURFACE('',#7390,5.);
#6747=CYLINDRICAL_SURFACE('',#7393,7.);
#6748=CYLINDRICAL_SURFACE('',#7399,6.767);
#6749=CYLINDRICAL_SURFACE('',#7401,6.767);
#6750=CYLINDRICAL_SURFACE('',#7402,6.767);
#6751=CYLINDRICAL_SURFACE('',#7403,6.767);
#6752=CYLINDRICAL_SURFACE('',#7404,6.767);
#6753=CYLINDRICAL_SURFACE('',#7405,6.767);
#6754=CYLINDRICAL_SURFACE('',#7406,6.767);
#6755=CYLINDRICAL_SURFACE('',#7407,6.767);
#6756=CYLINDRICAL_SURFACE('',#7408,6.767);
#6757=CYLINDRICAL_SURFACE('',#7409,6.767);
#6758=CYLINDRICAL_SURFACE('',#7410,6.767);
#6759=CYLINDRICAL_SURFACE('',#7411,6.767);
#6760=CYLINDRICAL_SURFACE('',#7412,6.767);
#6761=CYLINDRICAL_SURFACE('',#7413,6.767);
#6762=CYLINDRICAL_SURFACE('',#7414,6.767);
#6763=CYLINDRICAL_SURFACE('',#7415,6.767);
#6764=CYLINDRICAL_SURFACE('',#7416,6.767);
#6765=CYLINDRICAL_SURFACE('',#7417,6.767);
#6766=CYLINDRICAL_SURFACE('',#7418,6.767);
#6767=CYLINDRICAL_SURFACE('',#7419,6.767);
#6768=CYLINDRICAL_SURFACE('',#7420,6.767);
#6769=CYLINDRICAL_SURFACE('',#7421,6.767);
#6770=CYLINDRICAL_SURFACE('',#7422,6.767);
#6771=CYLINDRICAL_SURFACE('',#7423,6.767);
#6772=CYLINDRICAL_SURFACE('',#7424,6.767);
#6773=CYLINDRICAL_SURFACE('',#7425,6.767);
#6774=CYLINDRICAL_SURFACE('',#7426,6.767);
#6775=CYLINDRICAL_SURFACE('',#7427,6.767);
#6776=CYLINDRICAL_SURFACE('',#7428,6.767);
#6777=CYLINDRICAL_SURFACE('',#7429,6.767);
#6778=CYLINDRICAL_SURFACE('',#7430,6.767);
#6779=CYLINDRICAL_SURFACE('',#7431,6.767);
#6780=CYLINDRICAL_SURFACE('',#7432,6.767);
#6781=CYLINDRICAL_SURFACE('',#7433,6.767);
#6782=CYLINDRICAL_SURFACE('',#7434,6.767);
#6783=CYLINDRICAL_SURFACE('',#7435,6.767);
#6784=CYLINDRICAL_SURFACE('',#7436,6.767);
#6785=CYLINDRICAL_SURFACE('',#7437,6.767);
#6786=CYLINDRICAL_SURFACE('',#7438,6.767);
#6787=CYLINDRICAL_SURFACE('',#7439,6.767);
#6788=CYLINDRICAL_SURFACE('',#7440,6.767);
#6789=CYLINDRICAL_SURFACE('',#7441,6.767);
#6790=CYLINDRICAL_SURFACE('',#7442,6.767);
#6791=CYLINDRICAL_SURFACE('',#7443,6.767);
#6792=CYLINDRICAL_SURFACE('',#7444,6.767);
#6793=CYLINDRICAL_SURFACE('',#7445,6.767);
#6794=CYLINDRICAL_SURFACE('',#7446,6.767);
#6795=CYLINDRICAL_SURFACE('',#7447,6.767);
#6796=CYLINDRICAL_SURFACE('',#7448,6.767);
#6797=CYLINDRICAL_SURFACE('',#7449,6.767);
#6798=CYLINDRICAL_SURFACE('',#7450,6.767);
#6799=CYLINDRICAL_SURFACE('',#7451,6.767);
#6800=CYLINDRICAL_SURFACE('',#7452,6.767);
#6801=CYLINDRICAL_SURFACE('',#7453,6.767);
#6802=CYLINDRICAL_SURFACE('',#7454,6.767);
#6803=CYLINDRICAL_SURFACE('',#7455,6.767);
#6804=CYLINDRICAL_SURFACE('',#7456,6.767);
#6805=CYLINDRICAL_SURFACE('',#7457,6.767);
#6806=CYLINDRICAL_SURFACE('',#7458,6.767);
#6807=CYLINDRICAL_SURFACE('',#7459,6.767);
#6808=CYLINDRICAL_SURFACE('',#7460,6.767);
#6809=CYLINDRICAL_SURFACE('',#7461,6.767);
#6810=CYLINDRICAL_SURFACE('',#7462,6.767);
#6811=CYLINDRICAL_SURFACE('',#7463,6.767);
#6812=CYLINDRICAL_SURFACE('',#7464,6.767);
#6813=CYLINDRICAL_SURFACE('',#7465,6.767);
#6814=CYLINDRICAL_SURFACE('',#7466,6.767);
#6815=CYLINDRICAL_SURFACE('',#7467,6.767);
#6816=CYLINDRICAL_SURFACE('',#7468,6.767);
#6817=CYLINDRICAL_SURFACE('',#7469,6.767);
#6818=CYLINDRICAL_SURFACE('',#7470,6.767);
#6819=CYLINDRICAL_SURFACE('',#7471,6.767);
#6820=CYLINDRICAL_SURFACE('',#7472,6.767);
#6821=CYLINDRICAL_SURFACE('',#7473,6.767);
#6822=CYLINDRICAL_SURFACE('',#7474,6.767);
#6823=CYLINDRICAL_SURFACE('',#7475,6.767);
#6824=CYLINDRICAL_SURFACE('',#7476,6.767);
#6825=CYLINDRICAL_SURFACE('',#7477,6.767);
#6826=CYLINDRICAL_SURFACE('',#7479,7.911);
#6827=CYLINDRICAL_SURFACE('',#7482,4.);
#6828=CYLINDRICAL_SURFACE('',#7489,5.);
#6829=CYLINDRICAL_SURFACE('',#7491,5.);
#6830=CYLINDRICAL_SURFACE('',#7499,10.);
#6831=CYLINDRICAL_SURFACE('',#7502,8.);
#6832=CYLINDRICAL_SURFACE('',#7505,8.);
#6833=CYLINDRICAL_SURFACE('',#7508,8.);
#6834=CYLINDRICAL_SURFACE('',#7511,8.);
#6835=CYLINDRICAL_SURFACE('',#7524,45.);
#6836=CYLINDRICAL_SURFACE('',#7533,4.);
#6837=CYLINDRICAL_SURFACE('',#7535,8.);
#6838=CYLINDRICAL_SURFACE('',#7539,8.12525);
#6839=CYLINDRICAL_SURFACE('',#7541,8.12525);
#6840=CYLINDRICAL_SURFACE('',#7542,8.12525);
#6841=CYLINDRICAL_SURFACE('',#7543,8.12525);
#6842=CYLINDRICAL_SURFACE('',#7544,8.12525);
#6843=CYLINDRICAL_SURFACE('',#7545,8.12525);
#6844=CYLINDRICAL_SURFACE('',#7546,8.12525);
#6845=CYLINDRICAL_SURFACE('',#7547,8.12525);
#6846=CYLINDRICAL_SURFACE('',#7548,8.12525);
#6847=CYLINDRICAL_SURFACE('',#7549,8.12525);
#6848=CYLINDRICAL_SURFACE('',#7551,7.01125);
#6849=CYLINDRICAL_SURFACE('',#7553,7.01125);
#6850=CYLINDRICAL_SURFACE('',#7554,7.01125);
#6851=CYLINDRICAL_SURFACE('',#7555,7.01125);
#6852=CYLINDRICAL_SURFACE('',#7556,7.01125);
#6853=CYLINDRICAL_SURFACE('',#7557,7.01125);
#6854=CYLINDRICAL_SURFACE('',#7558,7.01125);
#6855=CYLINDRICAL_SURFACE('',#7559,7.01125);
#6856=CYLINDRICAL_SURFACE('',#7560,7.01125);
#6857=CYLINDRICAL_SURFACE('',#7561,7.01125);
#6858=CYLINDRICAL_SURFACE('',#7563,7.01125);
#6859=CYLINDRICAL_SURFACE('',#7564,8.12525);
#6860=CYLINDRICAL_SURFACE('',#7565,3.5);
#6861=CYLINDRICAL_SURFACE('',#7568,3.5);
#6862=CYLINDRICAL_SURFACE('',#7574,6.);
#6863=CYLINDRICAL_SURFACE('',#7576,6.);
#6864=CYLINDRICAL_SURFACE('',#7584,3.0735);
#6865=CYLINDRICAL_SURFACE('',#7586,3.0735);
#6866=CYLINDRICAL_SURFACE('',#7587,3.0735);
#6867=CYLINDRICAL_SURFACE('',#7588,3.0735);
#6868=CYLINDRICAL_SURFACE('',#7589,3.0735);
#6869=CYLINDRICAL_SURFACE('',#7590,3.0735);
#6870=CYLINDRICAL_SURFACE('',#7592,3.0735);
#6871=CYLINDRICAL_SURFACE('',#7594,3.0735);
#6872=CYLINDRICAL_SURFACE('',#7595,3.0735);
#6873=CYLINDRICAL_SURFACE('',#7596,3.0735);
#6874=CYLINDRICAL_SURFACE('',#7597,3.0735);
#6875=CYLINDRICAL_SURFACE('',#7598,3.0735);
#6876=CYLINDRICAL_SURFACE('',#7600,2.5175);
#6877=CYLINDRICAL_SURFACE('',#7602,2.5175);
#6878=CYLINDRICAL_SURFACE('',#7603,2.5175);
#6879=CYLINDRICAL_SURFACE('',#7604,2.5175);
#6880=CYLINDRICAL_SURFACE('',#7605,2.5175);
#6881=CYLINDRICAL_SURFACE('',#7606,2.5175);
#6882=CYLINDRICAL_SURFACE('',#7608,2.5175);
#6883=CYLINDRICAL_SURFACE('',#7610,2.5175);
#6884=CYLINDRICAL_SURFACE('',#7611,2.5175);
#6885=CYLINDRICAL_SURFACE('',#7612,2.5175);
#6886=CYLINDRICAL_SURFACE('',#7613,2.5175);
#6887=CYLINDRICAL_SURFACE('',#7614,2.5175);
#6888=CYLINDRICAL_SURFACE('',#7616,2.5175);
#6889=CYLINDRICAL_SURFACE('',#7617,2.5175);
#6890=CYLINDRICAL_SURFACE('',#7618,3.0735);
#6891=CYLINDRICAL_SURFACE('',#7619,3.0735);
#6892=CYLINDRICAL_SURFACE('',#7622,11.);
#6893=CYLINDRICAL_SURFACE('',#7630,5.);
#6894=CYLINDRICAL_SURFACE('',#7637,6.);
#6895=CYLINDRICAL_SURFACE('',#7642,8.);
#6896=CYLINDRICAL_SURFACE('',#7645,6.);
#6897=CYLINDRICAL_SURFACE('',#7653,5.);
#6898=CYLINDRICAL_SURFACE('',#7655,9.);
#6899=CYLINDRICAL_SURFACE('',#7659,6.);
#6900=CYLINDRICAL_SURFACE('',#7662,8.);
#6901=CYLINDRICAL_SURFACE('',#7668,5.);
#6902=CYLINDRICAL_SURFACE('',#7671,10.);
#6903=CYLINDRICAL_SURFACE('',#7677,2.37175);
#6904=CYLINDRICAL_SURFACE('',#7679,2.37175);
#6905=CYLINDRICAL_SURFACE('',#7680,2.37175);
#6906=CYLINDRICAL_SURFACE('',#7681,2.37175);
#6907=CYLINDRICAL_SURFACE('',#7682,2.37175);
#6908=CYLINDRICAL_SURFACE('',#7683,2.37175);
#6909=CYLINDRICAL_SURFACE('',#7684,2.37175);
#6910=CYLINDRICAL_SURFACE('',#7685,2.37175);
#6911=CYLINDRICAL_SURFACE('',#7686,2.37175);
#6912=CYLINDRICAL_SURFACE('',#7687,2.37175);
#6913=CYLINDRICAL_SURFACE('',#7688,2.37175);
#6914=CYLINDRICAL_SURFACE('',#7689,2.37175);
#6915=CYLINDRICAL_SURFACE('',#7690,2.37175);
#6916=CYLINDRICAL_SURFACE('',#7691,2.37175);
#6917=CYLINDRICAL_SURFACE('',#7692,2.37175);
#6918=CYLINDRICAL_SURFACE('',#7693,2.37175);
#6919=CYLINDRICAL_SURFACE('',#7694,2.37175);
#6920=CYLINDRICAL_SURFACE('',#7695,2.37175);
#6921=CYLINDRICAL_SURFACE('',#7696,2.37175);
#6922=CYLINDRICAL_SURFACE('',#7697,2.37175);
#6923=CYLINDRICAL_SURFACE('',#7698,2.37175);
#6924=CYLINDRICAL_SURFACE('',#7699,2.37175);
#6925=CYLINDRICAL_SURFACE('',#7700,2.37175);
#6926=CYLINDRICAL_SURFACE('',#7701,2.37175);
#6927=CYLINDRICAL_SURFACE('',#7702,2.942);
#6928=CYLINDRICAL_SURFACE('',#7705,2.37175);
#6929=CYLINDRICAL_SURFACE('',#7718,5.);
#6930=ADVANCED_FACE('',(#1065),#6737,.F.);
#6931=ADVANCED_FACE('',(#1066),#6738,.F.);
#6932=ADVANCED_FACE('',(#1067),#6739,.F.);
#6933=ADVANCED_FACE('',(#1068),#6740,.F.);
#6934=ADVANCED_FACE('',(#1069),#998,.T.);
#6935=ADVANCED_FACE('',(#1070),#999,.T.);
#6936=ADVANCED_FACE('',(#1071),#1000,.T.);
#6937=ADVANCED_FACE('',(#1072),#1001,.T.);
#6938=ADVANCED_FACE('',(#1073,#939,#940,#941,#942),#1002,.T.);
#6939=ADVANCED_FACE('',(#1074,#943,#944,#945,#946),#1003,.F.);
#6940=ADVANCED_FACE('',(#1075),#6741,.F.);
#6941=ADVANCED_FACE('',(#1076),#6742,.F.);
#6942=ADVANCED_FACE('',(#1077),#6743,.F.);
#6943=ADVANCED_FACE('',(#1078),#6744,.F.);
#6944=ADVANCED_FACE('',(#1079),#6745,.F.);
#6945=ADVANCED_FACE('',(#1080),#1004,.T.);
#6946=ADVANCED_FACE('',(#1081),#1005,.T.);
#6947=ADVANCED_FACE('',(#1082),#1006,.T.);
#6948=ADVANCED_FACE('',(#1083),#1007,.T.);
#6949=ADVANCED_FACE('',(#1084,#947,#948,#949,#950,#951),#1008,.T.);
#6950=ADVANCED_FACE('',(#1085,#952,#953,#954,#955,#956),#1009,.F.);
#6951=ADVANCED_FACE('',(#1086),#6746,.F.);
#6952=ADVANCED_FACE('',(#1087),#6747,.T.);
#6953=ADVANCED_FACE('',(#1088,#957),#1010,.T.);
#6954=ADVANCED_FACE('',(#1089,#958),#1011,.F.);
#6955=ADVANCED_FACE('',(#1090),#6748,.T.);
#6956=ADVANCED_FACE('',(#1091),#6749,.T.);
#6957=ADVANCED_FACE('',(#1092),#6750,.T.);
#6958=ADVANCED_FACE('',(#1093),#6751,.T.);
#6959=ADVANCED_FACE('',(#1094),#6752,.T.);
#6960=ADVANCED_FACE('',(#1095),#6753,.T.);
#6961=ADVANCED_FACE('',(#1096),#6754,.T.);
#6962=ADVANCED_FACE('',(#1097),#6755,.T.);
#6963=ADVANCED_FACE('',(#1098),#6756,.T.);
#6964=ADVANCED_FACE('',(#1099),#6757,.T.);
#6965=ADVANCED_FACE('',(#1100),#6758,.T.);
#6966=ADVANCED_FACE('',(#1101),#6759,.T.);
#6967=ADVANCED_FACE('',(#1102),#6760,.T.);
#6968=ADVANCED_FACE('',(#1103),#6761,.T.);
#6969=ADVANCED_FACE('',(#1104),#6762,.T.);
#6970=ADVANCED_FACE('',(#1105),#6763,.T.);
#6971=ADVANCED_FACE('',(#1106),#6764,.T.);
#6972=ADVANCED_FACE('',(#1107),#6765,.T.);
#6973=ADVANCED_FACE('',(#1108),#6766,.T.);
#6974=ADVANCED_FACE('',(#1109),#6767,.T.);
#6975=ADVANCED_FACE('',(#1110),#6768,.T.);
#6976=ADVANCED_FACE('',(#1111),#6769,.T.);
#6977=ADVANCED_FACE('',(#1112),#6770,.T.);
#6978=ADVANCED_FACE('',(#1113),#6771,.T.);
#6979=ADVANCED_FACE('',(#1114),#6772,.T.);
#6980=ADVANCED_FACE('',(#1115),#6773,.T.);
#6981=ADVANCED_FACE('',(#1116),#6774,.T.);
#6982=ADVANCED_FACE('',(#1117),#6775,.T.);
#6983=ADVANCED_FACE('',(#1118),#6776,.T.);
#6984=ADVANCED_FACE('',(#1119),#6777,.T.);
#6985=ADVANCED_FACE('',(#1120),#6778,.T.);
#6986=ADVANCED_FACE('',(#1121),#6779,.T.);
#6987=ADVANCED_FACE('',(#1122),#6780,.T.);
#6988=ADVANCED_FACE('',(#1123),#6781,.T.);
#6989=ADVANCED_FACE('',(#1124),#6782,.T.);
#6990=ADVANCED_FACE('',(#1125),#6783,.T.);
#6991=ADVANCED_FACE('',(#1126),#6784,.T.);
#6992=ADVANCED_FACE('',(#1127),#6785,.T.);
#6993=ADVANCED_FACE('',(#1128),#6786,.T.);
#6994=ADVANCED_FACE('',(#1129),#6787,.T.);
#6995=ADVANCED_FACE('',(#1130),#6788,.T.);
#6996=ADVANCED_FACE('',(#1131),#6789,.T.);
#6997=ADVANCED_FACE('',(#1132),#6790,.T.);
#6998=ADVANCED_FACE('',(#1133),#6791,.T.);
#6999=ADVANCED_FACE('',(#1134),#6792,.T.);
#7000=ADVANCED_FACE('',(#1135),#6793,.T.);
#7001=ADVANCED_FACE('',(#1136),#6794,.T.);
#7002=ADVANCED_FACE('',(#1137),#6795,.T.);
#7003=ADVANCED_FACE('',(#1138),#6796,.T.);
#7004=ADVANCED_FACE('',(#1139),#6797,.T.);
#7005=ADVANCED_FACE('',(#1140),#6798,.T.);
#7006=ADVANCED_FACE('',(#1141),#6799,.T.);
#7007=ADVANCED_FACE('',(#1142),#6800,.T.);
#7008=ADVANCED_FACE('',(#1143),#6801,.T.);
#7009=ADVANCED_FACE('',(#1144),#6802,.T.);
#7010=ADVANCED_FACE('',(#1145),#6803,.T.);
#7011=ADVANCED_FACE('',(#1146),#6804,.T.);
#7012=ADVANCED_FACE('',(#1147),#6805,.T.);
#7013=ADVANCED_FACE('',(#1148),#6806,.T.);
#7014=ADVANCED_FACE('',(#1149),#6807,.T.);
#7015=ADVANCED_FACE('',(#1150),#6808,.T.);
#7016=ADVANCED_FACE('',(#1151),#6809,.T.);
#7017=ADVANCED_FACE('',(#1152),#6810,.T.);
#7018=ADVANCED_FACE('',(#1153),#6811,.T.);
#7019=ADVANCED_FACE('',(#1154),#6812,.T.);
#7020=ADVANCED_FACE('',(#1155),#6813,.T.);
#7021=ADVANCED_FACE('',(#1156),#6814,.T.);
#7022=ADVANCED_FACE('',(#1157),#6815,.T.);
#7023=ADVANCED_FACE('',(#1158),#6816,.T.);
#7024=ADVANCED_FACE('',(#1159),#6817,.T.);
#7025=ADVANCED_FACE('',(#1160),#6818,.T.);
#7026=ADVANCED_FACE('',(#1161),#6819,.T.);
#7027=ADVANCED_FACE('',(#1162),#6820,.T.);
#7028=ADVANCED_FACE('',(#1163),#6821,.T.);
#7029=ADVANCED_FACE('',(#1164),#6822,.T.);
#7030=ADVANCED_FACE('',(#1165),#6823,.T.);
#7031=ADVANCED_FACE('',(#1166),#6824,.T.);
#7032=ADVANCED_FACE('',(#1167),#6825,.T.);
#7033=ADVANCED_FACE('',(#1168),#6826,.T.);
#7034=ADVANCED_FACE('',(#1169),#6827,.T.);
#7035=ADVANCED_FACE('',(#1170,#959),#1012,.F.);
#7036=ADVANCED_FACE('',(#1171,#960),#1013,.F.);
#7037=ADVANCED_FACE('',(#1172),#6828,.T.);
#7038=ADVANCED_FACE('',(#1173),#6829,.T.);
#7039=ADVANCED_FACE('',(#1174),#1014,.T.);
#7040=ADVANCED_FACE('',(#1175,#961),#1015,.F.);
#7041=ADVANCED_FACE('',(#1176),#6830,.T.);
#7042=ADVANCED_FACE('',(#1177,#962),#1016,.T.);
#7043=ADVANCED_FACE('',(#1178),#6831,.F.);
#7044=ADVANCED_FACE('',(#1179),#6832,.F.);
#7045=ADVANCED_FACE('',(#1180),#6833,.F.);
#7046=ADVANCED_FACE('',(#1181),#6834,.F.);
#7047=ADVANCED_FACE('',(#1182),#105,.T.);
#7048=ADVANCED_FACE('',(#1183),#95,.F.);
#7049=ADVANCED_FACE('',(#1184),#96,.F.);
#7050=ADVANCED_FACE('',(#1185),#1017,.F.);
#7051=ADVANCED_FACE('',(#1186),#1018,.F.);
#7052=ADVANCED_FACE('',(#1187),#1019,.F.);
#7053=ADVANCED_FACE('',(#1188),#1020,.F.);
#7054=ADVANCED_FACE('',(#1189),#1021,.F.);
#7055=ADVANCED_FACE('',(#1190),#1022,.F.);
#7056=ADVANCED_FACE('',(#1191),#1023,.F.);
#7057=ADVANCED_FACE('',(#1192,#963,#964,#965,#966,#967),#1024,.T.);
#7058=ADVANCED_FACE('',(#1193),#6835,.T.);
#7059=ADVANCED_FACE('',(#1194,#968,#969,#970,#971,#972),#1025,.F.);
#7060=ADVANCED_FACE('',(#1195),#1026,.F.);
#7061=ADVANCED_FACE('',(#1196),#1027,.F.);
#7062=ADVANCED_FACE('',(#1197),#1028,.F.);
#7063=ADVANCED_FACE('',(#1198),#6836,.F.);
#7064=ADVANCED_FACE('',(#1199),#6837,.T.);
#7065=ADVANCED_FACE('',(#1200),#1029,.T.);
#7066=ADVANCED_FACE('',(#1201),#6838,.F.);
#7067=ADVANCED_FACE('',(#1202),#6839,.F.);
#7068=ADVANCED_FACE('',(#1203),#6840,.F.);
#7069=ADVANCED_FACE('',(#1204),#6841,.F.);
#7070=ADVANCED_FACE('',(#1205),#6842,.F.);
#7071=ADVANCED_FACE('',(#1206),#6843,.F.);
#7072=ADVANCED_FACE('',(#1207),#6844,.F.);
#7073=ADVANCED_FACE('',(#1208),#6845,.F.);
#7074=ADVANCED_FACE('',(#1209),#6846,.F.);
#7075=ADVANCED_FACE('',(#1210),#6847,.F.);
#7076=ADVANCED_FACE('',(#1211),#6848,.F.);
#7077=ADVANCED_FACE('',(#1212),#6849,.F.);
#7078=ADVANCED_FACE('',(#1213),#6850,.F.);
#7079=ADVANCED_FACE('',(#1214),#6851,.F.);
#7080=ADVANCED_FACE('',(#1215),#6852,.F.);
#7081=ADVANCED_FACE('',(#1216),#6853,.F.);
#7082=ADVANCED_FACE('',(#1217),#6854,.F.);
#7083=ADVANCED_FACE('',(#1218),#6855,.F.);
#7084=ADVANCED_FACE('',(#1219),#6856,.F.);
#7085=ADVANCED_FACE('',(#1220),#6857,.F.);
#7086=ADVANCED_FACE('',(#1221),#6858,.F.);
#7087=ADVANCED_FACE('',(#1222),#6859,.F.);
#7088=ADVANCED_FACE('',(#1223),#6860,.F.);
#7089=ADVANCED_FACE('',(#1224),#6861,.F.);
#7090=ADVANCED_FACE('',(#1225),#97,.F.);
#7091=ADVANCED_FACE('',(#1226),#98,.F.);
#7092=ADVANCED_FACE('',(#1227,#973,#974,#975,#976,#977),#1030,.T.);
#7093=ADVANCED_FACE('',(#1228),#6862,.F.);
#7094=ADVANCED_FACE('',(#1229),#6863,.F.);
#7095=ADVANCED_FACE('',(#1230),#1031,.T.);
#7096=ADVANCED_FACE('',(#1231),#1032,.T.);
#7097=ADVANCED_FACE('',(#1232),#1033,.T.);
#7098=ADVANCED_FACE('',(#1233),#1034,.T.);
#7099=ADVANCED_FACE('',(#1234,#978,#979,#980,#981,#982),#1035,.F.);
#7100=ADVANCED_FACE('',(#1235),#6864,.F.);
#7101=ADVANCED_FACE('',(#1236),#6865,.F.);
#7102=ADVANCED_FACE('',(#1237),#6866,.F.);
#7103=ADVANCED_FACE('',(#1238),#6867,.F.);
#7104=ADVANCED_FACE('',(#1239),#6868,.F.);
#7105=ADVANCED_FACE('',(#1240),#6869,.F.);
#7106=ADVANCED_FACE('',(#1241),#6870,.F.);
#7107=ADVANCED_FACE('',(#1242),#6871,.F.);
#7108=ADVANCED_FACE('',(#1243),#6872,.F.);
#7109=ADVANCED_FACE('',(#1244),#6873,.F.);
#7110=ADVANCED_FACE('',(#1245),#6874,.F.);
#7111=ADVANCED_FACE('',(#1246),#6875,.F.);
#7112=ADVANCED_FACE('',(#1247),#6876,.F.);
#7113=ADVANCED_FACE('',(#1248),#6877,.F.);
#7114=ADVANCED_FACE('',(#1249),#6878,.F.);
#7115=ADVANCED_FACE('',(#1250),#6879,.F.);
#7116=ADVANCED_FACE('',(#1251),#6880,.F.);
#7117=ADVANCED_FACE('',(#1252),#6881,.F.);
#7118=ADVANCED_FACE('',(#1253),#6882,.F.);
#7119=ADVANCED_FACE('',(#1254),#6883,.F.);
#7120=ADVANCED_FACE('',(#1255),#6884,.F.);
#7121=ADVANCED_FACE('',(#1256),#6885,.F.);
#7122=ADVANCED_FACE('',(#1257),#6886,.F.);
#7123=ADVANCED_FACE('',(#1258),#6887,.F.);
#7124=ADVANCED_FACE('',(#1259),#6888,.F.);
#7125=ADVANCED_FACE('',(#1260),#6889,.F.);
#7126=ADVANCED_FACE('',(#1261),#6890,.F.);
#7127=ADVANCED_FACE('',(#1262),#6891,.F.);
#7128=ADVANCED_FACE('',(#1263),#99,.F.);
#7129=ADVANCED_FACE('',(#1264),#100,.F.);
#7130=ADVANCED_FACE('',(#1265,#983,#984,#985),#1036,.T.);
#7131=ADVANCED_FACE('',(#1266),#101,.F.);
#7132=ADVANCED_FACE('',(#1267),#102,.F.);
#7133=ADVANCED_FACE('',(#1268),#6892,.F.);
#7134=ADVANCED_FACE('',(#1269),#1037,.T.);
#7135=ADVANCED_FACE('',(#1270),#1038,.T.);
#7136=ADVANCED_FACE('',(#1271),#1039,.T.);
#7137=ADVANCED_FACE('',(#1272),#1040,.T.);
#7138=ADVANCED_FACE('',(#1273,#986,#987,#988),#1041,.F.);
#7139=ADVANCED_FACE('',(#1274),#6893,.T.);
#7140=ADVANCED_FACE('',(#1275,#989),#1042,.F.);
#7141=ADVANCED_FACE('',(#1276,#990),#1043,.F.);
#7142=ADVANCED_FACE('',(#1277),#6894,.T.);
#7143=ADVANCED_FACE('',(#1278,#991),#1044,.T.);
#7144=ADVANCED_FACE('',(#1279),#6895,.T.);
#7145=ADVANCED_FACE('',(#1280),#1045,.F.);
#7146=ADVANCED_FACE('',(#1281),#6896,.T.);
#7147=ADVANCED_FACE('',(#1282),#1046,.T.);
#7148=ADVANCED_FACE('',(#1283),#1047,.F.);
#7149=ADVANCED_FACE('',(#1284),#1048,.F.);
#7150=ADVANCED_FACE('',(#1285),#1049,.F.);
#7151=ADVANCED_FACE('',(#1286),#6897,.F.);
#7152=ADVANCED_FACE('',(#1287),#6898,.T.);
#7153=ADVANCED_FACE('',(#1288),#1050,.T.);
#7154=ADVANCED_FACE('',(#1289),#6899,.F.);
#7155=ADVANCED_FACE('',(#1290),#6900,.T.);
#7156=ADVANCED_FACE('',(#1291,#992),#1051,.T.);
#7157=ADVANCED_FACE('',(#1292,#993),#1052,.F.);
#7158=ADVANCED_FACE('',(#1293),#6901,.F.);
#7159=ADVANCED_FACE('',(#1294),#6902,.T.);
#7160=ADVANCED_FACE('',(#1295,#994),#1053,.T.);
#7161=ADVANCED_FACE('',(#1296,#995),#1054,.F.);
#7162=ADVANCED_FACE('',(#1297),#6903,.T.);
#7163=ADVANCED_FACE('',(#1298),#6904,.T.);
#7164=ADVANCED_FACE('',(#1299),#6905,.T.);
#7165=ADVANCED_FACE('',(#1300),#6906,.T.);
#7166=ADVANCED_FACE('',(#1301),#6907,.T.);
#7167=ADVANCED_FACE('',(#1302),#6908,.T.);
#7168=ADVANCED_FACE('',(#1303),#6909,.T.);
#7169=ADVANCED_FACE('',(#1304),#6910,.T.);
#7170=ADVANCED_FACE('',(#1305),#6911,.T.);
#7171=ADVANCED_FACE('',(#1306),#6912,.T.);
#7172=ADVANCED_FACE('',(#1307),#6913,.T.);
#7173=ADVANCED_FACE('',(#1308),#6914,.T.);
#7174=ADVANCED_FACE('',(#1309),#6915,.T.);
#7175=ADVANCED_FACE('',(#1310),#6916,.T.);
#7176=ADVANCED_FACE('',(#1311),#6917,.T.);
#7177=ADVANCED_FACE('',(#1312),#6918,.T.);
#7178=ADVANCED_FACE('',(#1313),#6919,.T.);
#7179=ADVANCED_FACE('',(#1314),#6920,.T.);
#7180=ADVANCED_FACE('',(#1315),#6921,.T.);
#7181=ADVANCED_FACE('',(#1316),#6922,.T.);
#7182=ADVANCED_FACE('',(#1317),#6923,.T.);
#7183=ADVANCED_FACE('',(#1318),#6924,.T.);
#7184=ADVANCED_FACE('',(#1319),#6925,.T.);
#7185=ADVANCED_FACE('',(#1320),#6926,.T.);
#7186=ADVANCED_FACE('',(#1321),#6927,.T.);
#7187=ADVANCED_FACE('',(#1322),#6928,.T.);
#7188=ADVANCED_FACE('',(#1323),#106,.T.);
#7189=ADVANCED_FACE('',(#1324),#103,.F.);
#7190=ADVANCED_FACE('',(#1325),#104,.F.);
#7191=ADVANCED_FACE('',(#1326),#1055,.F.);
#7192=ADVANCED_FACE('',(#1327),#1056,.F.);
#7193=ADVANCED_FACE('',(#1328),#1057,.F.);
#7194=ADVANCED_FACE('',(#1329),#1058,.F.);
#7195=ADVANCED_FACE('',(#1330),#1059,.F.);
#7196=ADVANCED_FACE('',(#1331),#1060,.F.);
#7197=ADVANCED_FACE('',(#1332),#1061,.F.);
#7198=ADVANCED_FACE('',(#1333,#996),#1062,.T.);
#7199=ADVANCED_FACE('',(#1334),#6929,.T.);
#7200=ADVANCED_FACE('',(#1335,#997),#1063,.F.);
#7201=ADVANCED_FACE('',(#1336),#1064,.T.);
#7202=CLOSED_SHELL('',(#6930,#6931,#6932,#6933,#6934,#6935,#6936,#6937,
#6938,#6939));
#7203=CLOSED_SHELL('',(#6940,#6941,#6942,#6943,#6944,#6945,#6946,#6947,
#6948,#6949,#6950));
#7204=CLOSED_SHELL('',(#6951,#6952,#6953,#6954));
#7205=CLOSED_SHELL('',(#6955,#6956,#6957,#6958,#6959,#6960,#6961,#6962,
#6963,#6964,#6965,#6966,#6967,#6968,#6969,#6970,#6971,#6972,#6973,#6974,
#6975,#6976,#6977,#6978,#6979,#6980,#6981,#6982,#6983,#6984,#6985,#6986,
#6987,#6988,#6989,#6990,#6991,#6992,#6993,#6994,#6995,#6996,#6997,#6998,
#6999,#7000,#7001,#7002,#7003,#7004,#7005,#7006,#7007,#7008,#7009,#7010,
#7011,#7012,#7013,#7014,#7015,#7016,#7017,#7018,#7019,#7020,#7021,#7022,
#7023,#7024,#7025,#7026,#7027,#7028,#7029,#7030,#7031,#7032,#7033,#7034,
#7035,#7036,#7037,#7038,#7039,#7040,#7041,#7042,#7043,#7044,#7045,#7046,
#7047,#7048,#7049,#7050,#7051,#7052,#7053,#7054,#7055,#7056,#7057,#7058,
#7059));
#7206=CLOSED_SHELL('',(#7060,#7061,#7062,#7063,#7064,#7065));
#7207=CLOSED_SHELL('',(#7066,#7067,#7068,#7069,#7070,#7071,#7072,#7073,
#7074,#7075,#7076,#7077,#7078,#7079,#7080,#7081,#7082,#7083,#7084,#7085,
#7086,#7087,#7088,#7089,#7090,#7091,#7092,#7093,#7094,#7095,#7096,#7097,
#7098,#7099));
#7208=CLOSED_SHELL('',(#7100,#7101,#7102,#7103,#7104,#7105,#7106,#7107,
#7108,#7109,#7110,#7111,#7112,#7113,#7114,#7115,#7116,#7117,#7118,#7119,
#7120,#7121,#7122,#7123,#7124,#7125,#7126,#7127,#7128,#7129,#7130,#7131,
#7132,#7133,#7134,#7135,#7136,#7137,#7138));
#7209=CLOSED_SHELL('',(#7139,#7140,#7141,#7142,#7143,#7144,#7145,#7146,
#7147));
#7210=CLOSED_SHELL('',(#7148,#7149,#7150,#7151,#7152,#7153));
#7211=CLOSED_SHELL('',(#7154,#7155,#7156,#7157));
#7212=CLOSED_SHELL('',(#7158,#7159,#7160,#7161));
#7213=CLOSED_SHELL('',(#7162,#7163,#7164,#7165,#7166,#7167,#7168,#7169,
#7170,#7171,#7172,#7173,#7174,#7175,#7176,#7177,#7178,#7179,#7180,#7181,
#7182,#7183,#7184,#7185,#7186,#7187,#7188,#7189,#7190,#7191,#7192,#7193,
#7194,#7195,#7196,#7197,#7198,#7199,#7200,#7201));
#7214=DERIVED_UNIT_ELEMENT(#7238,1.);
#7215=DERIVED_UNIT_ELEMENT(#105808,-3.);
#7216=DERIVED_UNIT_ELEMENT(#7238,1.);
#7217=DERIVED_UNIT_ELEMENT(#105808,-3.);
#7218=DERIVED_UNIT_ELEMENT(#7238,1.);
#7219=DERIVED_UNIT_ELEMENT(#105808,-3.);
#7220=DERIVED_UNIT_ELEMENT(#7238,1.);
#7221=DERIVED_UNIT_ELEMENT(#105808,-3.);
#7222=DERIVED_UNIT_ELEMENT(#7238,1.);
#7223=DERIVED_UNIT_ELEMENT(#105808,-3.);
#7224=DERIVED_UNIT_ELEMENT(#7238,1.);
#7225=DERIVED_UNIT_ELEMENT(#105808,-3.);
#7226=DERIVED_UNIT_ELEMENT(#7238,1.);
#7227=DERIVED_UNIT_ELEMENT(#105808,-3.);
#7228=DERIVED_UNIT_ELEMENT(#7238,1.);
#7229=DERIVED_UNIT_ELEMENT(#105808,-3.);
#7230=DERIVED_UNIT_ELEMENT(#7238,1.);
#7231=DERIVED_UNIT_ELEMENT(#105808,-3.);
#7232=DERIVED_UNIT_ELEMENT(#7238,1.);
#7233=DERIVED_UNIT_ELEMENT(#105808,-3.);
#7234=DERIVED_UNIT_ELEMENT(#7238,1.);
#7235=DERIVED_UNIT_ELEMENT(#105808,-3.);
#7236=DERIVED_UNIT_ELEMENT(#7238,1.);
#7237=DERIVED_UNIT_ELEMENT(#105808,-3.);
#7238=(
MASS_UNIT()
NAMED_UNIT(*)
SI_UNIT(.KILO.,.GRAM.)
);
#7239=DERIVED_UNIT((#7214,#7215));
#7240=DERIVED_UNIT((#7216,#7217));
#7241=DERIVED_UNIT((#7218,#7219));
#7242=DERIVED_UNIT((#7220,#7221));
#7243=DERIVED_UNIT((#7222,#7223));
#7244=DERIVED_UNIT((#7224,#7225));
#7245=DERIVED_UNIT((#7226,#7227));
#7246=DERIVED_UNIT((#7228,#7229));
#7247=DERIVED_UNIT((#7230,#7231));
#7248=DERIVED_UNIT((#7232,#7233));
#7249=DERIVED_UNIT((#7234,#7235));
#7250=DERIVED_UNIT((#7236,#7237));
#7251=MEASURE_REPRESENTATION_ITEM('density measure',
POSITIVE_RATIO_MEASURE(7850.),#7239);
#7252=MEASURE_REPRESENTATION_ITEM('density measure',
POSITIVE_RATIO_MEASURE(7850.),#7240);
#7253=MEASURE_REPRESENTATION_ITEM('density measure',
POSITIVE_RATIO_MEASURE(8920.),#7241);
#7254=MEASURE_REPRESENTATION_ITEM('density measure',
POSITIVE_RATIO_MEASURE(7850.),#7242);
#7255=MEASURE_REPRESENTATION_ITEM('density measure',
POSITIVE_RATIO_MEASURE(7850.),#7243);
#7256=MEASURE_REPRESENTATION_ITEM('density measure',
POSITIVE_RATIO_MEASURE(7850.),#7244);
#7257=MEASURE_REPRESENTATION_ITEM('density measure',
POSITIVE_RATIO_MEASURE(7850.),#7245);
#7258=MEASURE_REPRESENTATION_ITEM('density measure',
POSITIVE_RATIO_MEASURE(7850.),#7246);
#7259=MEASURE_REPRESENTATION_ITEM('density measure',
POSITIVE_RATIO_MEASURE(7850.),#7247);
#7260=MEASURE_REPRESENTATION_ITEM('density measure',
POSITIVE_RATIO_MEASURE(8920.),#7248);
#7261=MEASURE_REPRESENTATION_ITEM('density measure',
POSITIVE_RATIO_MEASURE(7850.),#7249);
#7262=MEASURE_REPRESENTATION_ITEM('density measure',
POSITIVE_RATIO_MEASURE(7850.),#7250);
#7263=PROPERTY_DEFINITION_REPRESENTATION(#7323,#7287);
#7264=PROPERTY_DEFINITION_REPRESENTATION(#7324,#7288);
#7265=PROPERTY_DEFINITION_REPRESENTATION(#7325,#7289);
#7266=PROPERTY_DEFINITION_REPRESENTATION(#7326,#7290);
#7267=PROPERTY_DEFINITION_REPRESENTATION(#7327,#7291);
#7268=PROPERTY_DEFINITION_REPRESENTATION(#7328,#7292);
#7269=PROPERTY_DEFINITION_REPRESENTATION(#7329,#7293);
#7270=PROPERTY_DEFINITION_REPRESENTATION(#7330,#7294);
#7271=PROPERTY_DEFINITION_REPRESENTATION(#7331,#7295);
#7272=PROPERTY_DEFINITION_REPRESENTATION(#7332,#7296);
#7273=PROPERTY_DEFINITION_REPRESENTATION(#7333,#7297);
#7274=PROPERTY_DEFINITION_REPRESENTATION(#7334,#7298);
#7275=PROPERTY_DEFINITION_REPRESENTATION(#7335,#7299);
#7276=PROPERTY_DEFINITION_REPRESENTATION(#7336,#7300);
#7277=PROPERTY_DEFINITION_REPRESENTATION(#7337,#7301);
#7278=PROPERTY_DEFINITION_REPRESENTATION(#7338,#7302);
#7279=PROPERTY_DEFINITION_REPRESENTATION(#7339,#7303);
#7280=PROPERTY_DEFINITION_REPRESENTATION(#7340,#7304);
#7281=PROPERTY_DEFINITION_REPRESENTATION(#7341,#7305);
#7282=PROPERTY_DEFINITION_REPRESENTATION(#7342,#7306);
#7283=PROPERTY_DEFINITION_REPRESENTATION(#7343,#7307);
#7284=PROPERTY_DEFINITION_REPRESENTATION(#7344,#7308);
#7285=PROPERTY_DEFINITION_REPRESENTATION(#7345,#7309);
#7286=PROPERTY_DEFINITION_REPRESENTATION(#7346,#7310);
#7287=REPRESENTATION('material name',(#7311),#105794);
#7288=REPRESENTATION('density',(#7251),#105794);
#7289=REPRESENTATION('material name',(#7312),#105795);
#7290=REPRESENTATION('density',(#7252),#105795);
#7291=REPRESENTATION('material name',(#7313),#105796);
#7292=REPRESENTATION('density',(#7253),#105796);
#7293=REPRESENTATION('material name',(#7314),#105797);
#7294=REPRESENTATION('density',(#7254),#105797);
#7295=REPRESENTATION('material name',(#7315),#105798);
#7296=REPRESENTATION('density',(#7255),#105798);
#7297=REPRESENTATION('material name',(#7316),#105799);
#7298=REPRESENTATION('density',(#7256),#105799);
#7299=REPRESENTATION('material name',(#7317),#105800);
#7300=REPRESENTATION('density',(#7257),#105800);
#7301=REPRESENTATION('material name',(#7318),#105801);
#7302=REPRESENTATION('density',(#7258),#105801);
#7303=REPRESENTATION('material name',(#7319),#105802);
#7304=REPRESENTATION('density',(#7259),#105802);
#7305=REPRESENTATION('material name',(#7320),#105803);
#7306=REPRESENTATION('density',(#7260),#105803);
#7307=REPRESENTATION('material name',(#7321),#105804);
#7308=REPRESENTATION('density',(#7261),#105804);
#7309=REPRESENTATION('material name',(#7322),#105805);
#7310=REPRESENTATION('density',(#7262),#105805);
#7311=DESCRIPTIVE_REPRESENTATION_ITEM('Steel','Steel');
#7312=DESCRIPTIVE_REPRESENTATION_ITEM('Steel','Steel');
#7313=DESCRIPTIVE_REPRESENTATION_ITEM('Copper, Alloy','Copper, Alloy');
#7314=DESCRIPTIVE_REPRESENTATION_ITEM('Steel','Steel');
#7315=DESCRIPTIVE_REPRESENTATION_ITEM('Steel','Steel');
#7316=DESCRIPTIVE_REPRESENTATION_ITEM('Steel','Steel');
#7317=DESCRIPTIVE_REPRESENTATION_ITEM('Steel','Steel');
#7318=DESCRIPTIVE_REPRESENTATION_ITEM('Steel','Steel');
#7319=DESCRIPTIVE_REPRESENTATION_ITEM('Steel','Steel');
#7320=DESCRIPTIVE_REPRESENTATION_ITEM('Copper, Alloy','Copper, Alloy');
#7321=DESCRIPTIVE_REPRESENTATION_ITEM('Steel','Steel');
#7322=DESCRIPTIVE_REPRESENTATION_ITEM('Steel','Steel');
#7323=PROPERTY_DEFINITION('material property','material name',#105873);
#7324=PROPERTY_DEFINITION('material property','density of part',#105873);
#7325=PROPERTY_DEFINITION('material property','material name',#105874);
#7326=PROPERTY_DEFINITION('material property','density of part',#105874);
#7327=PROPERTY_DEFINITION('material property','material name',#105875);
#7328=PROPERTY_DEFINITION('material property','density of part',#105875);
#7329=PROPERTY_DEFINITION('material property','material name',#105876);
#7330=PROPERTY_DEFINITION('material property','density of part',#105876);
#7331=PROPERTY_DEFINITION('material property','material name',#105877);
#7332=PROPERTY_DEFINITION('material property','density of part',#105877);
#7333=PROPERTY_DEFINITION('material property','material name',#105878);
#7334=PROPERTY_DEFINITION('material property','density of part',#105878);
#7335=PROPERTY_DEFINITION('material property','material name',#105879);
#7336=PROPERTY_DEFINITION('material property','density of part',#105879);
#7337=PROPERTY_DEFINITION('material property','material name',#105880);
#7338=PROPERTY_DEFINITION('material property','density of part',#105880);
#7339=PROPERTY_DEFINITION('material property','material name',#105881);
#7340=PROPERTY_DEFINITION('material property','density of part',#105881);
#7341=PROPERTY_DEFINITION('material property','material name',#105882);
#7342=PROPERTY_DEFINITION('material property','density of part',#105882);
#7343=PROPERTY_DEFINITION('material property','material name',#105883);
#7344=PROPERTY_DEFINITION('material property','density of part',#105883);
#7345=PROPERTY_DEFINITION('material property','material name',#105884);
#7346=PROPERTY_DEFINITION('material property','density of part',#105884);
#7347=AXIS2_PLACEMENT_3D('',#8815,#7743,#7744);
#7348=AXIS2_PLACEMENT_3D('',#8816,#7745,#7746);
#7349=AXIS2_PLACEMENT_3D('',#8817,#7747,#7748);
#7350=AXIS2_PLACEMENT_3D('',#8819,#7749,#7750);
#7351=AXIS2_PLACEMENT_3D('',#8822,#7752,#7753);
#7352=AXIS2_PLACEMENT_3D('',#8823,#7754,#7755);
#7353=AXIS2_PLACEMENT_3D('',#8825,#7756,#7757);
#7354=AXIS2_PLACEMENT_3D('',#8828,#7759,#7760);
#7355=AXIS2_PLACEMENT_3D('',#8829,#7761,#7762);
#7356=AXIS2_PLACEMENT_3D('',#8831,#7763,#7764);
#7357=AXIS2_PLACEMENT_3D('',#8834,#7766,#7767);
#7358=AXIS2_PLACEMENT_3D('',#8835,#7768,#7769);
#7359=AXIS2_PLACEMENT_3D('',#8837,#7770,#7771);
#7360=AXIS2_PLACEMENT_3D('',#8840,#7773,#7774);
#7361=AXIS2_PLACEMENT_3D('',#8841,#7775,#7776);
#7362=AXIS2_PLACEMENT_3D('',#8850,#7781,#7782);
#7363=AXIS2_PLACEMENT_3D('',#8856,#7786,#7787);
#7364=AXIS2_PLACEMENT_3D('',#8862,#7791,#7792);
#7365=AXIS2_PLACEMENT_3D('',#8865,#7795,#7796);
#7366=AXIS2_PLACEMENT_3D('',#8866,#7797,#7798);
#7367=AXIS2_PLACEMENT_3D('',#8867,#7799,#7800);
#7368=AXIS2_PLACEMENT_3D('',#8868,#7801,#7802);
#7369=AXIS2_PLACEMENT_3D('',#8870,#7803,#7804);
#7370=AXIS2_PLACEMENT_3D('',#8873,#7806,#7807);
#7371=AXIS2_PLACEMENT_3D('',#8874,#7808,#7809);
#7372=AXIS2_PLACEMENT_3D('',#8876,#7810,#7811);
#7373=AXIS2_PLACEMENT_3D('',#8879,#7813,#7814);
#7374=AXIS2_PLACEMENT_3D('',#8880,#7815,#7816);
#7375=AXIS2_PLACEMENT_3D('',#8882,#7817,#7818);
#7376=AXIS2_PLACEMENT_3D('',#8885,#7820,#7821);
#7377=AXIS2_PLACEMENT_3D('',#8886,#7822,#7823);
#7378=AXIS2_PLACEMENT_3D('',#8888,#7824,#7825);
#7379=AXIS2_PLACEMENT_3D('',#8891,#7827,#7828);
#7380=AXIS2_PLACEMENT_3D('',#8892,#7829,#7830);
#7381=AXIS2_PLACEMENT_3D('',#8894,#7831,#7832);
#7382=AXIS2_PLACEMENT_3D('',#8897,#7834,#7835);
#7383=AXIS2_PLACEMENT_3D('',#8898,#7836,#7837);
#7384=AXIS2_PLACEMENT_3D('',#8907,#7842,#7843);
#7385=AXIS2_PLACEMENT_3D('',#8913,#7847,#7848);
#7386=AXIS2_PLACEMENT_3D('',#8919,#7852,#7853);
#7387=AXIS2_PLACEMENT_3D('',#8922,#7856,#7857);
#7388=AXIS2_PLACEMENT_3D('',#8923,#7858,#7859);
#7389=AXIS2_PLACEMENT_3D('',#8924,#7860,#7861);
#7390=AXIS2_PLACEMENT_3D('',#8925,#7862,#7863);
#7391=AXIS2_PLACEMENT_3D('',#8927,#7864,#7865);
#7392=AXIS2_PLACEMENT_3D('',#8930,#7867,#7868);
#7393=AXIS2_PLACEMENT_3D('',#8931,#7869,#7870);
#7394=AXIS2_PLACEMENT_3D('',#8933,#7871,#7872);
#7395=AXIS2_PLACEMENT_3D('',#8936,#7874,#7875);
#7396=AXIS2_PLACEMENT_3D('',#8937,#7876,#7877);
#7397=AXIS2_PLACEMENT_3D('',#8938,#7878,#7879);
#7398=AXIS2_PLACEMENT_3D('',#8939,#7880,#7881);
#7399=AXIS2_PLACEMENT_3D('',#8940,#7882,#7883);
#7400=AXIS2_PLACEMENT_3D('',#9079,#7885,#7886);
#7401=AXIS2_PLACEMENT_3D('',#9156,#7887,#7888);
#7402=AXIS2_PLACEMENT_3D('',#9652,#7890,#7891);
#7403=AXIS2_PLACEMENT_3D('',#10154,#7893,#7894);
#7404=AXIS2_PLACEMENT_3D('',#10665,#7896,#7897);
#7405=AXIS2_PLACEMENT_3D('',#11158,#7899,#7900);
#7406=AXIS2_PLACEMENT_3D('',#11651,#7902,#7903);
#7407=AXIS2_PLACEMENT_3D('',#12150,#7905,#7906);
#7408=AXIS2_PLACEMENT_3D('',#12649,#7908,#7909);
#7409=AXIS2_PLACEMENT_3D('',#13139,#7911,#7912);
#7410=AXIS2_PLACEMENT_3D('',#13626,#7914,#7915);
#7411=AXIS2_PLACEMENT_3D('',#14131,#7917,#7918);
#7412=AXIS2_PLACEMENT_3D('',#14636,#7920,#7921);
#7413=AXIS2_PLACEMENT_3D('',#15138,#7923,#7924);
#7414=AXIS2_PLACEMENT_3D('',#15634,#7926,#7927);
#7415=AXIS2_PLACEMENT_3D('',#16127,#7929,#7930);
#7416=AXIS2_PLACEMENT_3D('',#16617,#7932,#7933);
#7417=AXIS2_PLACEMENT_3D('',#17119,#7935,#7936);
#7418=AXIS2_PLACEMENT_3D('',#17633,#7938,#7939);
#7419=AXIS2_PLACEMENT_3D('',#18132,#7941,#7942);
#7420=AXIS2_PLACEMENT_3D('',#18619,#7944,#7945);
#7421=AXIS2_PLACEMENT_3D('',#19112,#7947,#7948);
#7422=AXIS2_PLACEMENT_3D('',#19620,#7950,#7951);
#7423=AXIS2_PLACEMENT_3D('',#20119,#7953,#7954);
#7424=AXIS2_PLACEMENT_3D('',#20621,#7956,#7957);
#7425=AXIS2_PLACEMENT_3D('',#21108,#7959,#7960);
#7426=AXIS2_PLACEMENT_3D('',#21592,#7962,#7963);
#7427=AXIS2_PLACEMENT_3D('',#22094,#7965,#7966);
#7428=AXIS2_PLACEMENT_3D('',#22602,#7968,#7969);
#7429=AXIS2_PLACEMENT_3D('',#23110,#7971,#7972);
#7430=AXIS2_PLACEMENT_3D('',#23594,#7974,#7975);
#7431=AXIS2_PLACEMENT_3D('',#24087,#7977,#7978);
#7432=AXIS2_PLACEMENT_3D('',#24598,#7980,#7981);
#7433=AXIS2_PLACEMENT_3D('',#25109,#7983,#7984);
#7434=AXIS2_PLACEMENT_3D('',#25605,#7986,#7987);
#7435=AXIS2_PLACEMENT_3D('',#26086,#7989,#7990);
#7436=AXIS2_PLACEMENT_3D('',#26585,#7992,#7993);
#7437=AXIS2_PLACEMENT_3D('',#27084,#7995,#7996);
#7438=AXIS2_PLACEMENT_3D('',#27580,#7998,#7999);
#7439=AXIS2_PLACEMENT_3D('',#28097,#8001,#8002);
#7440=AXIS2_PLACEMENT_3D('',#28581,#8004,#8005);
#7441=AXIS2_PLACEMENT_3D('',#29074,#8007,#8008);
#7442=AXIS2_PLACEMENT_3D('',#29576,#8010,#8011);
#7443=AXIS2_PLACEMENT_3D('',#30075,#8013,#8014);
#7444=AXIS2_PLACEMENT_3D('',#30562,#8016,#8017);
#7445=AXIS2_PLACEMENT_3D('',#30895,#8019,#8020);
#7446=AXIS2_PLACEMENT_3D('',#31333,#8022,#8023);
#7447=AXIS2_PLACEMENT_3D('',#31829,#8025,#8026);
#7448=AXIS2_PLACEMENT_3D('',#32331,#8028,#8029);
#7449=AXIS2_PLACEMENT_3D('',#32833,#8031,#8032);
#7450=AXIS2_PLACEMENT_3D('',#33335,#8034,#8035);
#7451=AXIS2_PLACEMENT_3D('',#33831,#8037,#8038);
#7452=AXIS2_PLACEMENT_3D('',#34333,#8040,#8041);
#7453=AXIS2_PLACEMENT_3D('',#34835,#8043,#8044);
#7454=AXIS2_PLACEMENT_3D('',#35322,#8046,#8047);
#7455=AXIS2_PLACEMENT_3D('',#35827,#8049,#8050);
#7456=AXIS2_PLACEMENT_3D('',#36329,#8052,#8053);
#7457=AXIS2_PLACEMENT_3D('',#36819,#8055,#8056);
#7458=AXIS2_PLACEMENT_3D('',#37306,#8058,#8059);
#7459=AXIS2_PLACEMENT_3D('',#37808,#8061,#8062);
#7460=AXIS2_PLACEMENT_3D('',#38319,#8064,#8065);
#7461=AXIS2_PLACEMENT_3D('',#38815,#8067,#8068);
#7462=AXIS2_PLACEMENT_3D('',#39305,#8070,#8071);
#7463=AXIS2_PLACEMENT_3D('',#39795,#8073,#8074);
#7464=AXIS2_PLACEMENT_3D('',#40294,#8076,#8077);
#7465=AXIS2_PLACEMENT_3D('',#40793,#8079,#8080);
#7466=AXIS2_PLACEMENT_3D('',#41286,#8082,#8083);
#7467=AXIS2_PLACEMENT_3D('',#41779,#8085,#8086);
#7468=AXIS2_PLACEMENT_3D('',#42284,#8088,#8089);
#7469=AXIS2_PLACEMENT_3D('',#42777,#8091,#8092);
#7470=AXIS2_PLACEMENT_3D('',#43285,#8094,#8095);
#7471=AXIS2_PLACEMENT_3D('',#43784,#8097,#8098);
#7472=AXIS2_PLACEMENT_3D('',#44271,#8100,#8101);
#7473=AXIS2_PLACEMENT_3D('',#44770,#8103,#8104);
#7474=AXIS2_PLACEMENT_3D('',#45266,#8106,#8107);
#7475=AXIS2_PLACEMENT_3D('',#45768,#8109,#8110);
#7476=AXIS2_PLACEMENT_3D('',#46270,#8112,#8113);
#7477=AXIS2_PLACEMENT_3D('',#46775,#8115,#8116);
#7478=AXIS2_PLACEMENT_3D('',#46943,#8117,#8118);
#7479=AXIS2_PLACEMENT_3D('',#47064,#8119,#8120);
#7480=AXIS2_PLACEMENT_3D('',#47076,#8121,#8122);
#7481=AXIS2_PLACEMENT_3D('',#53093,#8123,#8124);
#7482=AXIS2_PLACEMENT_3D('',#66980,#8125,#8126);
#7483=AXIS2_PLACEMENT_3D('',#66982,#8127,#8128);
#7484=AXIS2_PLACEMENT_3D('',#66985,#8130,#8131);
#7485=AXIS2_PLACEMENT_3D('',#66986,#8132,#8133);
#7486=AXIS2_PLACEMENT_3D('',#66988,#8134,#8135);
#7487=AXIS2_PLACEMENT_3D('',#66989,#8136,#8137);
#7488=AXIS2_PLACEMENT_3D('',#66991,#8138,#8139);
#7489=AXIS2_PLACEMENT_3D('',#66992,#8140,#8141);
#7490=AXIS2_PLACEMENT_3D('',#66994,#8142,#8143);
#7491=AXIS2_PLACEMENT_3D('',#66996,#8145,#8146);
#7492=AXIS2_PLACEMENT_3D('',#66999,#8148,#8149);
#7493=AXIS2_PLACEMENT_3D('',#67000,#8150,#8151);
#7494=AXIS2_PLACEMENT_3D('',#67001,#8152,#8153);
#7495=AXIS2_PLACEMENT_3D('',#67003,#8154,#8155);
#7496=AXIS2_PLACEMENT_3D('',#67006,#8156,#8157);
#7497=AXIS2_PLACEMENT_3D('',#67007,#8158,#8159);
#7498=AXIS2_PLACEMENT_3D('',#67008,#8160,#8161);
#7499=AXIS2_PLACEMENT_3D('',#67009,#8162,#8163);
#7500=AXIS2_PLACEMENT_3D('',#67011,#8164,#8165);
#7501=AXIS2_PLACEMENT_3D('',#67013,#8167,#8168);
#7502=AXIS2_PLACEMENT_3D('',#67014,#8169,#8170);
#7503=AXIS2_PLACEMENT_3D('',#67016,#8171,#8172);
#7504=AXIS2_PLACEMENT_3D('',#67019,#8174,#8175);
#7505=AXIS2_PLACEMENT_3D('',#67020,#8176,#8177);
#7506=AXIS2_PLACEMENT_3D('',#67022,#8178,#8179);
#7507=AXIS2_PLACEMENT_3D('',#67025,#8181,#8182);
#7508=AXIS2_PLACEMENT_3D('',#67026,#8183,#8184);
#7509=AXIS2_PLACEMENT_3D('',#67028,#8185,#8186);
#7510=AXIS2_PLACEMENT_3D('',#67031,#8188,#8189);
#7511=AXIS2_PLACEMENT_3D('',#67032,#8190,#8191);
#7512=AXIS2_PLACEMENT_3D('',#67034,#8192,#8193);
#7513=AXIS2_PLACEMENT_3D('',#67037,#8195,#8196);
#7514=AXIS2_PLACEMENT_3D('',#67038,#8197,#8198);
#7515=AXIS2_PLACEMENT_3D('',#71825,#8199,#8200);
#7516=AXIS2_PLACEMENT_3D('',#71834,#8205,#8206);
#7517=AXIS2_PLACEMENT_3D('',#71840,#8210,#8211);
#7518=AXIS2_PLACEMENT_3D('',#71846,#8215,#8216);
#7519=AXIS2_PLACEMENT_3D('',#71852,#8220,#8221);
#7520=AXIS2_PLACEMENT_3D('',#71858,#8225,#8226);
#7521=AXIS2_PLACEMENT_3D('',#71861,#8229,#8230);
#7522=AXIS2_PLACEMENT_3D('',#71862,#8231,#8232);
#7523=AXIS2_PLACEMENT_3D('',#71864,#8233,#8234);
#7524=AXIS2_PLACEMENT_3D('',#71865,#8235,#8236);
#7525=AXIS2_PLACEMENT_3D('',#71868,#8238,#8239);
#7526=AXIS2_PLACEMENT_3D('',#71869,#8240,#8241);
#7527=AXIS2_PLACEMENT_3D('',#71870,#8242,#8243);
#7528=AXIS2_PLACEMENT_3D('',#71871,#8244,#8245);
#7529=AXIS2_PLACEMENT_3D('',#71880,#8250,#8251);
#7530=AXIS2_PLACEMENT_3D('',#71889,#8256,#8257);
#7531=AXIS2_PLACEMENT_3D('',#71890,#8258,#8259);
#7532=AXIS2_PLACEMENT_3D('',#71891,#8260,#8261);
#7533=AXIS2_PLACEMENT_3D('',#71892,#8262,#8263);
#7534=AXIS2_PLACEMENT_3D('',#71893,#8264,#8265);
#7535=AXIS2_PLACEMENT_3D('',#71894,#8266,#8267);
#7536=AXIS2_PLACEMENT_3D('',#71895,#8268,#8269);
#7537=AXIS2_PLACEMENT_3D('',#71896,#8270,#8271);
#7538=AXIS2_PLACEMENT_3D('',#71897,#8272,#8273);
#7539=AXIS2_PLACEMENT_3D('',#71898,#8274,#8275);
#7540=AXIS2_PLACEMENT_3D('',#71912,#8277,#8278);
#7541=AXIS2_PLACEMENT_3D('',#71922,#8279,#8280);
#7542=AXIS2_PLACEMENT_3D('',#72292,#8282,#8283);
#7543=AXIS2_PLACEMENT_3D('',#72510,#8285,#8286);
#7544=AXIS2_PLACEMENT_3D('',#72878,#8288,#8289);
#7545=AXIS2_PLACEMENT_3D('',#73419,#8291,#8292);
#7546=AXIS2_PLACEMENT_3D('',#73960,#8294,#8295);
#7547=AXIS2_PLACEMENT_3D('',#74342,#8297,#8298);
#7548=AXIS2_PLACEMENT_3D('',#74794,#8300,#8301);
#7549=AXIS2_PLACEMENT_3D('',#75178,#8303,#8304);
#7550=AXIS2_PLACEMENT_3D('',#75200,#8306,#8307);
#7551=AXIS2_PLACEMENT_3D('',#75218,#8308,#8309);
#7552=AXIS2_PLACEMENT_3D('',#75232,#8311,#8312);
#7553=AXIS2_PLACEMENT_3D('',#75277,#8313,#8314);
#7554=AXIS2_PLACEMENT_3D('',#75529,#8316,#8317);
#7555=AXIS2_PLACEMENT_3D('',#75824,#8319,#8320);
#7556=AXIS2_PLACEMENT_3D('',#76213,#8322,#8323);
#7557=AXIS2_PLACEMENT_3D('',#76471,#8325,#8326);
#7558=AXIS2_PLACEMENT_3D('',#76618,#8328,#8329);
#7559=AXIS2_PLACEMENT_3D('',#77012,#8331,#8332);
#7560=AXIS2_PLACEMENT_3D('',#77169,#8334,#8335);
#7561=AXIS2_PLACEMENT_3D('',#77551,#8337,#8338);
#7562=AXIS2_PLACEMENT_3D('',#77635,#8340,#8341);
#7563=AXIS2_PLACEMENT_3D('',#77882,#8342,#8343);
#7564=AXIS2_PLACEMENT_3D('',#78143,#8344,#8345);
#7565=AXIS2_PLACEMENT_3D('',#78272,#8346,#8347);
#7566=AXIS2_PLACEMENT_3D('',#78274,#8348,#8349);
#7567=AXIS2_PLACEMENT_3D('',#78277,#8351,#8352);
#7568=AXIS2_PLACEMENT_3D('',#78278,#8353,#8354);
#7569=AXIS2_PLACEMENT_3D('',#78280,#8355,#8356);
#7570=AXIS2_PLACEMENT_3D('',#78283,#8358,#8359);
#7571=AXIS2_PLACEMENT_3D('',#79804,#8360,#8361);
#7572=AXIS2_PLACEMENT_3D('',#79814,#8366,#8367);
#7573=AXIS2_PLACEMENT_3D('',#79816,#8368,#8369);
#7574=AXIS2_PLACEMENT_3D('',#79817,#8370,#8371);
#7575=AXIS2_PLACEMENT_3D('',#79820,#8373,#8374);
#7576=AXIS2_PLACEMENT_3D('',#79821,#8375,#8376);
#7577=AXIS2_PLACEMENT_3D('',#79824,#8378,#8379);
#7578=AXIS2_PLACEMENT_3D('',#79825,#8380,#8381);
#7579=AXIS2_PLACEMENT_3D('',#79831,#8385,#8386);
#7580=AXIS2_PLACEMENT_3D('',#79835,#8389,#8390);
#7581=AXIS2_PLACEMENT_3D('',#79839,#8393,#8394);
#7582=AXIS2_PLACEMENT_3D('',#79841,#8396,#8397);
#7583=AXIS2_PLACEMENT_3D('',#79842,#8398,#8399);
#7584=AXIS2_PLACEMENT_3D('',#79843,#8400,#8401);
#7585=AXIS2_PLACEMENT_3D('',#79855,#8403,#8404);
#7586=AXIS2_PLACEMENT_3D('',#79950,#8405,#8406);
#7587=AXIS2_PLACEMENT_3D('',#80316,#8408,#8409);
#7588=AXIS2_PLACEMENT_3D('',#80618,#8411,#8412);
#7589=AXIS2_PLACEMENT_3D('',#80982,#8414,#8415);
#7590=AXIS2_PLACEMENT_3D('',#81287,#8417,#8418);
#7591=AXIS2_PLACEMENT_3D('',#81375,#8420,#8421);
#7592=AXIS2_PLACEMENT_3D('',#81448,#8422,#8423);
#7593=AXIS2_PLACEMENT_3D('',#81460,#8425,#8426);
#7594=AXIS2_PLACEMENT_3D('',#81555,#8427,#8428);
#7595=AXIS2_PLACEMENT_3D('',#81921,#8430,#8431);
#7596=AXIS2_PLACEMENT_3D('',#82223,#8433,#8434);
#7597=AXIS2_PLACEMENT_3D('',#82587,#8436,#8437);
#7598=AXIS2_PLACEMENT_3D('',#82892,#8439,#8440);
#7599=AXIS2_PLACEMENT_3D('',#82980,#8442,#8443);
#7600=AXIS2_PLACEMENT_3D('',#83053,#8444,#8445);
#7601=AXIS2_PLACEMENT_3D('',#83069,#8447,#8448);
#7602=AXIS2_PLACEMENT_3D('',#83126,#8449,#8450);
#7603=AXIS2_PLACEMENT_3D('',#83478,#8452,#8453);
#7604=AXIS2_PLACEMENT_3D('',#83844,#8455,#8456);
#7605=AXIS2_PLACEMENT_3D('',#84032,#8458,#8459);
#7606=AXIS2_PLACEMENT_3D('',#84243,#8461,#8462);
#7607=AXIS2_PLACEMENT_3D('',#84381,#8464,#8465);
#7608=AXIS2_PLACEMENT_3D('',#84568,#8466,#8467);
#7609=AXIS2_PLACEMENT_3D('',#84584,#8469,#8470);
#7610=AXIS2_PLACEMENT_3D('',#84641,#8471,#8472);
#7611=AXIS2_PLACEMENT_3D('',#84993,#8474,#8475);
#7612=AXIS2_PLACEMENT_3D('',#85361,#8477,#8478);
#7613=AXIS2_PLACEMENT_3D('',#85549,#8480,#8481);
#7614=AXIS2_PLACEMENT_3D('',#85760,#8483,#8484);
#7615=AXIS2_PLACEMENT_3D('',#85898,#8486,#8487);
#7616=AXIS2_PLACEMENT_3D('',#86085,#8488,#8489);
#7617=AXIS2_PLACEMENT_3D('',#86470,#8490,#8491);
#7618=AXIS2_PLACEMENT_3D('',#86855,#8492,#8493);
#7619=AXIS2_PLACEMENT_3D('',#87084,#8494,#8495);
#7620=AXIS2_PLACEMENT_3D('',#88020,#8496,#8497);
#7621=AXIS2_PLACEMENT_3D('',#88212,#8502,#8503);
#7622=AXIS2_PLACEMENT_3D('',#88744,#8504,#8505);
#7623=AXIS2_PLACEMENT_3D('',#88747,#8507,#8508);
#7624=AXIS2_PLACEMENT_3D('',#88748,#8509,#8510);
#7625=AXIS2_PLACEMENT_3D('',#88754,#8514,#8515);
#7626=AXIS2_PLACEMENT_3D('',#88758,#8518,#8519);
#7627=AXIS2_PLACEMENT_3D('',#88762,#8522,#8523);
#7628=AXIS2_PLACEMENT_3D('',#88764,#8525,#8526);
#7629=AXIS2_PLACEMENT_3D('',#88765,#8527,#8528);
#7630=AXIS2_PLACEMENT_3D('',#88766,#8529,#8530);
#7631=AXIS2_PLACEMENT_3D('',#88768,#8531,#8532);
#7632=AXIS2_PLACEMENT_3D('',#88771,#8534,#8535);
#7633=AXIS2_PLACEMENT_3D('',#88772,#8536,#8537);
#7634=AXIS2_PLACEMENT_3D('',#88774,#8538,#8539);
#7635=AXIS2_PLACEMENT_3D('',#88775,#8540,#8541);
#7636=AXIS2_PLACEMENT_3D('',#88777,#8542,#8543);
#7637=AXIS2_PLACEMENT_3D('',#88778,#8544,#8545);
#7638=AXIS2_PLACEMENT_3D('',#88780,#8546,#8547);
#7639=AXIS2_PLACEMENT_3D('',#88782,#8549,#8550);
#7640=AXIS2_PLACEMENT_3D('',#88784,#8551,#8552);
#7641=AXIS2_PLACEMENT_3D('',#88786,#8553,#8554);
#7642=AXIS2_PLACEMENT_3D('',#88787,#8555,#8556);
#7643=AXIS2_PLACEMENT_3D('',#88790,#8558,#8559);
#7644=AXIS2_PLACEMENT_3D('',#88791,#8560,#8561);
#7645=AXIS2_PLACEMENT_3D('',#88792,#8562,#8563);
#7646=AXIS2_PLACEMENT_3D('',#88794,#8565,#8566);
#7647=AXIS2_PLACEMENT_3D('',#88795,#8567,#8568);
#7648=AXIS2_PLACEMENT_3D('',#88796,#8569,#8570);
#7649=AXIS2_PLACEMENT_3D('',#88805,#8575,#8576);
#7650=AXIS2_PLACEMENT_3D('',#88814,#8581,#8582);
#7651=AXIS2_PLACEMENT_3D('',#88815,#8583,#8584);
#7652=AXIS2_PLACEMENT_3D('',#88816,#8585,#8586);
#7653=AXIS2_PLACEMENT_3D('',#88817,#8587,#8588);
#7654=AXIS2_PLACEMENT_3D('',#88818,#8589,#8590);
#7655=AXIS2_PLACEMENT_3D('',#88819,#8591,#8592);
#7656=AXIS2_PLACEMENT_3D('',#88820,#8593,#8594);
#7657=AXIS2_PLACEMENT_3D('',#88821,#8595,#8596);
#7658=AXIS2_PLACEMENT_3D('',#88822,#8597,#8598);
#7659=AXIS2_PLACEMENT_3D('',#88823,#8599,#8600);
#7660=AXIS2_PLACEMENT_3D('',#88825,#8601,#8602);
#7661=AXIS2_PLACEMENT_3D('',#88828,#8604,#8605);
#7662=AXIS2_PLACEMENT_3D('',#88829,#8606,#8607);
#7663=AXIS2_PLACEMENT_3D('',#88831,#8608,#8609);
#7664=AXIS2_PLACEMENT_3D('',#88834,#8611,#8612);
#7665=AXIS2_PLACEMENT_3D('',#88835,#8613,#8614);
#7666=AXIS2_PLACEMENT_3D('',#88836,#8615,#8616);
#7667=AXIS2_PLACEMENT_3D('',#88837,#8617,#8618);
#7668=AXIS2_PLACEMENT_3D('',#88838,#8619,#8620);
#7669=AXIS2_PLACEMENT_3D('',#88840,#8621,#8622);
#7670=AXIS2_PLACEMENT_3D('',#88843,#8624,#8625);
#7671=AXIS2_PLACEMENT_3D('',#88844,#8626,#8627);
#7672=AXIS2_PLACEMENT_3D('',#88846,#8628,#8629);
#7673=AXIS2_PLACEMENT_3D('',#88849,#8631,#8632);
#7674=AXIS2_PLACEMENT_3D('',#88850,#8633,#8634);
#7675=AXIS2_PLACEMENT_3D('',#88851,#8635,#8636);
#7676=AXIS2_PLACEMENT_3D('',#88852,#8637,#8638);
#7677=AXIS2_PLACEMENT_3D('',#88853,#8639,#8640);
#7678=AXIS2_PLACEMENT_3D('',#89029,#8642,#8643);
#7679=AXIS2_PLACEMENT_3D('',#89154,#8644,#8645);
#7680=AXIS2_PLACEMENT_3D('',#89619,#8647,#8648);
#7681=AXIS2_PLACEMENT_3D('',#90042,#8650,#8651);
#7682=AXIS2_PLACEMENT_3D('',#90285,#8653,#8654);
#7683=AXIS2_PLACEMENT_3D('',#90525,#8656,#8657);
#7684=AXIS2_PLACEMENT_3D('',#90929,#8659,#8660);
#7685=AXIS2_PLACEMENT_3D('',#91459,#8662,#8663);
#7686=AXIS2_PLACEMENT_3D('',#91977,#8665,#8666);
#7687=AXIS2_PLACEMENT_3D('',#92423,#8668,#8669);
#7688=AXIS2_PLACEMENT_3D('',#92865,#8671,#8672);
#7689=AXIS2_PLACEMENT_3D('',#92911,#8674,#8675);
#7690=AXIS2_PLACEMENT_3D('',#93376,#8677,#8678);
#7691=AXIS2_PLACEMENT_3D('',#93851,#8680,#8681);
#7692=AXIS2_PLACEMENT_3D('',#94298,#8683,#8684);
#7693=AXIS2_PLACEMENT_3D('',#94747,#8686,#8687);
#7694=AXIS2_PLACEMENT_3D('',#95198,#8689,#8690);
#7695=AXIS2_PLACEMENT_3D('',#95627,#8692,#8693);
#7696=AXIS2_PLACEMENT_3D('',#95899,#8695,#8696);
#7697=AXIS2_PLACEMENT_3D('',#96343,#8698,#8699);
#7698=AXIS2_PLACEMENT_3D('',#96811,#8701,#8702);
#7699=AXIS2_PLACEMENT_3D('',#97257,#8704,#8705);
#7700=AXIS2_PLACEMENT_3D('',#97683,#8707,#8708);
#7701=AXIS2_PLACEMENT_3D('',#98149,#8710,#8711);
#7702=AXIS2_PLACEMENT_3D('',#98675,#8713,#8714);
#7703=AXIS2_PLACEMENT_3D('',#98685,#8715,#8716);
#7704=AXIS2_PLACEMENT_3D('',#101181,#8717,#8718);
#7705=AXIS2_PLACEMENT_3D('',#103771,#8719,#8720);
#7706=AXIS2_PLACEMENT_3D('',#103963,#8721,#8722);
#7707=AXIS2_PLACEMENT_3D('',#104119,#8723,#8724);
#7708=AXIS2_PLACEMENT_3D('',#104255,#8726,#8727);
#7709=AXIS2_PLACEMENT_3D('',#105712,#8728,#8729);
#7710=AXIS2_PLACEMENT_3D('',#105721,#8734,#8735);
#7711=AXIS2_PLACEMENT_3D('',#105727,#8739,#8740);
#7712=AXIS2_PLACEMENT_3D('',#105733,#8744,#8745);
#7713=AXIS2_PLACEMENT_3D('',#105739,#8749,#8750);
#7714=AXIS2_PLACEMENT_3D('',#105745,#8754,#8755);
#7715=AXIS2_PLACEMENT_3D('',#105748,#8758,#8759);
#7716=AXIS2_PLACEMENT_3D('',#105749,#8760,#8761);
#7717=AXIS2_PLACEMENT_3D('',#105751,#8762,#8763);
#7718=AXIS2_PLACEMENT_3D('',#105752,#8764,#8765);
#7719=AXIS2_PLACEMENT_3D('',#105755,#8767,#8768);
#7720=AXIS2_PLACEMENT_3D('',#105756,#8769,#8770);
#7721=AXIS2_PLACEMENT_3D('',#105757,#8771,#8772);
#7722=AXIS2_PLACEMENT_3D('',#105758,#8773,#8774);
#7723=AXIS2_PLACEMENT_3D('',#105759,#8775,#8776);
#7724=AXIS2_PLACEMENT_3D('',#105760,#8777,#8778);
#7725=AXIS2_PLACEMENT_3D('',#105761,#8779,#8780);
#7726=AXIS2_PLACEMENT_3D('',#105762,#8781,#8782);
#7727=AXIS2_PLACEMENT_3D('',#105763,#8783,#8784);
#7728=AXIS2_PLACEMENT_3D('',#105764,#8785,#8786);
#7729=AXIS2_PLACEMENT_3D('',#105765,#8787,#8788);
#7730=AXIS2_PLACEMENT_3D('',#105766,#8789,#8790);
#7731=AXIS2_PLACEMENT_3D('',#105767,#8791,#8792);
#7732=AXIS2_PLACEMENT_3D('',#105768,#8793,#8794);
#7733=AXIS2_PLACEMENT_3D('',#105769,#8795,#8796);
#7734=AXIS2_PLACEMENT_3D('',#105770,#8797,#8798);
#7735=AXIS2_PLACEMENT_3D('',#105771,#8799,#8800);
#7736=AXIS2_PLACEMENT_3D('',#105772,#8801,#8802);
#7737=AXIS2_PLACEMENT_3D('',#105773,#8803,#8804);
#7738=AXIS2_PLACEMENT_3D('',#105774,#8805,#8806);
#7739=AXIS2_PLACEMENT_3D('',#105775,#8807,#8808);
#7740=AXIS2_PLACEMENT_3D('',#105776,#8809,#8810);
#7741=AXIS2_PLACEMENT_3D('',#105777,#8811,#8812);
#7742=AXIS2_PLACEMENT_3D('',#105778,#8813,#8814);
#7743=DIRECTION('axis',(0.,0.,1.));
#7744=DIRECTION('refdir',(1.,0.,0.));
#7745=DIRECTION('axis',(0.,0.,1.));
#7746=DIRECTION('refdir',(1.,0.,0.));
#7747=DIRECTION('center_axis',(0.,0.,-1.));
#7748=DIRECTION('ref_axis',(1.,0.,0.));
#7749=DIRECTION('center_axis',(0.,0.,-1.));
#7750=DIRECTION('ref_axis',(1.,0.,0.));
#7751=DIRECTION('',(0.,0.,-1.));
#7752=DIRECTION('center_axis',(0.,0.,1.));
#7753=DIRECTION('ref_axis',(1.,0.,0.));
#7754=DIRECTION('center_axis',(0.,0.,-1.));
#7755=DIRECTION('ref_axis',(1.,0.,0.));
#7756=DIRECTION('center_axis',(0.,0.,-1.));
#7757=DIRECTION('ref_axis',(1.,0.,0.));
#7758=DIRECTION('',(0.,0.,-1.));
#7759=DIRECTION('center_axis',(0.,0.,1.));
#7760=DIRECTION('ref_axis',(1.,0.,0.));
#7761=DIRECTION('center_axis',(0.,0.,-1.));
#7762=DIRECTION('ref_axis',(1.,0.,0.));
#7763=DIRECTION('center_axis',(0.,0.,-1.));
#7764=DIRECTION('ref_axis',(1.,0.,0.));
#7765=DIRECTION('',(0.,0.,-1.));
#7766=DIRECTION('center_axis',(0.,0.,1.));
#7767=DIRECTION('ref_axis',(1.,0.,0.));
#7768=DIRECTION('center_axis',(0.,0.,-1.));
#7769=DIRECTION('ref_axis',(1.,0.,0.));
#7770=DIRECTION('center_axis',(0.,0.,-1.));
#7771=DIRECTION('ref_axis',(1.,0.,0.));
#7772=DIRECTION('',(0.,0.,-1.));
#7773=DIRECTION('center_axis',(0.,0.,1.));
#7774=DIRECTION('ref_axis',(1.,0.,0.));
#7775=DIRECTION('center_axis',(0.,1.,0.));
#7776=DIRECTION('ref_axis',(-1.,0.,0.));
#7777=DIRECTION('',(1.,0.,0.));
#7778=DIRECTION('',(0.,0.,1.));
#7779=DIRECTION('',(1.,0.,0.));
#7780=DIRECTION('',(0.,0.,-1.));
#7781=DIRECTION('center_axis',(1.,0.,0.));
#7782=DIRECTION('ref_axis',(0.,1.,0.));
#7783=DIRECTION('',(0.,-1.,0.));
#7784=DIRECTION('',(0.,-1.,0.));
#7785=DIRECTION('',(0.,0.,-1.));
#7786=DIRECTION('center_axis',(0.,-1.,0.));
#7787=DIRECTION('ref_axis',(1.,0.,0.));
#7788=DIRECTION('',(-1.,0.,0.));
#7789=DIRECTION('',(-1.,0.,0.));
#7790=DIRECTION('',(0.,0.,1.));
#7791=DIRECTION('center_axis',(-1.,0.,0.));
#7792=DIRECTION('ref_axis',(0.,-1.,0.));
#7793=DIRECTION('',(0.,1.,0.));
#7794=DIRECTION('',(0.,1.,0.));
#7795=DIRECTION('center_axis',(0.,0.,1.));
#7796=DIRECTION('ref_axis',(1.,0.,0.));
#7797=DIRECTION('center_axis',(0.,0.,1.));
#7798=DIRECTION('ref_axis',(1.,0.,0.));
#7799=DIRECTION('axis',(0.,0.,1.));
#7800=DIRECTION('refdir',(1.,0.,0.));
#7801=DIRECTION('center_axis',(0.,0.,-1.));
#7802=DIRECTION('ref_axis',(1.,0.,0.));
#7803=DIRECTION('center_axis',(0.,0.,-1.));
#7804=DIRECTION('ref_axis',(1.,0.,0.));
#7805=DIRECTION('',(0.,0.,-1.));
#7806=DIRECTION('center_axis',(0.,0.,1.));
#7807=DIRECTION('ref_axis',(1.,0.,0.));
#7808=DIRECTION('center_axis',(0.,0.,-1.));
#7809=DIRECTION('ref_axis',(1.,0.,0.));
#7810=DIRECTION('center_axis',(0.,0.,-1.));
#7811=DIRECTION('ref_axis',(1.,0.,0.));
#7812=DIRECTION('',(0.,0.,-1.));
#7813=DIRECTION('center_axis',(0.,0.,1.));
#7814=DIRECTION('ref_axis',(1.,0.,0.));
#7815=DIRECTION('center_axis',(0.,0.,-1.));
#7816=DIRECTION('ref_axis',(1.,0.,0.));
#7817=DIRECTION('center_axis',(0.,0.,-1.));
#7818=DIRECTION('ref_axis',(1.,0.,0.));
#7819=DIRECTION('',(0.,0.,-1.));
#7820=DIRECTION('center_axis',(0.,0.,1.));
#7821=DIRECTION('ref_axis',(1.,0.,0.));
#7822=DIRECTION('center_axis',(0.,0.,-1.));
#7823=DIRECTION('ref_axis',(1.,0.,0.));
#7824=DIRECTION('center_axis',(0.,0.,-1.));
#7825=DIRECTION('ref_axis',(1.,0.,0.));
#7826=DIRECTION('',(0.,0.,-1.));
#7827=DIRECTION('center_axis',(0.,0.,1.));
#7828=DIRECTION('ref_axis',(1.,0.,0.));
#7829=DIRECTION('center_axis',(0.,0.,-1.));
#7830=DIRECTION('ref_axis',(1.,0.,0.));
#7831=DIRECTION('center_axis',(0.,0.,-1.));
#7832=DIRECTION('ref_axis',(1.,0.,0.));
#7833=DIRECTION('',(0.,0.,-1.));
#7834=DIRECTION('center_axis',(0.,0.,1.));
#7835=DIRECTION('ref_axis',(1.,0.,0.));
#7836=DIRECTION('center_axis',(0.,1.,0.));
#7837=DIRECTION('ref_axis',(-1.,0.,0.));
#7838=DIRECTION('',(1.,0.,0.));
#7839=DIRECTION('',(0.,0.,1.));
#7840=DIRECTION('',(1.,0.,0.));
#7841=DIRECTION('',(0.,0.,-1.));
#7842=DIRECTION('center_axis',(1.,0.,0.));
#7843=DIRECTION('ref_axis',(0.,1.,0.));
#7844=DIRECTION('',(0.,1.,0.));
#7845=DIRECTION('',(0.,1.,0.));
#7846=DIRECTION('',(0.,0.,1.));
#7847=DIRECTION('center_axis',(0.,-1.,0.));
#7848=DIRECTION('ref_axis',(1.,0.,0.));
#7849=DIRECTION('',(1.,0.,0.));
#7850=DIRECTION('',(1.,0.,0.));
#7851=DIRECTION('',(0.,0.,1.));
#7852=DIRECTION('center_axis',(-1.,0.,0.));
#7853=DIRECTION('ref_axis',(0.,-1.,0.));
#7854=DIRECTION('',(0.,-1.,0.));
#7855=DIRECTION('',(0.,-1.,0.));
#7856=DIRECTION('center_axis',(0.,0.,1.));
#7857=DIRECTION('ref_axis',(1.,0.,0.));
#7858=DIRECTION('center_axis',(0.,0.,1.));
#7859=DIRECTION('ref_axis',(1.,0.,0.));
#7860=DIRECTION('axis',(0.,0.,1.));
#7861=DIRECTION('refdir',(1.,0.,0.));
#7862=DIRECTION('center_axis',(0.,0.,1.));
#7863=DIRECTION('ref_axis',(1.,0.,0.));
#7864=DIRECTION('center_axis',(0.,0.,-1.));
#7865=DIRECTION('ref_axis',(1.,0.,0.));
#7866=DIRECTION('',(0.,0.,1.));
#7867=DIRECTION('center_axis',(0.,0.,-1.));
#7868=DIRECTION('ref_axis',(1.,0.,0.));
#7869=DIRECTION('center_axis',(0.,0.,1.));
#7870=DIRECTION('ref_axis',(1.,0.,0.));
#7871=DIRECTION('center_axis',(0.,0.,1.));
#7872=DIRECTION('ref_axis',(1.,0.,0.));
#7873=DIRECTION('',(0.,0.,-1.));
#7874=DIRECTION('center_axis',(0.,0.,1.));
#7875=DIRECTION('ref_axis',(1.,0.,0.));
#7876=DIRECTION('center_axis',(0.,0.,1.));
#7877=DIRECTION('ref_axis',(1.,0.,0.));
#7878=DIRECTION('center_axis',(0.,0.,1.));
#7879=DIRECTION('ref_axis',(1.,0.,0.));
#7880=DIRECTION('axis',(0.,0.,1.));
#7881=DIRECTION('refdir',(1.,0.,0.));
#7882=DIRECTION('center_axis',(0.,0.,1.));
#7883=DIRECTION('ref_axis',(-0.457983707777832,-0.888960585971093,0.));
#7884=DIRECTION('',(0.,0.,-1.));
#7885=DIRECTION('center_axis',(0.,0.,-1.));
#7886=DIRECTION('ref_axis',(1.,-1.35784937511192E-12,0.));
#7887=DIRECTION('center_axis',(0.,0.,1.));
#7888=DIRECTION('ref_axis',(-0.457983707777832,-0.888960585971093,0.));
#7889=DIRECTION('',(0.,0.,-1.));
#7890=DIRECTION('center_axis',(0.,0.,1.));
#7891=DIRECTION('ref_axis',(-0.457983707777832,-0.888960585971093,0.));
#7892=DIRECTION('',(0.,0.,-1.));
#7893=DIRECTION('center_axis',(0.,0.,1.));
#7894=DIRECTION('ref_axis',(-0.457983707777832,-0.888960585971093,0.));
#7895=DIRECTION('',(0.,0.,-1.));
#7896=DIRECTION('center_axis',(0.,0.,1.));
#7897=DIRECTION('ref_axis',(-0.457983707777832,-0.888960585971093,0.));
#7898=DIRECTION('',(0.,0.,-1.));
#7899=DIRECTION('center_axis',(0.,0.,1.));
#7900=DIRECTION('ref_axis',(-0.457983707777832,-0.888960585971093,0.));
#7901=DIRECTION('',(0.,0.,-1.));
#7902=DIRECTION('center_axis',(0.,0.,1.));
#7903=DIRECTION('ref_axis',(-0.457983707777832,-0.888960585971093,0.));
#7904=DIRECTION('',(0.,0.,-1.));
#7905=DIRECTION('center_axis',(0.,0.,1.));
#7906=DIRECTION('ref_axis',(-0.457983707777832,-0.888960585971093,0.));
#7907=DIRECTION('',(0.,0.,-1.));
#7908=DIRECTION('center_axis',(0.,0.,1.));
#7909=DIRECTION('ref_axis',(-0.457983707777832,-0.888960585971093,0.));
#7910=DIRECTION('',(0.,0.,-1.));
#7911=DIRECTION('center_axis',(0.,0.,1.));
#7912=DIRECTION('ref_axis',(-0.457983707777832,-0.888960585971093,0.));
#7913=DIRECTION('',(0.,0.,-1.));
#7914=DIRECTION('center_axis',(0.,0.,1.));
#7915=DIRECTION('ref_axis',(-0.457983707777832,-0.888960585971093,0.));
#7916=DIRECTION('',(0.,0.,-1.));
#7917=DIRECTION('center_axis',(0.,0.,1.));
#7918=DIRECTION('ref_axis',(-0.457983707777832,-0.888960585971093,0.));
#7919=DIRECTION('',(0.,0.,-1.));
#7920=DIRECTION('center_axis',(0.,0.,1.));
#7921=DIRECTION('ref_axis',(-0.457983707777832,-0.888960585971093,0.));
#7922=DIRECTION('',(0.,0.,-1.));
#7923=DIRECTION('center_axis',(0.,0.,1.));
#7924=DIRECTION('ref_axis',(-0.457983707777832,-0.888960585971093,0.));
#7925=DIRECTION('',(0.,0.,-1.));
#7926=DIRECTION('center_axis',(0.,0.,1.));
#7927=DIRECTION('ref_axis',(-0.457983707777832,-0.888960585971093,0.));
#7928=DIRECTION('',(0.,0.,-1.));
#7929=DIRECTION('center_axis',(0.,0.,1.));
#7930=DIRECTION('ref_axis',(-0.457983707777832,-0.888960585971093,0.));
#7931=DIRECTION('',(0.,0.,-1.));
#7932=DIRECTION('center_axis',(0.,0.,1.));
#7933=DIRECTION('ref_axis',(-0.457983707777832,-0.888960585971093,0.));
#7934=DIRECTION('',(0.,0.,-1.));
#7935=DIRECTION('center_axis',(0.,0.,1.));
#7936=DIRECTION('ref_axis',(-0.457983707777832,-0.888960585971093,0.));
#7937=DIRECTION('',(0.,0.,-1.));
#7938=DIRECTION('center_axis',(0.,0.,1.));
#7939=DIRECTION('ref_axis',(-0.457983707777832,-0.888960585971093,0.));
#7940=DIRECTION('',(0.,0.,-1.));
#7941=DIRECTION('center_axis',(0.,0.,1.));
#7942=DIRECTION('ref_axis',(-0.457983707777832,-0.888960585971093,0.));
#7943=DIRECTION('',(0.,0.,-1.));
#7944=DIRECTION('center_axis',(0.,0.,1.));
#7945=DIRECTION('ref_axis',(-0.457983707777832,-0.888960585971093,0.));
#7946=DIRECTION('',(0.,0.,-1.));
#7947=DIRECTION('center_axis',(0.,0.,1.));
#7948=DIRECTION('ref_axis',(-0.457983707777832,-0.888960585971093,0.));
#7949=DIRECTION('',(0.,0.,-1.));
#7950=DIRECTION('center_axis',(0.,0.,1.));
#7951=DIRECTION('ref_axis',(-0.457983707777832,-0.888960585971093,0.));
#7952=DIRECTION('',(0.,0.,-1.));
#7953=DIRECTION('center_axis',(0.,0.,1.));
#7954=DIRECTION('ref_axis',(-0.457983707777832,-0.888960585971093,0.));
#7955=DIRECTION('',(0.,0.,-1.));
#7956=DIRECTION('center_axis',(0.,0.,1.));
#7957=DIRECTION('ref_axis',(-0.457983707777832,-0.888960585971093,0.));
#7958=DIRECTION('',(0.,0.,-1.));
#7959=DIRECTION('center_axis',(0.,0.,1.));
#7960=DIRECTION('ref_axis',(-0.457983707777832,-0.888960585971093,0.));
#7961=DIRECTION('',(0.,0.,-1.));
#7962=DIRECTION('center_axis',(0.,0.,1.));
#7963=DIRECTION('ref_axis',(-0.457983707777832,-0.888960585971093,0.));
#7964=DIRECTION('',(0.,0.,-1.));
#7965=DIRECTION('center_axis',(0.,0.,1.));
#7966=DIRECTION('ref_axis',(-0.457983707777832,-0.888960585971093,0.));
#7967=DIRECTION('',(0.,0.,-1.));
#7968=DIRECTION('center_axis',(0.,0.,1.));
#7969=DIRECTION('ref_axis',(-0.457983707777832,-0.888960585971093,0.));
#7970=DIRECTION('',(0.,0.,-1.));
#7971=DIRECTION('center_axis',(0.,0.,1.));
#7972=DIRECTION('ref_axis',(-0.457983707777832,-0.888960585971093,0.));
#7973=DIRECTION('',(0.,0.,-1.));
#7974=DIRECTION('center_axis',(0.,0.,1.));
#7975=DIRECTION('ref_axis',(-0.457983707777832,-0.888960585971093,0.));
#7976=DIRECTION('',(0.,0.,-1.));
#7977=DIRECTION('center_axis',(0.,0.,1.));
#7978=DIRECTION('ref_axis',(-0.457983707777832,-0.888960585971093,0.));
#7979=DIRECTION('',(0.,0.,-1.));
#7980=DIRECTION('center_axis',(0.,0.,1.));
#7981=DIRECTION('ref_axis',(-0.457983707777832,-0.888960585971093,0.));
#7982=DIRECTION('',(0.,0.,-1.));
#7983=DIRECTION('center_axis',(0.,0.,1.));
#7984=DIRECTION('ref_axis',(-0.457983707777832,-0.888960585971093,0.));
#7985=DIRECTION('',(0.,0.,-1.));
#7986=DIRECTION('center_axis',(0.,0.,1.));
#7987=DIRECTION('ref_axis',(-0.457983707777832,-0.888960585971093,0.));
#7988=DIRECTION('',(0.,0.,-1.));
#7989=DIRECTION('center_axis',(0.,0.,1.));
#7990=DIRECTION('ref_axis',(-0.457983707777832,-0.888960585971093,0.));
#7991=DIRECTION('',(0.,0.,-1.));
#7992=DIRECTION('center_axis',(0.,0.,1.));
#7993=DIRECTION('ref_axis',(-0.457983707777832,-0.888960585971093,0.));
#7994=DIRECTION('',(0.,0.,-1.));
#7995=DIRECTION('center_axis',(0.,0.,1.));
#7996=DIRECTION('ref_axis',(-0.457983707777832,-0.888960585971093,0.));
#7997=DIRECTION('',(0.,0.,-1.));
#7998=DIRECTION('center_axis',(0.,0.,1.));
#7999=DIRECTION('ref_axis',(-0.457983707777832,-0.888960585971093,0.));
#8000=DIRECTION('',(0.,0.,-1.));
#8001=DIRECTION('center_axis',(0.,0.,1.));
#8002=DIRECTION('ref_axis',(-0.457983707777832,-0.888960585971093,0.));
#8003=DIRECTION('',(0.,0.,-1.));
#8004=DIRECTION('center_axis',(0.,0.,1.));
#8005=DIRECTION('ref_axis',(-0.457983707777832,-0.888960585971093,0.));
#8006=DIRECTION('',(0.,0.,-1.));
#8007=DIRECTION('center_axis',(0.,0.,1.));
#8008=DIRECTION('ref_axis',(-0.457983707777832,-0.888960585971093,0.));
#8009=DIRECTION('',(0.,0.,-1.));
#8010=DIRECTION('center_axis',(0.,0.,1.));
#8011=DIRECTION('ref_axis',(-0.457983707777832,-0.888960585971093,0.));
#8012=DIRECTION('',(0.,0.,-1.));
#8013=DIRECTION('center_axis',(0.,0.,1.));
#8014=DIRECTION('ref_axis',(-0.457983707777832,-0.888960585971093,0.));
#8015=DIRECTION('',(0.,0.,-1.));
#8016=DIRECTION('center_axis',(0.,0.,1.));
#8017=DIRECTION('ref_axis',(-0.457983707777832,-0.888960585971093,0.));
#8018=DIRECTION('',(0.,0.,-1.));
#8019=DIRECTION('center_axis',(0.,0.,1.));
#8020=DIRECTION('ref_axis',(-0.457983707777832,-0.888960585971093,0.));
#8021=DIRECTION('',(0.,0.,-1.));
#8022=DIRECTION('center_axis',(0.,0.,1.));
#8023=DIRECTION('ref_axis',(-0.457983707777832,-0.888960585971093,0.));
#8024=DIRECTION('',(0.,0.,-1.));
#8025=DIRECTION('center_axis',(0.,0.,1.));
#8026=DIRECTION('ref_axis',(-0.457983707777832,-0.888960585971093,0.));
#8027=DIRECTION('',(0.,0.,-1.));
#8028=DIRECTION('center_axis',(0.,0.,1.));
#8029=DIRECTION('ref_axis',(-0.457983707777832,-0.888960585971093,0.));
#8030=DIRECTION('',(0.,0.,-1.));
#8031=DIRECTION('center_axis',(0.,0.,1.));
#8032=DIRECTION('ref_axis',(-0.457983707777832,-0.888960585971093,0.));
#8033=DIRECTION('',(0.,0.,-1.));
#8034=DIRECTION('center_axis',(0.,0.,1.));
#8035=DIRECTION('ref_axis',(-0.457983707777832,-0.888960585971093,0.));
#8036=DIRECTION('',(0.,0.,-1.));
#8037=DIRECTION('center_axis',(0.,0.,1.));
#8038=DIRECTION('ref_axis',(-0.457983707777832,-0.888960585971093,0.));
#8039=DIRECTION('',(0.,0.,-1.));
#8040=DIRECTION('center_axis',(0.,0.,1.));
#8041=DIRECTION('ref_axis',(-0.457983707777832,-0.888960585971093,0.));
#8042=DIRECTION('',(0.,0.,-1.));
#8043=DIRECTION('center_axis',(0.,0.,1.));
#8044=DIRECTION('ref_axis',(-0.457983707777832,-0.888960585971093,0.));
#8045=DIRECTION('',(0.,0.,-1.));
#8046=DIRECTION('center_axis',(0.,0.,1.));
#8047=DIRECTION('ref_axis',(-0.457983707777832,-0.888960585971093,0.));
#8048=DIRECTION('',(0.,0.,-1.));
#8049=DIRECTION('center_axis',(0.,0.,1.));
#8050=DIRECTION('ref_axis',(-0.457983707777832,-0.888960585971093,0.));
#8051=DIRECTION('',(0.,0.,-1.));
#8052=DIRECTION('center_axis',(0.,0.,1.));
#8053=DIRECTION('ref_axis',(-0.457983707777832,-0.888960585971093,0.));
#8054=DIRECTION('',(0.,0.,-1.));
#8055=DIRECTION('center_axis',(0.,0.,1.));
#8056=DIRECTION('ref_axis',(-0.457983707777832,-0.888960585971093,0.));
#8057=DIRECTION('',(0.,0.,-1.));
#8058=DIRECTION('center_axis',(0.,0.,1.));
#8059=DIRECTION('ref_axis',(-0.457983707777832,-0.888960585971093,0.));
#8060=DIRECTION('',(0.,0.,-1.));
#8061=DIRECTION('center_axis',(0.,0.,1.));
#8062=DIRECTION('ref_axis',(-0.457983707777832,-0.888960585971093,0.));
#8063=DIRECTION('',(0.,0.,-1.));
#8064=DIRECTION('center_axis',(0.,0.,1.));
#8065=DIRECTION('ref_axis',(-0.457983707777832,-0.888960585971093,0.));
#8066=DIRECTION('',(0.,0.,-1.));
#8067=DIRECTION('center_axis',(0.,0.,1.));
#8068=DIRECTION('ref_axis',(-0.457983707777832,-0.888960585971093,0.));
#8069=DIRECTION('',(0.,0.,-1.));
#8070=DIRECTION('center_axis',(0.,0.,1.));
#8071=DIRECTION('ref_axis',(-0.457983707777832,-0.888960585971093,0.));
#8072=DIRECTION('',(0.,0.,-1.));
#8073=DIRECTION('center_axis',(0.,0.,1.));
#8074=DIRECTION('ref_axis',(-0.457983707777832,-0.888960585971093,0.));
#8075=DIRECTION('',(0.,0.,-1.));
#8076=DIRECTION('center_axis',(0.,0.,1.));
#8077=DIRECTION('ref_axis',(-0.457983707777832,-0.888960585971093,0.));
#8078=DIRECTION('',(0.,0.,-1.));
#8079=DIRECTION('center_axis',(0.,0.,1.));
#8080=DIRECTION('ref_axis',(-0.457983707777832,-0.888960585971093,0.));
#8081=DIRECTION('',(0.,0.,-1.));
#8082=DIRECTION('center_axis',(0.,0.,1.));
#8083=DIRECTION('ref_axis',(-0.457983707777832,-0.888960585971093,0.));
#8084=DIRECTION('',(0.,0.,-1.));
#8085=DIRECTION('center_axis',(0.,0.,1.));
#8086=DIRECTION('ref_axis',(-0.457983707777832,-0.888960585971093,0.));
#8087=DIRECTION('',(0.,0.,-1.));
#8088=DIRECTION('center_axis',(0.,0.,1.));
#8089=DIRECTION('ref_axis',(-0.457983707777832,-0.888960585971093,0.));
#8090=DIRECTION('',(0.,0.,-1.));
#8091=DIRECTION('center_axis',(0.,0.,1.));
#8092=DIRECTION('ref_axis',(-0.457983707777832,-0.888960585971093,0.));
#8093=DIRECTION('',(0.,0.,-1.));
#8094=DIRECTION('center_axis',(0.,0.,1.));
#8095=DIRECTION('ref_axis',(-0.457983707777832,-0.888960585971093,0.));
#8096=DIRECTION('',(0.,0.,-1.));
#8097=DIRECTION('center_axis',(0.,0.,1.));
#8098=DIRECTION('ref_axis',(-0.457983707777832,-0.888960585971093,0.));
#8099=DIRECTION('',(0.,0.,-1.));
#8100=DIRECTION('center_axis',(0.,0.,1.));
#8101=DIRECTION('ref_axis',(-0.457983707777832,-0.888960585971093,0.));
#8102=DIRECTION('',(0.,0.,-1.));
#8103=DIRECTION('center_axis',(0.,0.,1.));
#8104=DIRECTION('ref_axis',(-0.457983707777832,-0.888960585971093,0.));
#8105=DIRECTION('',(0.,0.,-1.));
#8106=DIRECTION('center_axis',(0.,0.,1.));
#8107=DIRECTION('ref_axis',(-0.457983707777832,-0.888960585971093,0.));
#8108=DIRECTION('',(0.,0.,-1.));
#8109=DIRECTION('center_axis',(0.,0.,1.));
#8110=DIRECTION('ref_axis',(-0.457983707777832,-0.888960585971093,0.));
#8111=DIRECTION('',(0.,0.,-1.));
#8112=DIRECTION('center_axis',(0.,0.,1.));
#8113=DIRECTION('ref_axis',(-0.457983707777832,-0.888960585971093,0.));
#8114=DIRECTION('',(0.,0.,-1.));
#8115=DIRECTION('center_axis',(0.,0.,1.));
#8116=DIRECTION('ref_axis',(-0.457983707777832,-0.888960585971093,0.));
#8117=DIRECTION('center_axis',(0.,0.,1.));
#8118=DIRECTION('ref_axis',(1.,-1.35784937511192E-12,0.));
#8119=DIRECTION('center_axis',(0.,0.,1.));
#8120=DIRECTION('ref_axis',(1.,0.,0.));
#8121=DIRECTION('center_axis',(0.,0.,-1.));
#8122=DIRECTION('ref_axis',(1.,0.,0.));
#8123=DIRECTION('center_axis',(0.,0.,-1.));
#8124=DIRECTION('ref_axis',(1.,0.,0.));
#8125=DIRECTION('center_axis',(0.,0.,1.));
#8126=DIRECTION('ref_axis',(1.,0.,0.));
#8127=DIRECTION('center_axis',(0.,0.,1.));
#8128=DIRECTION('ref_axis',(1.,0.,0.));
#8129=DIRECTION('',(0.,0.,-1.));
#8130=DIRECTION('center_axis',(0.,0.,1.));
#8131=DIRECTION('ref_axis',(1.,0.,0.));
#8132=DIRECTION('center_axis',(0.,0.,-1.));
#8133=DIRECTION('ref_axis',(-1.,0.,0.));
#8134=DIRECTION('center_axis',(0.,0.,-1.));
#8135=DIRECTION('ref_axis',(1.,0.,0.));
#8136=DIRECTION('center_axis',(0.,0.,1.));
#8137=DIRECTION('ref_axis',(1.,0.,0.));
#8138=DIRECTION('center_axis',(0.,0.,1.));
#8139=DIRECTION('ref_axis',(1.,0.,0.));
#8140=DIRECTION('center_axis',(0.,0.,1.));
#8141=DIRECTION('ref_axis',(1.,0.,0.));
#8142=DIRECTION('center_axis',(0.,0.,1.));
#8143=DIRECTION('ref_axis',(1.,0.,0.));
#8144=DIRECTION('',(0.,0.,-1.));
#8145=DIRECTION('center_axis',(0.,0.,1.));
#8146=DIRECTION('ref_axis',(1.,0.,0.));
#8147=DIRECTION('',(0.,0.,-1.));
#8148=DIRECTION('center_axis',(0.,0.,-1.));
#8149=DIRECTION('ref_axis',(1.,0.,0.));
#8150=DIRECTION('center_axis',(0.,0.,1.));
#8151=DIRECTION('ref_axis',(1.,0.,0.));
#8152=DIRECTION('center_axis',(0.,0.,1.));
#8153=DIRECTION('ref_axis',(1.,0.,0.));
#8154=DIRECTION('center_axis',(0.,0.,1.));
#8155=DIRECTION('ref_axis',(1.,0.,0.));
#8156=DIRECTION('center_axis',(0.,0.,1.));
#8157=DIRECTION('ref_axis',(1.,0.,0.));
#8158=DIRECTION('center_axis',(6.78567850819536E-13,5.53097019214562E-13,
1.));
#8159=DIRECTION('ref_axis',(0.504160107343572,-0.86361020499026,1.35553389634315E-13));
#8160=DIRECTION('center_axis',(-6.40020660077179E-13,6.68075341414769E-13,
1.));
#8161=DIRECTION('ref_axis',(0.774139656364633,0.633014843778287,7.25637659806176E-14));
#8162=DIRECTION('center_axis',(0.,0.,1.));
#8163=DIRECTION('ref_axis',(1.,0.,0.));
#8164=DIRECTION('center_axis',(0.,0.,1.));
#8165=DIRECTION('ref_axis',(1.,0.,0.));
#8166=DIRECTION('',(0.,0.,-1.));
#8167=DIRECTION('center_axis',(0.,0.,1.));
#8168=DIRECTION('ref_axis',(1.,0.,0.));
#8169=DIRECTION('center_axis',(0.,0.,-1.));
#8170=DIRECTION('ref_axis',(1.,0.,0.));
#8171=DIRECTION('center_axis',(0.,0.,-1.));
#8172=DIRECTION('ref_axis',(1.,0.,0.));
#8173=DIRECTION('',(0.,0.,-1.));
#8174=DIRECTION('center_axis',(0.,0.,1.));
#8175=DIRECTION('ref_axis',(1.,0.,0.));
#8176=DIRECTION('center_axis',(0.,0.,-1.));
#8177=DIRECTION('ref_axis',(1.,0.,0.));
#8178=DIRECTION('center_axis',(0.,0.,-1.));
#8179=DIRECTION('ref_axis',(1.,0.,0.));
#8180=DIRECTION('',(0.,0.,-1.));
#8181=DIRECTION('center_axis',(0.,0.,1.));
#8182=DIRECTION('ref_axis',(1.,0.,0.));
#8183=DIRECTION('center_axis',(0.,0.,-1.));
#8184=DIRECTION('ref_axis',(1.,0.,0.));
#8185=DIRECTION('center_axis',(0.,0.,-1.));
#8186=DIRECTION('ref_axis',(1.,0.,0.));
#8187=DIRECTION('',(0.,0.,-1.));
#8188=DIRECTION('center_axis',(0.,0.,1.));
#8189=DIRECTION('ref_axis',(1.,0.,0.));
#8190=DIRECTION('center_axis',(0.,0.,-1.));
#8191=DIRECTION('ref_axis',(1.,0.,0.));
#8192=DIRECTION('center_axis',(0.,0.,-1.));
#8193=DIRECTION('ref_axis',(1.,0.,0.));
#8194=DIRECTION('',(0.,0.,-1.));
#8195=DIRECTION('center_axis',(0.,0.,1.));
#8196=DIRECTION('ref_axis',(1.,0.,0.));
#8197=DIRECTION('center_axis',(0.,0.,-1.));
#8198=DIRECTION('ref_axis',(0.568605661693349,0.822610236679722,0.));
#8199=DIRECTION('center_axis',(-2.40370335797945E-16,-1.,0.));
#8200=DIRECTION('ref_axis',(1.,-2.40370335797945E-16,0.));
#8201=DIRECTION('',(1.,-2.40370335797945E-16,0.));
#8202=DIRECTION('',(0.,0.,1.));
#8203=DIRECTION('',(1.,-2.40370335797945E-16,0.));
#8204=DIRECTION('',(0.,0.,1.));
#8205=DIRECTION('center_axis',(-0.866025403784439,-0.5,0.));
#8206=DIRECTION('ref_axis',(0.5,-0.866025403784439,0.));
#8207=DIRECTION('',(0.5,-0.866025403784439,0.));
#8208=DIRECTION('',(0.,0.,1.));
#8209=DIRECTION('',(0.5,-0.866025403784439,0.));
#8210=DIRECTION('center_axis',(-0.866025403784439,0.5,0.));
#8211=DIRECTION('ref_axis',(-0.5,-0.866025403784439,0.));
#8212=DIRECTION('',(-0.5,-0.866025403784439,0.));
#8213=DIRECTION('',(0.,0.,1.));
#8214=DIRECTION('',(-0.5,-0.866025403784439,0.));
#8215=DIRECTION('center_axis',(1.20185167898973E-16,1.,0.));
#8216=DIRECTION('ref_axis',(-1.,1.20185167898973E-16,0.));
#8217=DIRECTION('',(-1.,1.20185167898973E-16,0.));
#8218=DIRECTION('',(0.,0.,1.));
#8219=DIRECTION('',(-1.,1.20185167898973E-16,0.));
#8220=DIRECTION('center_axis',(0.866025403784439,0.5,0.));
#8221=DIRECTION('ref_axis',(-0.5,0.866025403784439,0.));
#8222=DIRECTION('',(-0.5,0.866025403784439,0.));
#8223=DIRECTION('',(0.,0.,1.));
#8224=DIRECTION('',(-0.5,0.866025403784439,0.));
#8225=DIRECTION('center_axis',(0.866025403784439,-0.5,0.));
#8226=DIRECTION('ref_axis',(0.5,0.866025403784439,0.));
#8227=DIRECTION('',(0.5,0.866025403784439,0.));
#8228=DIRECTION('',(0.5,0.866025403784439,0.));
#8229=DIRECTION('center_axis',(0.,0.,1.));
#8230=DIRECTION('ref_axis',(1.,0.,0.));
#8231=DIRECTION('center_axis',(0.,0.,1.));
#8232=DIRECTION('ref_axis',(1.,0.,0.));
#8233=DIRECTION('center_axis',(0.,0.,-1.));
#8234=DIRECTION('ref_axis',(1.,0.,0.));
#8235=DIRECTION('center_axis',(0.,0.,1.));
#8236=DIRECTION('ref_axis',(1.,0.,0.));
#8237=DIRECTION('',(0.,0.,-1.));
#8238=DIRECTION('center_axis',(0.,0.,-1.));
#8239=DIRECTION('ref_axis',(1.,0.,0.));
#8240=DIRECTION('center_axis',(0.,0.,1.));
#8241=DIRECTION('ref_axis',(1.,0.,0.));
#8242=DIRECTION('axis',(0.,0.,1.));
#8243=DIRECTION('refdir',(1.,0.,0.));
#8244=DIRECTION('center_axis',(-1.,0.,0.));
#8245=DIRECTION('ref_axis',(0.,1.,0.));
#8246=DIRECTION('',(0.,0.,1.));
#8247=DIRECTION('',(0.,-1.,0.));
#8248=DIRECTION('',(0.,0.,-1.));
#8249=DIRECTION('',(0.,1.,0.));
#8250=DIRECTION('center_axis',(1.,0.,0.));
#8251=DIRECTION('ref_axis',(0.,-1.,0.));
#8252=DIRECTION('',(0.,0.,-1.));
#8253=DIRECTION('',(0.,-1.,0.));
#8254=DIRECTION('',(0.,0.,1.));
#8255=DIRECTION('',(0.,1.,0.));
#8256=DIRECTION('center_axis',(0.,0.,1.));
#8257=DIRECTION('ref_axis',(1.,0.,0.));
#8258=DIRECTION('center_axis',(0.,0.,1.));
#8259=DIRECTION('ref_axis',(1.,0.,0.));
#8260=DIRECTION('center_axis',(0.,0.,-1.));
#8261=DIRECTION('ref_axis',(1.,0.,0.));
#8262=DIRECTION('center_axis',(0.,0.,1.));
#8263=DIRECTION('ref_axis',(6.12323399573677E-17,-1.,0.));
#8264=DIRECTION('center_axis',(0.,0.,-1.));
#8265=DIRECTION('ref_axis',(1.,0.,0.));
#8266=DIRECTION('center_axis',(0.,0.,1.));
#8267=DIRECTION('ref_axis',(6.12323399573677E-17,-1.,0.));
#8268=DIRECTION('center_axis',(0.,0.,1.));
#8269=DIRECTION('ref_axis',(1.,0.,0.));
#8270=DIRECTION('center_axis',(0.,0.,1.));
#8271=DIRECTION('ref_axis',(1.,0.,0.));
#8272=DIRECTION('axis',(0.,0.,1.));
#8273=DIRECTION('refdir',(1.,0.,0.));
#8274=DIRECTION('center_axis',(0.,0.,-1.));
#8275=DIRECTION('ref_axis',(-0.608813211676711,-0.793313603367475,0.));
#8276=DIRECTION('',(0.,0.,-1.));
#8277=DIRECTION('center_axis',(0.,0.,1.));
#8278=DIRECTION('ref_axis',(1.,-3.58774509990574E-14,0.));
#8279=DIRECTION('center_axis',(0.,0.,-1.));
#8280=DIRECTION('ref_axis',(-0.608813211676711,-0.793313603367475,0.));
#8281=DIRECTION('',(0.,0.,-1.));
#8282=DIRECTION('center_axis',(0.,0.,-1.));
#8283=DIRECTION('ref_axis',(-0.608813211676711,-0.793313603367475,0.));
#8284=DIRECTION('',(0.,0.,-1.));
#8285=DIRECTION('center_axis',(0.,0.,-1.));
#8286=DIRECTION('ref_axis',(-0.608813211676711,-0.793313603367475,0.));
#8287=DIRECTION('',(0.,0.,-1.));
#8288=DIRECTION('center_axis',(0.,0.,-1.));
#8289=DIRECTION('ref_axis',(-0.608813211676711,-0.793313603367475,0.));
#8290=DIRECTION('',(0.,0.,-1.));
#8291=DIRECTION('center_axis',(0.,0.,-1.));
#8292=DIRECTION('ref_axis',(-0.608813211676711,-0.793313603367475,0.));
#8293=DIRECTION('',(0.,0.,-1.));
#8294=DIRECTION('center_axis',(0.,0.,-1.));
#8295=DIRECTION('ref_axis',(-0.608813211676711,-0.793313603367475,0.));
#8296=DIRECTION('',(0.,0.,-1.));
#8297=DIRECTION('center_axis',(0.,0.,-1.));
#8298=DIRECTION('ref_axis',(-0.608813211676711,-0.793313603367475,0.));
#8299=DIRECTION('',(0.,0.,-1.));
#8300=DIRECTION('center_axis',(0.,0.,-1.));
#8301=DIRECTION('ref_axis',(-0.608813211676711,-0.793313603367475,0.));
#8302=DIRECTION('',(0.,0.,-1.));
#8303=DIRECTION('center_axis',(0.,0.,-1.));
#8304=DIRECTION('ref_axis',(-0.608813211676711,-0.793313603367475,0.));
#8305=DIRECTION('',(0.,0.,-1.));
#8306=DIRECTION('center_axis',(0.,0.,-1.));
#8307=DIRECTION('ref_axis',(1.,-3.58774509990574E-14,0.));
#8308=DIRECTION('center_axis',(0.,0.,-1.));
#8309=DIRECTION('ref_axis',(0.937388910103482,-0.348284411386738,0.));
#8310=DIRECTION('',(0.,0.,-1.));
#8311=DIRECTION('center_axis',(0.,0.,-1.));
#8312=DIRECTION('ref_axis',(1.,0.,0.));
#8313=DIRECTION('center_axis',(0.,0.,-1.));
#8314=DIRECTION('ref_axis',(0.937388910103482,-0.348284411386738,0.));
#8315=DIRECTION('',(0.,0.,-1.));
#8316=DIRECTION('center_axis',(0.,0.,-1.));
#8317=DIRECTION('ref_axis',(0.937388910103482,-0.348284411386738,0.));
#8318=DIRECTION('',(0.,0.,-1.));
#8319=DIRECTION('center_axis',(0.,0.,-1.));
#8320=DIRECTION('ref_axis',(0.937388910103482,-0.348284411386738,0.));
#8321=DIRECTION('',(0.,0.,-1.));
#8322=DIRECTION('center_axis',(0.,0.,-1.));
#8323=DIRECTION('ref_axis',(0.937388910103482,-0.348284411386738,0.));
#8324=DIRECTION('',(0.,0.,-1.));
#8325=DIRECTION('center_axis',(0.,0.,-1.));
#8326=DIRECTION('ref_axis',(0.937388910103482,-0.348284411386738,0.));
#8327=DIRECTION('',(0.,0.,-1.));
#8328=DIRECTION('center_axis',(0.,0.,-1.));
#8329=DIRECTION('ref_axis',(0.937388910103482,-0.348284411386738,0.));
#8330=DIRECTION('',(0.,0.,-1.));
#8331=DIRECTION('center_axis',(0.,0.,-1.));
#8332=DIRECTION('ref_axis',(0.937388910103482,-0.348284411386738,0.));
#8333=DIRECTION('',(0.,0.,-1.));
#8334=DIRECTION('center_axis',(0.,0.,-1.));
#8335=DIRECTION('ref_axis',(0.937388910103482,-0.348284411386738,0.));
#8336=DIRECTION('',(0.,0.,-1.));
#8337=DIRECTION('center_axis',(0.,0.,-1.));
#8338=DIRECTION('ref_axis',(0.937388910103482,-0.348284411386738,0.));
#8339=DIRECTION('',(0.,0.,-1.));
#8340=DIRECTION('center_axis',(0.,0.,-1.));
#8341=DIRECTION('ref_axis',(1.,0.,0.));
#8342=DIRECTION('center_axis',(0.,0.,-1.));
#8343=DIRECTION('ref_axis',(0.937388910103482,-0.348284411386738,0.));
#8344=DIRECTION('center_axis',(0.,0.,-1.));
#8345=DIRECTION('ref_axis',(-0.608813211676711,-0.793313603367475,0.));
#8346=DIRECTION('center_axis',(0.,0.,-1.));
#8347=DIRECTION('ref_axis',(1.,0.,0.));
#8348=DIRECTION('center_axis',(0.,0.,-1.));
#8349=DIRECTION('ref_axis',(1.,0.,0.));
#8350=DIRECTION('',(0.,0.,-1.));
#8351=DIRECTION('center_axis',(0.,0.,1.));
#8352=DIRECTION('ref_axis',(1.,0.,0.));
#8353=DIRECTION('center_axis',(0.,0.,-1.));
#8354=DIRECTION('ref_axis',(1.,0.,0.));
#8355=DIRECTION('center_axis',(0.,0.,-1.));
#8356=DIRECTION('ref_axis',(1.,0.,0.));
#8357=DIRECTION('',(0.,0.,-1.));
#8358=DIRECTION('center_axis',(0.,0.,1.));
#8359=DIRECTION('ref_axis',(1.,0.,0.));
#8360=DIRECTION('center_axis',(0.,0.,1.));
#8361=DIRECTION('ref_axis',(1.,0.,0.));
#8362=DIRECTION('',(0.,-1.,0.));
#8363=DIRECTION('',(1.,0.,0.));
#8364=DIRECTION('',(0.,1.,0.));
#8365=DIRECTION('',(1.,0.,0.));
#8366=DIRECTION('center_axis',(0.,0.,-1.));
#8367=DIRECTION('ref_axis',(1.,0.,0.));
#8368=DIRECTION('center_axis',(0.,0.,-1.));
#8369=DIRECTION('ref_axis',(1.,0.,0.));
#8370=DIRECTION('center_axis',(0.,0.,-1.));
#8371=DIRECTION('ref_axis',(1.,0.,0.));
#8372=DIRECTION('',(0.,0.,-1.));
#8373=DIRECTION('center_axis',(0.,0.,1.));
#8374=DIRECTION('ref_axis',(1.,0.,0.));
#8375=DIRECTION('center_axis',(0.,0.,-1.));
#8376=DIRECTION('ref_axis',(1.,0.,0.));
#8377=DIRECTION('',(0.,0.,-1.));
#8378=DIRECTION('center_axis',(0.,0.,1.));
#8379=DIRECTION('ref_axis',(1.,0.,0.));
#8380=DIRECTION('center_axis',(0.,1.,0.));
#8381=DIRECTION('ref_axis',(-1.,0.,0.));
#8382=DIRECTION('',(1.,0.,0.));
#8383=DIRECTION('',(0.,0.,1.));
#8384=DIRECTION('',(0.,0.,-1.));
#8385=DIRECTION('center_axis',(1.,0.,0.));
#8386=DIRECTION('ref_axis',(0.,1.,0.));
#8387=DIRECTION('',(0.,1.,0.));
#8388=DIRECTION('',(0.,0.,1.));
#8389=DIRECTION('center_axis',(0.,-1.,0.));
#8390=DIRECTION('ref_axis',(1.,0.,0.));
#8391=DIRECTION('',(1.,0.,0.));
#8392=DIRECTION('',(0.,0.,1.));
#8393=DIRECTION('center_axis',(-1.,0.,0.));
#8394=DIRECTION('ref_axis',(0.,-1.,0.));
#8395=DIRECTION('',(0.,-1.,0.));
#8396=DIRECTION('center_axis',(0.,0.,1.));
#8397=DIRECTION('ref_axis',(1.,0.,0.));
#8398=DIRECTION('axis',(0.,0.,1.));
#8399=DIRECTION('refdir',(1.,0.,0.));
#8400=DIRECTION('center_axis',(0.,0.,-1.));
#8401=DIRECTION('ref_axis',(-0.609178726672388,-0.793032962095402,0.));
#8402=DIRECTION('',(0.,0.,-1.));
#8403=DIRECTION('center_axis',(0.,0.,1.));
#8404=DIRECTION('ref_axis',(1.,-7.46332589967923E-15,0.));
#8405=DIRECTION('center_axis',(0.,0.,-1.));
#8406=DIRECTION('ref_axis',(-0.609178726672388,-0.793032962095402,0.));
#8407=DIRECTION('',(0.,0.,-1.));
#8408=DIRECTION('center_axis',(0.,0.,-1.));
#8409=DIRECTION('ref_axis',(-0.609178726672388,-0.793032962095402,0.));
#8410=DIRECTION('',(0.,0.,-1.));
#8411=DIRECTION('center_axis',(0.,0.,-1.));
#8412=DIRECTION('ref_axis',(-0.609178726672388,-0.793032962095402,0.));
#8413=DIRECTION('',(0.,0.,-1.));
#8414=DIRECTION('center_axis',(0.,0.,-1.));
#8415=DIRECTION('ref_axis',(-0.609178726672388,-0.793032962095402,0.));
#8416=DIRECTION('',(0.,0.,-1.));
#8417=DIRECTION('center_axis',(0.,0.,-1.));
#8418=DIRECTION('ref_axis',(-0.609178726672388,-0.793032962095402,0.));
#8419=DIRECTION('',(0.,0.,-1.));
#8420=DIRECTION('center_axis',(0.,0.,-1.));
#8421=DIRECTION('ref_axis',(1.,-7.46332589967923E-15,0.));
#8422=DIRECTION('center_axis',(0.,0.,-1.));
#8423=DIRECTION('ref_axis',(-0.609178844542212,-0.793032871552129,0.));
#8424=DIRECTION('',(0.,0.,-1.));
#8425=DIRECTION('center_axis',(0.,0.,1.));
#8426=DIRECTION('ref_axis',(1.,-7.50489341657914E-15,0.));
#8427=DIRECTION('center_axis',(0.,0.,-1.));
#8428=DIRECTION('ref_axis',(-0.609178844542212,-0.793032871552129,0.));
#8429=DIRECTION('',(0.,0.,-1.));
#8430=DIRECTION('center_axis',(0.,0.,-1.));
#8431=DIRECTION('ref_axis',(-0.609178844542212,-0.793032871552129,0.));
#8432=DIRECTION('',(0.,0.,-1.));
#8433=DIRECTION('center_axis',(0.,0.,-1.));
#8434=DIRECTION('ref_axis',(-0.609178844542212,-0.793032871552129,0.));
#8435=DIRECTION('',(0.,0.,-1.));
#8436=DIRECTION('center_axis',(0.,0.,-1.));
#8437=DIRECTION('ref_axis',(-0.609178844542212,-0.793032871552129,0.));
#8438=DIRECTION('',(0.,0.,-1.));
#8439=DIRECTION('center_axis',(0.,0.,-1.));
#8440=DIRECTION('ref_axis',(-0.609178844542212,-0.793032871552129,0.));
#8441=DIRECTION('',(0.,0.,-1.));
#8442=DIRECTION('center_axis',(0.,0.,-1.));
#8443=DIRECTION('ref_axis',(1.,-7.50489341657914E-15,0.));
#8444=DIRECTION('center_axis',(0.,0.,-1.));
#8445=DIRECTION('ref_axis',(0.938005636158359,-0.34662000307996,0.));
#8446=DIRECTION('',(0.,0.,-1.));
#8447=DIRECTION('center_axis',(0.,0.,-1.));
#8448=DIRECTION('ref_axis',(1.,0.,0.));
#8449=DIRECTION('center_axis',(0.,0.,-1.));
#8450=DIRECTION('ref_axis',(0.938005636158359,-0.34662000307996,0.));
#8451=DIRECTION('',(0.,0.,-1.));
#8452=DIRECTION('center_axis',(0.,0.,-1.));
#8453=DIRECTION('ref_axis',(0.938005636158359,-0.34662000307996,0.));
#8454=DIRECTION('',(0.,0.,-1.));
#8455=DIRECTION('center_axis',(0.,0.,-1.));
#8456=DIRECTION('ref_axis',(0.938005636158359,-0.34662000307996,0.));
#8457=DIRECTION('',(0.,0.,-1.));
#8458=DIRECTION('center_axis',(0.,0.,-1.));
#8459=DIRECTION('ref_axis',(0.938005636158359,-0.34662000307996,0.));
#8460=DIRECTION('',(0.,0.,-1.));
#8461=DIRECTION('center_axis',(0.,0.,-1.));
#8462=DIRECTION('ref_axis',(0.938005636158359,-0.34662000307996,0.));
#8463=DIRECTION('',(0.,0.,-1.));
#8464=DIRECTION('center_axis',(0.,0.,-1.));
#8465=DIRECTION('ref_axis',(1.,0.,0.));
#8466=DIRECTION('center_axis',(0.,0.,-1.));
#8467=DIRECTION('ref_axis',(0.938005556308566,-0.346620219165381,0.));
#8468=DIRECTION('',(0.,0.,-1.));
#8469=DIRECTION('center_axis',(0.,0.,-1.));
#8470=DIRECTION('ref_axis',(1.,0.,0.));
#8471=DIRECTION('center_axis',(0.,0.,-1.));
#8472=DIRECTION('ref_axis',(0.938005556308566,-0.346620219165381,0.));
#8473=DIRECTION('',(0.,0.,-1.));
#8474=DIRECTION('center_axis',(0.,0.,-1.));
#8475=DIRECTION('ref_axis',(0.938005556308566,-0.346620219165381,0.));
#8476=DIRECTION('',(0.,0.,-1.));
#8477=DIRECTION('center_axis',(0.,0.,-1.));
#8478=DIRECTION('ref_axis',(0.938005556308566,-0.346620219165381,0.));
#8479=DIRECTION('',(0.,0.,-1.));
#8480=DIRECTION('center_axis',(0.,0.,-1.));
#8481=DIRECTION('ref_axis',(0.938005556308566,-0.346620219165381,0.));
#8482=DIRECTION('',(0.,0.,-1.));
#8483=DIRECTION('center_axis',(0.,0.,-1.));
#8484=DIRECTION('ref_axis',(0.938005556308566,-0.346620219165381,0.));
#8485=DIRECTION('',(0.,0.,-1.));
#8486=DIRECTION('center_axis',(0.,0.,-1.));
#8487=DIRECTION('ref_axis',(1.,0.,0.));
#8488=DIRECTION('center_axis',(0.,0.,-1.));
#8489=DIRECTION('ref_axis',(0.938005556308566,-0.346620219165381,0.));
#8490=DIRECTION('center_axis',(0.,0.,-1.));
#8491=DIRECTION('ref_axis',(0.938005636158359,-0.34662000307996,0.));
#8492=DIRECTION('center_axis',(0.,0.,-1.));
#8493=DIRECTION('ref_axis',(-0.609178844542212,-0.793032871552129,0.));
#8494=DIRECTION('center_axis',(0.,0.,-1.));
#8495=DIRECTION('ref_axis',(-0.609178726672388,-0.793032962095402,0.));
#8496=DIRECTION('center_axis',(0.,0.,1.));
#8497=DIRECTION('ref_axis',(1.,0.,0.));
#8498=DIRECTION('',(0.,-1.,0.));
#8499=DIRECTION('',(1.,0.,0.));
#8500=DIRECTION('',(0.,1.,0.));
#8501=DIRECTION('',(-1.,0.,0.));
#8502=DIRECTION('center_axis',(0.,0.,-1.));
#8503=DIRECTION('ref_axis',(1.,0.,0.));
#8504=DIRECTION('center_axis',(0.,0.,-1.));
#8505=DIRECTION('ref_axis',(1.,0.,0.));
#8506=DIRECTION('',(0.,0.,-1.));
#8507=DIRECTION('center_axis',(0.,0.,1.));
#8508=DIRECTION('ref_axis',(1.,0.,0.));
#8509=DIRECTION('center_axis',(0.,1.,0.));
#8510=DIRECTION('ref_axis',(-1.,0.,0.));
#8511=DIRECTION('',(-1.,0.,0.));
#8512=DIRECTION('',(0.,0.,1.));
#8513=DIRECTION('',(0.,0.,1.));
#8514=DIRECTION('center_axis',(1.,0.,0.));
#8515=DIRECTION('ref_axis',(0.,1.,0.));
#8516=DIRECTION('',(0.,1.,0.));
#8517=DIRECTION('',(0.,0.,1.));
#8518=DIRECTION('center_axis',(0.,-1.,0.));
#8519=DIRECTION('ref_axis',(1.,0.,0.));
#8520=DIRECTION('',(1.,0.,0.));
#8521=DIRECTION('',(0.,0.,1.));
#8522=DIRECTION('center_axis',(-1.,0.,0.));
#8523=DIRECTION('ref_axis',(0.,-1.,0.));
#8524=DIRECTION('',(0.,-1.,0.));
#8525=DIRECTION('center_axis',(0.,0.,1.));
#8526=DIRECTION('ref_axis',(1.,0.,0.));
#8527=DIRECTION('axis',(0.,0.,1.));
#8528=DIRECTION('refdir',(1.,0.,0.));
#8529=DIRECTION('center_axis',(0.,0.,1.));
#8530=DIRECTION('ref_axis',(1.,0.,0.));
#8531=DIRECTION('center_axis',(0.,0.,1.));
#8532=DIRECTION('ref_axis',(1.,0.,0.));
#8533=DIRECTION('',(0.,0.,-1.));
#8534=DIRECTION('center_axis',(0.,0.,1.));
#8535=DIRECTION('ref_axis',(1.,0.,0.));
#8536=DIRECTION('center_axis',(0.,0.,-1.));
#8537=DIRECTION('ref_axis',(-1.,0.,0.));
#8538=DIRECTION('center_axis',(0.,0.,-1.));
#8539=DIRECTION('ref_axis',(1.,0.,0.));
#8540=DIRECTION('center_axis',(0.,0.,1.));
#8541=DIRECTION('ref_axis',(1.,0.,0.));
#8542=DIRECTION('center_axis',(0.,0.,1.));
#8543=DIRECTION('ref_axis',(1.,0.,0.));
#8544=DIRECTION('center_axis',(0.,0.,1.));
#8545=DIRECTION('ref_axis',(1.,0.,0.));
#8546=DIRECTION('center_axis',(0.,0.,1.));
#8547=DIRECTION('ref_axis',(1.,0.,0.));
#8548=DIRECTION('',(0.,0.,-1.));
#8549=DIRECTION('center_axis',(0.,0.,1.));
#8550=DIRECTION('ref_axis',(1.,0.,0.));
#8551=DIRECTION('center_axis',(0.,0.,1.));
#8552=DIRECTION('ref_axis',(1.,0.,0.));
#8553=DIRECTION('center_axis',(0.,0.,1.));
#8554=DIRECTION('ref_axis',(1.,0.,0.));
#8555=DIRECTION('center_axis',(0.,0.,1.));
#8556=DIRECTION('ref_axis',(1.,0.,0.));
#8557=DIRECTION('',(0.,0.,-1.));
#8558=DIRECTION('center_axis',(0.,0.,1.));
#8559=DIRECTION('ref_axis',(1.,0.,0.));
#8560=DIRECTION('center_axis',(0.,0.,1.));
#8561=DIRECTION('ref_axis',(1.,0.,0.));
#8562=DIRECTION('center_axis',(0.,0.,1.));
#8563=DIRECTION('ref_axis',(1.,0.,0.));
#8564=DIRECTION('',(0.,0.,-1.));
#8565=DIRECTION('center_axis',(0.,0.,1.));
#8566=DIRECTION('ref_axis',(1.,0.,0.));
#8567=DIRECTION('axis',(0.,0.,1.));
#8568=DIRECTION('refdir',(1.,0.,0.));
#8569=DIRECTION('center_axis',(-1.,0.,0.));
#8570=DIRECTION('ref_axis',(0.,1.,0.));
#8571=DIRECTION('',(0.,0.,1.));
#8572=DIRECTION('',(0.,-1.,0.));
#8573=DIRECTION('',(0.,0.,-1.));
#8574=DIRECTION('',(0.,1.,0.));
#8575=DIRECTION('center_axis',(1.,0.,0.));
#8576=DIRECTION('ref_axis',(0.,-1.,0.));
#8577=DIRECTION('',(0.,0.,-1.));
#8578=DIRECTION('',(0.,-1.,0.));
#8579=DIRECTION('',(0.,0.,1.));
#8580=DIRECTION('',(0.,1.,0.));
#8581=DIRECTION('center_axis',(0.,0.,1.));
#8582=DIRECTION('ref_axis',(1.,0.,0.));
#8583=DIRECTION('center_axis',(0.,0.,1.));
#8584=DIRECTION('ref_axis',(1.,0.,0.));
#8585=DIRECTION('center_axis',(0.,0.,-1.));
#8586=DIRECTION('ref_axis',(1.,0.,0.));
#8587=DIRECTION('center_axis',(0.,0.,1.));
#8588=DIRECTION('ref_axis',(6.12323399573677E-17,-1.,0.));
#8589=DIRECTION('center_axis',(0.,0.,-1.));
#8590=DIRECTION('ref_axis',(1.,0.,0.));
#8591=DIRECTION('center_axis',(0.,0.,1.));
#8592=DIRECTION('ref_axis',(6.12323399573677E-17,-1.,0.));
#8593=DIRECTION('center_axis',(0.,0.,1.));
#8594=DIRECTION('ref_axis',(1.,0.,0.));
#8595=DIRECTION('center_axis',(0.,0.,1.));
#8596=DIRECTION('ref_axis',(1.,0.,0.));
#8597=DIRECTION('axis',(0.,0.,1.));
#8598=DIRECTION('refdir',(1.,0.,0.));
#8599=DIRECTION('center_axis',(0.,0.,1.));
#8600=DIRECTION('ref_axis',(1.,0.,0.));
#8601=DIRECTION('center_axis',(0.,0.,-1.));
#8602=DIRECTION('ref_axis',(1.,0.,0.));
#8603=DIRECTION('',(0.,0.,1.));
#8604=DIRECTION('center_axis',(0.,0.,-1.));
#8605=DIRECTION('ref_axis',(1.,0.,0.));
#8606=DIRECTION('center_axis',(0.,0.,1.));
#8607=DIRECTION('ref_axis',(1.,0.,0.));
#8608=DIRECTION('center_axis',(0.,0.,1.));
#8609=DIRECTION('ref_axis',(1.,0.,0.));
#8610=DIRECTION('',(0.,0.,-1.));
#8611=DIRECTION('center_axis',(0.,0.,1.));
#8612=DIRECTION('ref_axis',(1.,0.,0.));
#8613=DIRECTION('center_axis',(0.,0.,1.));
#8614=DIRECTION('ref_axis',(1.,0.,0.));
#8615=DIRECTION('center_axis',(0.,0.,1.));
#8616=DIRECTION('ref_axis',(1.,0.,0.));
#8617=DIRECTION('axis',(0.,0.,1.));
#8618=DIRECTION('refdir',(1.,0.,0.));
#8619=DIRECTION('center_axis',(0.,0.,1.));
#8620=DIRECTION('ref_axis',(1.,0.,0.));
#8621=DIRECTION('center_axis',(0.,0.,-1.));
#8622=DIRECTION('ref_axis',(1.,0.,0.));
#8623=DIRECTION('',(0.,0.,1.));
#8624=DIRECTION('center_axis',(0.,0.,-1.));
#8625=DIRECTION('ref_axis',(1.,0.,0.));
#8626=DIRECTION('center_axis',(0.,0.,1.));
#8627=DIRECTION('ref_axis',(1.,0.,0.));
#8628=DIRECTION('center_axis',(0.,0.,1.));
#8629=DIRECTION('ref_axis',(1.,0.,0.));
#8630=DIRECTION('',(0.,0.,-1.));
#8631=DIRECTION('center_axis',(0.,0.,1.));
#8632=DIRECTION('ref_axis',(1.,0.,0.));
#8633=DIRECTION('center_axis',(0.,0.,1.));
#8634=DIRECTION('ref_axis',(1.,0.,0.));
#8635=DIRECTION('center_axis',(0.,0.,1.));
#8636=DIRECTION('ref_axis',(1.,0.,0.));
#8637=DIRECTION('axis',(0.,0.,1.));
#8638=DIRECTION('refdir',(1.,0.,0.));
#8639=DIRECTION('center_axis',(0.,0.,1.));
#8640=DIRECTION('ref_axis',(0.997333822932903,-0.0729742806339326,0.));
#8641=DIRECTION('',(0.,0.,-1.));
#8642=DIRECTION('center_axis',(0.,0.,-1.));
#8643=DIRECTION('ref_axis',(1.,-6.57997986587321E-14,0.));
#8644=DIRECTION('center_axis',(0.,0.,1.));
#8645=DIRECTION('ref_axis',(0.997333822932903,-0.0729742806339326,0.));
#8646=DIRECTION('',(0.,0.,-1.));
#8647=DIRECTION('center_axis',(0.,0.,1.));
#8648=DIRECTION('ref_axis',(0.997333822932903,-0.0729742806339326,0.));
#8649=DIRECTION('',(0.,0.,-1.));
#8650=DIRECTION('center_axis',(0.,0.,1.));
#8651=DIRECTION('ref_axis',(0.997333822932903,-0.0729742806339326,0.));
#8652=DIRECTION('',(0.,0.,-1.));
#8653=DIRECTION('center_axis',(0.,0.,1.));
#8654=DIRECTION('ref_axis',(0.997333822932903,-0.0729742806339326,0.));
#8655=DIRECTION('',(0.,0.,-1.));
#8656=DIRECTION('center_axis',(0.,0.,1.));
#8657=DIRECTION('ref_axis',(0.997333822932903,-0.0729742806339326,0.));
#8658=DIRECTION('',(0.,0.,-1.));
#8659=DIRECTION('center_axis',(0.,0.,1.));
#8660=DIRECTION('ref_axis',(0.997333822932903,-0.0729742806339326,0.));
#8661=DIRECTION('',(0.,0.,-1.));
#8662=DIRECTION('center_axis',(0.,0.,1.));
#8663=DIRECTION('ref_axis',(0.997333822932903,-0.0729742806339326,0.));
#8664=DIRECTION('',(0.,0.,-1.));
#8665=DIRECTION('center_axis',(0.,0.,1.));
#8666=DIRECTION('ref_axis',(0.997333822932903,-0.0729742806339326,0.));
#8667=DIRECTION('',(0.,0.,-1.));
#8668=DIRECTION('center_axis',(0.,0.,1.));
#8669=DIRECTION('ref_axis',(0.997333822932903,-0.0729742806339326,0.));
#8670=DIRECTION('',(0.,0.,-1.));
#8671=DIRECTION('center_axis',(0.,0.,1.));
#8672=DIRECTION('ref_axis',(0.997333822932903,-0.0729742806339326,0.));
#8673=DIRECTION('',(0.,0.,-1.));
#8674=DIRECTION('center_axis',(0.,0.,1.));
#8675=DIRECTION('ref_axis',(0.997333822932903,-0.0729742806339326,0.));
#8676=DIRECTION('',(0.,0.,-1.));
#8677=DIRECTION('center_axis',(0.,0.,1.));
#8678=DIRECTION('ref_axis',(0.997333822932903,-0.0729742806339326,0.));
#8679=DIRECTION('',(0.,0.,-1.));
#8680=DIRECTION('center_axis',(0.,0.,1.));
#8681=DIRECTION('ref_axis',(0.997333822932903,-0.0729742806339326,0.));
#8682=DIRECTION('',(0.,0.,-1.));
#8683=DIRECTION('center_axis',(0.,0.,1.));
#8684=DIRECTION('ref_axis',(0.997333822932903,-0.0729742806339326,0.));
#8685=DIRECTION('',(0.,0.,-1.));
#8686=DIRECTION('center_axis',(0.,0.,1.));
#8687=DIRECTION('ref_axis',(0.997333822932903,-0.0729742806339326,0.));
#8688=DIRECTION('',(0.,0.,-1.));
#8689=DIRECTION('center_axis',(0.,0.,1.));
#8690=DIRECTION('ref_axis',(0.997333822932903,-0.0729742806339326,0.));
#8691=DIRECTION('',(0.,0.,-1.));
#8692=DIRECTION('center_axis',(0.,0.,1.));
#8693=DIRECTION('ref_axis',(0.997333822932903,-0.0729742806339326,0.));
#8694=DIRECTION('',(0.,0.,-1.));
#8695=DIRECTION('center_axis',(0.,0.,1.));
#8696=DIRECTION('ref_axis',(0.997333822932903,-0.0729742806339326,0.));
#8697=DIRECTION('',(0.,0.,-1.));
#8698=DIRECTION('center_axis',(0.,0.,1.));
#8699=DIRECTION('ref_axis',(0.997333822932903,-0.0729742806339326,0.));
#8700=DIRECTION('',(0.,0.,-1.));
#8701=DIRECTION('center_axis',(0.,0.,1.));
#8702=DIRECTION('ref_axis',(0.997333822932903,-0.0729742806339326,0.));
#8703=DIRECTION('',(0.,0.,-1.));
#8704=DIRECTION('center_axis',(0.,0.,1.));
#8705=DIRECTION('ref_axis',(0.997333822932903,-0.0729742806339326,0.));
#8706=DIRECTION('',(0.,0.,-1.));
#8707=DIRECTION('center_axis',(0.,0.,1.));
#8708=DIRECTION('ref_axis',(0.997333822932903,-0.0729742806339326,0.));
#8709=DIRECTION('',(0.,0.,-1.));
#8710=DIRECTION('center_axis',(0.,0.,1.));
#8711=DIRECTION('ref_axis',(0.997333822932903,-0.0729742806339326,0.));
#8712=DIRECTION('',(0.,0.,-1.));
#8713=DIRECTION('center_axis',(0.,0.,1.));
#8714=DIRECTION('ref_axis',(1.,0.,0.));
#8715=DIRECTION('center_axis',(0.,0.,-1.));
#8716=DIRECTION('ref_axis',(1.,0.,0.));
#8717=DIRECTION('center_axis',(0.,0.,-1.));
#8718=DIRECTION('ref_axis',(1.,0.,0.));
#8719=DIRECTION('center_axis',(0.,0.,1.));
#8720=DIRECTION('ref_axis',(0.997333822932903,-0.0729742806339326,0.));
#8721=DIRECTION('center_axis',(0.,0.,-1.));
#8722=DIRECTION('ref_axis',(1.,-6.57997986587321E-14,0.));
#8723=DIRECTION('center_axis',(0.,0.,-1.));
#8724=DIRECTION('ref_axis',(1.,0.,0.));
#8725=DIRECTION('',(0.707106781186547,-8.65956056235493E-17,0.707106781186548));
#8726=DIRECTION('center_axis',(0.,0.,1.));
#8727=DIRECTION('ref_axis',(1.,0.,0.));
#8728=DIRECTION('center_axis',(-1.92296268638356E-16,-1.,0.));
#8729=DIRECTION('ref_axis',(1.,-1.92296268638356E-16,0.));
#8730=DIRECTION('',(1.,-1.92296268638356E-16,0.));
#8731=DIRECTION('',(0.,0.,1.));
#8732=DIRECTION('',(1.,-1.92296268638356E-16,0.));
#8733=DIRECTION('',(0.,0.,1.));
#8734=DIRECTION('center_axis',(-0.866025403784439,-0.5,0.));
#8735=DIRECTION('ref_axis',(0.5,-0.866025403784439,0.));
#8736=DIRECTION('',(0.5,-0.866025403784439,0.));
#8737=DIRECTION('',(0.,0.,1.));
#8738=DIRECTION('',(0.5,-0.866025403784439,0.));
#8739=DIRECTION('center_axis',(-0.866025403784439,0.5,0.));
#8740=DIRECTION('ref_axis',(-0.5,-0.866025403784439,0.));
#8741=DIRECTION('',(-0.5,-0.866025403784439,0.));
#8742=DIRECTION('',(0.,0.,1.));
#8743=DIRECTION('',(-0.5,-0.866025403784439,0.));
#8744=DIRECTION('center_axis',(1.92296268638356E-16,1.,0.));
#8745=DIRECTION('ref_axis',(-1.,1.92296268638356E-16,0.));
#8746=DIRECTION('',(-1.,1.92296268638356E-16,0.));
#8747=DIRECTION('',(0.,0.,1.));
#8748=DIRECTION('',(-1.,1.92296268638356E-16,0.));
#8749=DIRECTION('center_axis',(0.866025403784439,0.5,0.));
#8750=DIRECTION('ref_axis',(-0.5,0.866025403784439,0.));
#8751=DIRECTION('',(-0.5,0.866025403784439,0.));
#8752=DIRECTION('',(0.,0.,1.));
#8753=DIRECTION('',(-0.5,0.866025403784439,0.));
#8754=DIRECTION('center_axis',(0.866025403784439,-0.5,0.));
#8755=DIRECTION('ref_axis',(0.5,0.866025403784439,0.));
#8756=DIRECTION('',(0.5,0.866025403784439,0.));
#8757=DIRECTION('',(0.5,0.866025403784439,0.));
#8758=DIRECTION('center_axis',(0.,0.,1.));
#8759=DIRECTION('ref_axis',(1.,0.,0.));
#8760=DIRECTION('center_axis',(0.,0.,1.));
#8761=DIRECTION('ref_axis',(1.,0.,0.));
#8762=DIRECTION('center_axis',(0.,0.,1.));
#8763=DIRECTION('ref_axis',(1.,0.,0.));
#8764=DIRECTION('center_axis',(0.,0.,1.));
#8765=DIRECTION('ref_axis',(1.,0.,0.));
#8766=DIRECTION('',(0.,0.,-1.));
#8767=DIRECTION('center_axis',(0.,0.,1.));
#8768=DIRECTION('ref_axis',(1.,0.,0.));
#8769=DIRECTION('center_axis',(0.,0.,1.));
#8770=DIRECTION('ref_axis',(1.,0.,0.));
#8771=DIRECTION('center_axis',(0.,0.,1.));
#8772=DIRECTION('ref_axis',(1.,0.,0.));
#8773=DIRECTION('',(0.,0.,1.));
#8774=DIRECTION('',(1.,0.,0.));
#8775=DIRECTION('',(1.,0.,0.));
#8776=DIRECTION('',(0.,1.,0.));
#8777=DIRECTION('',(1.,2.59855450499152E-64,-6.12323399573677E-17));
#8778=DIRECTION('',(-2.29584502165847E-49,1.,-3.74939945665464E-33));
#8779=DIRECTION('',(1.,0.,0.));
#8780=DIRECTION('',(0.,1.,0.));
#8781=DIRECTION('',(1.,0.,0.));
#8782=DIRECTION('',(0.,1.,0.));
#8783=DIRECTION('',(1.,0.,0.));
#8784=DIRECTION('',(0.,1.,0.));
#8785=DIRECTION('',(1.,2.59855450499152E-64,-6.12323399573677E-17));
#8786=DIRECTION('',(-2.29584502165847E-49,1.,-3.74939945665464E-33));
#8787=DIRECTION('',(1.,2.59855450499152E-64,-6.12323399573677E-17));
#8788=DIRECTION('',(-2.29584502165847E-49,1.,-3.74939945665464E-33));
#8789=DIRECTION('',(-1.,-1.22051243050493E-16,5.95146731239587E-17));
#8790=DIRECTION('',(-6.12206869146017E-17,0.014025814092723,-0.999901633431527));
#8791=DIRECTION('',(1.,2.59855450499152E-64,-6.12323399573677E-17));
#8792=DIRECTION('',(-2.29584502165847E-49,1.,-3.74939945665464E-33));
#8793=DIRECTION('',(1.,-4.01390433921683E-19,-6.12323399573678E-17));
#8794=DIRECTION('',(-6.12206869146019E-17,0.014025814092723,-0.999901633431527));
#8795=DIRECTION('',(1.,0.,0.));
#8796=DIRECTION('',(0.,-0.984807753012208,0.17364817766693));
#8797=DIRECTION('',(1.,0.,0.));
#8798=DIRECTION('',(0.,1.,0.));
#8799=DIRECTION('',(1.,2.59855450499152E-64,-6.12323399573677E-17));
#8800=DIRECTION('',(-2.29584502165847E-49,1.,-3.74939945665464E-33));
#8801=DIRECTION('',(1.,0.,0.));
#8802=DIRECTION('',(0.,1.,0.));
#8803=DIRECTION('',(1.,0.,0.));
#8804=DIRECTION('',(0.,1.,0.));
#8805=DIRECTION('',(1.,2.59855450499152E-64,-6.12323399573677E-17));
#8806=DIRECTION('',(-2.29584502165847E-49,1.,-3.74939945665464E-33));
#8807=DIRECTION('',(1.,2.59855450499152E-64,-6.12323399573677E-17));
#8808=DIRECTION('',(-2.29584502165847E-49,1.,-3.74939945665464E-33));
#8809=DIRECTION('',(1.,0.,0.));
#8810=DIRECTION('',(0.,-0.984807753012208,0.17364817766693));
#8811=DIRECTION('',(-1.,2.76668533537974E-63,-6.12323399573677E-17));
#8812=DIRECTION('',(2.29584502165849E-49,1.,-3.74939945665464E-33));
#8813=DIRECTION('',(-1.,2.76668533537974E-63,-6.12323399573677E-17));
#8814=DIRECTION('',(2.29584502165849E-49,1.,-3.74939945665464E-33));
#8815=CARTESIAN_POINT('',(0.,0.,0.));
#8816=CARTESIAN_POINT('',(0.,0.,0.));
#8817=CARTESIAN_POINT('Origin',(160.,-50.,6.));
#8818=CARTESIAN_POINT('',(155.5,-50.,12.));
#8819=CARTESIAN_POINT('Origin',(160.,-50.,12.));
#8820=CARTESIAN_POINT('',(155.5,-50.,0.));
#8821=CARTESIAN_POINT('',(155.5,-50.,6.));
#8822=CARTESIAN_POINT('Origin',(160.,-50.,0.));
#8823=CARTESIAN_POINT('Origin',(40.,-50.,6.));
#8824=CARTESIAN_POINT('',(35.5,-50.,12.));
#8825=CARTESIAN_POINT('Origin',(40.,-50.,12.));
#8826=CARTESIAN_POINT('',(35.5,-50.,0.));
#8827=CARTESIAN_POINT('',(35.5,-50.,6.));
#8828=CARTESIAN_POINT('Origin',(40.,-50.,0.));
#8829=CARTESIAN_POINT('Origin',(40.,50.,6.));
#8830=CARTESIAN_POINT('',(35.5,50.,12.));
#8831=CARTESIAN_POINT('Origin',(40.,50.,12.));
#8832=CARTESIAN_POINT('',(35.5,50.,0.));
#8833=CARTESIAN_POINT('',(35.5,50.,6.));
#8834=CARTESIAN_POINT('Origin',(40.,50.,0.));
#8835=CARTESIAN_POINT('Origin',(160.,50.,6.));
#8836=CARTESIAN_POINT('',(155.5,50.,12.));
#8837=CARTESIAN_POINT('Origin',(160.,50.,12.));
#8838=CARTESIAN_POINT('',(155.5,50.,0.));
#8839=CARTESIAN_POINT('',(155.5,50.,6.));
#8840=CARTESIAN_POINT('Origin',(160.,50.,0.));
#8841=CARTESIAN_POINT('Origin',(200.,65.,0.));
#8842=CARTESIAN_POINT('',(205.,65.,0.));
#8843=CARTESIAN_POINT('',(-5.,65.,0.));
#8844=CARTESIAN_POINT('',(150.,65.,0.));
#8845=CARTESIAN_POINT('',(-5.,65.,12.));
#8846=CARTESIAN_POINT('',(-5.,65.,0.));
#8847=CARTESIAN_POINT('',(205.,65.,12.));
#8848=CARTESIAN_POINT('',(150.,65.,12.));
#8849=CARTESIAN_POINT('',(205.,65.,0.));
#8850=CARTESIAN_POINT('Origin',(205.,-60.,0.));
#8851=CARTESIAN_POINT('',(205.,-65.,0.));
#8852=CARTESIAN_POINT('',(205.,-30.,0.));
#8853=CARTESIAN_POINT('',(205.,-65.,12.));
#8854=CARTESIAN_POINT('',(205.,-30.,12.));
#8855=CARTESIAN_POINT('',(205.,-65.,0.));
#8856=CARTESIAN_POINT('Origin',(0.,-65.,0.));
#8857=CARTESIAN_POINT('',(-5.,-65.,0.));
#8858=CARTESIAN_POINT('',(50.,-65.,0.));
#8859=CARTESIAN_POINT('',(-5.,-65.,12.));
#8860=CARTESIAN_POINT('',(50.,-65.,12.));
#8861=CARTESIAN_POINT('',(-5.,-65.,0.));
#8862=CARTESIAN_POINT('Origin',(-5.,60.,0.));
#8863=CARTESIAN_POINT('',(-5.,30.,0.));
#8864=CARTESIAN_POINT('',(-5.,30.,12.));
#8865=CARTESIAN_POINT('Origin',(100.,0.,12.));
#8866=CARTESIAN_POINT('Origin',(100.,0.,0.));
#8867=CARTESIAN_POINT('',(0.,0.,0.));
#8868=CARTESIAN_POINT('Origin',(-15.,0.,10.));
#8869=CARTESIAN_POINT('',(-18.5,4.28626379701574E-16,20.));
#8870=CARTESIAN_POINT('Origin',(-15.,0.,20.));
#8871=CARTESIAN_POINT('',(-18.5,4.28626379701574E-16,0.));
#8872=CARTESIAN_POINT('',(-18.5,4.28626379701574E-16,10.));
#8873=CARTESIAN_POINT('Origin',(-15.,0.,0.));
#8874=CARTESIAN_POINT('Origin',(15.,0.,10.));
#8875=CARTESIAN_POINT('',(11.5,4.28626379701574E-16,20.));
#8876=CARTESIAN_POINT('Origin',(15.,0.,20.));
#8877=CARTESIAN_POINT('',(11.5,4.28626379701574E-16,0.));
#8878=CARTESIAN_POINT('',(11.5,4.28626379701574E-16,10.));
#8879=CARTESIAN_POINT('Origin',(15.,0.,0.));
#8880=CARTESIAN_POINT('Origin',(0.,0.,10.));
#8881=CARTESIAN_POINT('',(-7.,8.57252759403147E-16,20.));
#8882=CARTESIAN_POINT('Origin',(0.,0.,20.));
#8883=CARTESIAN_POINT('',(-7.,8.57252759403147E-16,0.));
#8884=CARTESIAN_POINT('',(-7.,8.57252759403147E-16,10.));
#8885=CARTESIAN_POINT('Origin',(0.,0.,0.));
#8886=CARTESIAN_POINT('Origin',(-35.,0.,10.));
#8887=CARTESIAN_POINT('',(-43.,9.79717439317883E-16,20.));
#8888=CARTESIAN_POINT('Origin',(-35.,0.,20.));
#8889=CARTESIAN_POINT('',(-43.,9.79717439317883E-16,0.));
#8890=CARTESIAN_POINT('',(-43.,9.79717439317883E-16,10.));
#8891=CARTESIAN_POINT('Origin',(-35.,0.,0.));
#8892=CARTESIAN_POINT('Origin',(35.,0.,10.));
#8893=CARTESIAN_POINT('',(27.,9.79717439317883E-16,20.));
#8894=CARTESIAN_POINT('Origin',(35.,0.,20.));
#8895=CARTESIAN_POINT('',(27.,9.79717439317883E-16,0.));
#8896=CARTESIAN_POINT('',(27.,9.79717439317883E-16,10.));
#8897=CARTESIAN_POINT('Origin',(35.,0.,0.));
#8898=CARTESIAN_POINT('Origin',(50.,33.,0.));
#8899=CARTESIAN_POINT('',(50.,33.,0.));
#8900=CARTESIAN_POINT('',(-50.,33.,0.));
#8901=CARTESIAN_POINT('',(25.,33.,0.));
#8902=CARTESIAN_POINT('',(-50.,33.,20.));
#8903=CARTESIAN_POINT('',(-50.,33.,0.));
#8904=CARTESIAN_POINT('',(50.,33.,20.));
#8905=CARTESIAN_POINT('',(25.,33.,20.));
#8906=CARTESIAN_POINT('',(50.,33.,0.));
#8907=CARTESIAN_POINT('Origin',(50.,-30.,0.));
#8908=CARTESIAN_POINT('',(50.,-30.,0.));
#8909=CARTESIAN_POINT('',(50.,-30.,0.));
#8910=CARTESIAN_POINT('',(50.,-30.,20.));
#8911=CARTESIAN_POINT('',(50.,-30.,20.));
#8912=CARTESIAN_POINT('',(50.,-30.,0.));
#8913=CARTESIAN_POINT('Origin',(-50.,-30.,0.));
#8914=CARTESIAN_POINT('',(-50.,-30.,0.));
#8915=CARTESIAN_POINT('',(-50.,-30.,0.));
#8916=CARTESIAN_POINT('',(-50.,-30.,20.));
#8917=CARTESIAN_POINT('',(-50.,-30.,20.));
#8918=CARTESIAN_POINT('',(-50.,-30.,0.));
#8919=CARTESIAN_POINT('Origin',(-50.,30.,0.));
#8920=CARTESIAN_POINT('',(-50.,30.,0.));
#8921=CARTESIAN_POINT('',(-50.,30.,20.));
#8922=CARTESIAN_POINT('Origin',(0.,0.,20.));
#8923=CARTESIAN_POINT('Origin',(0.,0.,0.));
#8924=CARTESIAN_POINT('',(0.,0.,0.));
#8925=CARTESIAN_POINT('Origin',(0.,0.,0.));
#8926=CARTESIAN_POINT('',(-5.,-6.12323399573677E-16,0.));
#8927=CARTESIAN_POINT('Origin',(0.,0.,0.));
#8928=CARTESIAN_POINT('',(-5.,-6.12323399573677E-16,20.));
#8929=CARTESIAN_POINT('',(-5.,-6.12323399573677E-16,0.));
#8930=CARTESIAN_POINT('Origin',(0.,0.,20.));
#8931=CARTESIAN_POINT('Origin',(0.,0.,0.));
#8932=CARTESIAN_POINT('',(-7.,-8.57252759403147E-16,20.));
#8933=CARTESIAN_POINT('Origin',(0.,0.,20.));
#8934=CARTESIAN_POINT('',(-7.,-8.57252759403147E-16,0.));
#8935=CARTESIAN_POINT('',(-7.,-8.57252759403147E-16,0.));
#8936=CARTESIAN_POINT('Origin',(0.,0.,0.));
#8937=CARTESIAN_POINT('Origin',(0.,0.,20.));
#8938=CARTESIAN_POINT('Origin',(0.,0.,0.));
#8939=CARTESIAN_POINT('',(0.,0.,0.));
#8940=CARTESIAN_POINT('Origin',(0.,0.,-3.69717978381041));
#8941=CARTESIAN_POINT('',(3.0991757505326,6.01559628526639,1.04590194808422));
#8942=CARTESIAN_POINT('',(3.09917575053259,6.01559628526639,0.651392015122069));
#8943=CARTESIAN_POINT('',(3.09917575053259,6.01559628526639,-3.69717978381041));
#8944=CARTESIAN_POINT('',(-3.92961407736517,-5.50997186835842,0.000232560444541066));
#8945=CARTESIAN_POINT('Ctrl Pts',(-3.92889204432313,-5.50963667622961,0.00025114599476872));
#8946=CARTESIAN_POINT('Ctrl Pts',(-3.79038240896438,-5.60840714629906,0.00830193321678136));
#8947=CARTESIAN_POINT('Ctrl Pts',(-3.6479042510226,-5.70212321738183,0.0163527204387951));
#8948=CARTESIAN_POINT('Ctrl Pts',(-3.50187062022184,-5.79043963436517,0.0244035076608076));
#8949=CARTESIAN_POINT('Ctrl Pts',(-3.35600620203666,-5.87865371703119,0.0324449662456032));
#8950=CARTESIAN_POINT('Ctrl Pts',(-3.2065948255179,-5.96148040292313,0.0404864248303983));
#8951=CARTESIAN_POINT('Ctrl Pts',(-3.05408187353037,-6.03861514834098,0.0485278834151939));
#8952=CARTESIAN_POINT('Ctrl Pts',(-2.90171192392777,-6.11567756906503,0.0565618019993478));
#8953=CARTESIAN_POINT('Ctrl Pts',(-2.74624651834304,-6.18705850218575,0.0645957205835019));
#8954=CARTESIAN_POINT('Ctrl Pts',(-2.58815912298106,-6.25249720944599,0.0726296391676557));
#8955=CARTESIAN_POINT('Ctrl Pts',(-2.43018506105976,-6.31788900345404,0.0806577982057483));
#8956=CARTESIAN_POINT('Ctrl Pts',(-2.26959309568702,-6.37734690791538,0.0886859572438399));
#8957=CARTESIAN_POINT('Ctrl Pts',(-2.10688022797297,-6.43065663093409,0.0967141162819325));
#8958=CARTESIAN_POINT('Ctrl Pts',(-1.94010051972161,-6.48529877557163,0.104942930886329));
#8959=CARTESIAN_POINT('Ctrl Pts',(-1.77109285526961,-6.53348118862384,0.113171745490725));
#8960=CARTESIAN_POINT('Ctrl Pts',(-1.6004136702066,-6.57502586186669,0.121400560095122));
#8961=CARTESIAN_POINT('Ctrl Pts',(-1.43400115166054,-6.61553199449185,0.129423669430104));
#8962=CARTESIAN_POINT('Ctrl Pts',(-1.26600007280295,-6.64972821013253,0.137446778765087));
#8963=CARTESIAN_POINT('Ctrl Pts',(-1.09694043186167,-6.67750033238091,0.145469888100069));
#8964=CARTESIAN_POINT('Ctrl Pts',(-0.927881956037865,-6.70527226323065,
0.153492942141754));
#8965=CARTESIAN_POINT('Ctrl Pts',(-0.757765302814855,-6.72662012752097,
0.161515996183439));
#8966=CARTESIAN_POINT('Ctrl Pts',(-0.587129013611443,-6.74148118156356,
0.169539050225124));
#8967=CARTESIAN_POINT('Ctrl Pts',(-0.416459841795382,-6.75634509941833,
0.177563650356328));
#8968=CARTESIAN_POINT('Ctrl Pts',(-0.245271208442629,-6.76471968690886,
0.185588250487533));
#8969=CARTESIAN_POINT('Ctrl Pts',(-0.0741049318708623,-6.76659422893618,
0.193612850618737));
#8970=CARTESIAN_POINT('Ctrl Pts',(0.104700424075701,-6.76855243099061,0.201995585299463));
#8971=CARTESIAN_POINT('Ctrl Pts',(0.283480924655757,-6.76341705142668,0.210378319980189));
#8972=CARTESIAN_POINT('Ctrl Pts',(0.461622104329729,-6.75123648177089,0.218761054660915));
#8973=CARTESIAN_POINT('Ctrl Pts',(0.632409631117175,-6.73955872500415,0.22679775076036));
#8974=CARTESIAN_POINT('Ctrl Pts',(0.80260919751235,-6.72140587627492,0.234834446859806));
#8975=CARTESIAN_POINT('Ctrl Pts',(0.97168796157606,-6.69687326334672,0.242871142959252));
#8976=CARTESIAN_POINT('Ctrl Pts',(1.14087936821317,-6.67232430645796,0.250913193215));
#8977=CARTESIAN_POINT('Ctrl Pts',(1.30894811887766,-6.64138719044629,0.258955243470749));
#8978=CARTESIAN_POINT('Ctrl Pts',(1.47537431408813,-6.60420772184893,0.266997293726497));
#8979=CARTESIAN_POINT('Ctrl Pts',(1.64201671727433,-6.5669799525761,0.275049791588792));
#8980=CARTESIAN_POINT('Ctrl Pts',(1.80701194770951,-6.52349374575839,0.283102289451085));
#8981=CARTESIAN_POINT('Ctrl Pts',(1.96985743028625,-6.47394398372013,0.291154787313379));
#8982=CARTESIAN_POINT('Ctrl Pts',(1.99042338587475,-6.46768628354095,0.292171747138067));
#8983=CARTESIAN_POINT('Ctrl Pts',(2.010955083382,-6.46133193442697,0.293188706962756));
#8984=CARTESIAN_POINT('Ctrl Pts',(2.03145153667316,-6.45488138188056,0.294205666787444));
#8985=CARTESIAN_POINT('Ctrl Pts',(2.19747654241461,-6.40263073108063,0.302443226639107));
#8986=CARTESIAN_POINT('Ctrl Pts',(2.3617135116338,-6.3438984024491,0.31068078649077));
#8987=CARTESIAN_POINT('Ctrl Pts',(2.52362070621982,-6.27882373786194,0.318918346342433));
#8988=CARTESIAN_POINT('Ctrl Pts',(2.68534576630942,-6.21382227781208,0.327146639503884));
#8989=CARTESIAN_POINT('Ctrl Pts',(2.84474594209345,-6.14249282172973,0.335374932665337));
#8990=CARTESIAN_POINT('Ctrl Pts',(3.0012937929869,-6.06502469641949,0.343603225826788));
#8991=CARTESIAN_POINT('Ctrl Pts',(3.15769669554932,-5.98762829918093,0.351823900376077));
#8992=CARTESIAN_POINT('Ctrl Pts',(3.3112522146734,-5.90410471035315,0.360044574925363));
#8993=CARTESIAN_POINT('Ctrl Pts',(3.4614519757946,-5.8146916701806,0.368265249474652));
#8994=CARTESIAN_POINT('Ctrl Pts',(3.6115425504235,-5.72534362808894,0.376479948071571));
#8995=CARTESIAN_POINT('Ctrl Pts',(3.75828192028324,-5.63011484475562,0.38469464666849));
#8996=CARTESIAN_POINT('Ctrl Pts',(3.90118536821696,-5.52928944104122,0.392909345265409));
#8997=CARTESIAN_POINT('Ctrl Pts',(4.04401335933728,-5.42851727581604,0.401119706283438));
#8998=CARTESIAN_POINT('Ctrl Pts',(4.18300917239897,-5.3221545832726,0.409330067301468));
#8999=CARTESIAN_POINT('Ctrl Pts',(4.31771611726011,-5.21052939064278,0.417540428319497));
#9000=CARTESIAN_POINT('Ctrl Pts',(4.45239570423667,-5.09892686818146,0.425749121879999));
#9001=CARTESIAN_POINT('Ctrl Pts',(4.58278787946917,-4.98206419803764,0.433957815440499));
#9002=CARTESIAN_POINT('Ctrl Pts',(4.70846792674628,-4.86031056443944,0.442166509001001));
#9003=CARTESIAN_POINT('Ctrl Pts',(4.83413768807839,-4.73856689543948,0.450374530743085));
#9004=CARTESIAN_POINT('Ctrl Pts',(4.95509583218291,-4.61193330837405,0.45858255248517));
#9005=CARTESIAN_POINT('Ctrl Pts',(5.07095353957911,-4.48081680047624,0.466790574227254));
#9006=CARTESIAN_POINT('Ctrl Pts',(5.18682264631825,-4.34968739190852,0.474999403563902));
#9007=CARTESIAN_POINT('Ctrl Pts',(5.29759007971564,-4.21407445167993,0.483208232900549));
#9008=CARTESIAN_POINT('Ctrl Pts',(5.40290641236495,-4.07441913642003,0.491417062237197));
#9009=CARTESIAN_POINT('Ctrl Pts',(5.50825208868729,-3.93472490981746,0.499628178751893));
#9010=CARTESIAN_POINT('Ctrl Pts',(5.60814342364821,-3.79098635003299,0.507839295266589));
#9011=CARTESIAN_POINT('Ctrl Pts',(5.70227349625691,-3.64367478980851,0.516050411781285));
#9012=CARTESIAN_POINT('Ctrl Pts',(5.7964993705027,-3.49621330206095,0.524269885225734));
#9013=CARTESIAN_POINT('Ctrl Pts',(5.88495207482346,-3.34517185030215,0.532489358670184));
#9014=CARTESIAN_POINT('Ctrl Pts',(5.96736947095795,-3.19104851061201,0.540708832114634));
#9015=CARTESIAN_POINT('Ctrl Pts',(6.04982999095192,-3.0368445278349,0.54893260629454));
#9016=CARTESIAN_POINT('Ctrl Pts',(6.12624875071037,-2.8795557634772,0.557156380474448));
#9017=CARTESIAN_POINT('Ctrl Pts',(6.19641126214192,-2.71970154068435,0.565380154654354));
#9018=CARTESIAN_POINT('Ctrl Pts',(6.26667455633474,-2.55961770025602,0.573615741619366));
#9019=CARTESIAN_POINT('Ctrl Pts',(6.33066351158858,-2.3969613695239,0.581851328584376));
#9020=CARTESIAN_POINT('Ctrl Pts',(6.38821271033491,-2.23226955529915,0.590086915549388));
#9021=CARTESIAN_POINT('Ctrl Pts',(6.44027281862399,-2.08328618333845,0.597536985377683));
#9022=CARTESIAN_POINT('Ctrl Pts',(6.48706363804092,-1.93263748079221,0.604987055205977));
#9023=CARTESIAN_POINT('Ctrl Pts',(6.52849874228747,-1.78072827010495,0.612437125034272));
#9024=CARTESIAN_POINT('Ctrl Pts',(6.57393130962719,-1.6141635764817,0.620605942400958));
#9025=CARTESIAN_POINT('Ctrl Pts',(6.61305351986596,-1.44560879889593,0.628774759767645));
#9026=CARTESIAN_POINT('Ctrl Pts',(6.64568796898957,-1.27558630395096,0.636943577134332));
#9027=CARTESIAN_POINT('Ctrl Pts',(6.67828553118715,-1.10575598651667,0.645103161234637));
#9028=CARTESIAN_POINT('Ctrl Pts',(6.704409862946,-0.934461608373648,0.653262745334943));
#9029=CARTESIAN_POINT('Ctrl Pts',(6.72393320152799,-0.762240973308022,0.661422329435248));
#9030=CARTESIAN_POINT('Ctrl Pts',(6.74343853720231,-0.590179146746397,0.669574389400343));
#9031=CARTESIAN_POINT('Ctrl Pts',(6.75635495829404,-0.417193123190283,0.677726449365437));
#9032=CARTESIAN_POINT('Ctrl Pts',(6.76260566212413,-0.24383120925473,0.685878509330532));
#9033=CARTESIAN_POINT('Ctrl Pts',(6.76885190277121,-0.0705930807313588,
0.69402474848943));
#9034=CARTESIAN_POINT('Ctrl Pts',(6.76844189092621,0.103020041389537,0.70217098764833));
#9035=CARTESIAN_POINT('Ctrl Pts',(6.76135060250933,0.276454390355338,0.710317226807228));
#9036=CARTESIAN_POINT('Ctrl Pts',(6.75426290225783,0.449800982190343,0.718459343999632));
#9037=CARTESIAN_POINT('Ctrl Pts',(6.74050067365104,0.622968618117431,0.726601461192037));
#9038=CARTESIAN_POINT('Ctrl Pts',(6.72009098117132,0.795403171215613,0.734743578384441));
#9039=CARTESIAN_POINT('Ctrl Pts',(6.69962758385231,0.968291458243047,0.742907120255134));
#9040=CARTESIAN_POINT('Ctrl Pts',(6.67248169599599,1.14044243079594,0.751070662125828));
#9041=CARTESIAN_POINT('Ctrl Pts',(6.63873304122902,1.3113018749678,0.759234203996522));
#9042=CARTESIAN_POINT('Ctrl Pts',(6.60507898639243,1.48168238770861,0.767374862866457));
#9043=CARTESIAN_POINT('Ctrl Pts',(6.56485921978189,1.65077824737774,0.775515521736392));
#9044=CARTESIAN_POINT('Ctrl Pts',(6.51820410356284,1.81804957696335,0.783656180606327));
#9045=CARTESIAN_POINT('Ctrl Pts',(6.47154210487086,1.98534558209348,0.791798040370587));
#9046=CARTESIAN_POINT('Ctrl Pts',(6.41844296343186,2.15081617013514,0.799939900134848));
#9047=CARTESIAN_POINT('Ctrl Pts',(6.35908705673205,2.31393621452774,0.808081759899108));
#9048=CARTESIAN_POINT('Ctrl Pts',(6.29971120841759,2.47711106184132,0.816226355058021));
#9049=CARTESIAN_POINT('Ctrl Pts',(6.23407453305535,2.6379334507201,0.824370950216934));
#9050=CARTESIAN_POINT('Ctrl Pts',(6.16240571227708,2.79589785888091,0.832515545375847));
#9051=CARTESIAN_POINT('Ctrl Pts',(6.09043044989734,2.95453769138503,0.840694965201285));
#9052=CARTESIAN_POINT('Ctrl Pts',(6.01237149959967,3.11029471312419,0.848874385026722));
#9053=CARTESIAN_POINT('Ctrl Pts',(5.92850683918757,3.26268227961385,0.857053804852159));
#9054=CARTESIAN_POINT('Ctrl Pts',(5.84485364385698,3.41468560023628,0.865212600237317));
#9055=CARTESIAN_POINT('Ctrl Pts',(5.75542421689786,3.5633361542509,0.873371395622476));
#9056=CARTESIAN_POINT('Ctrl Pts',(5.66053745414438,3.70818078445868,0.881530191007635));
#9057=CARTESIAN_POINT('Ctrl Pts',(5.56529089813482,3.85357463902209,0.889719923053211));
#9058=CARTESIAN_POINT('Ctrl Pts',(5.46454576871104,3.99513336137898,0.897909655098788));
#9059=CARTESIAN_POINT('Ctrl Pts',(5.35866457522277,4.13243305695962,0.906099387144364));
#9060=CARTESIAN_POINT('Ctrl Pts',(5.25278338173449,4.26973275254026,0.91428911918994));
#9061=CARTESIAN_POINT('Ctrl Pts',(5.14176640573001,4.40277318243318,0.922478851235517));
#9062=CARTESIAN_POINT('Ctrl Pts',(5.02601218914608,4.53116877577464,0.930668583281093));
#9063=CARTESIAN_POINT('Ctrl Pts',(4.90985584864106,4.66001040849997,0.938886766015206));
#9064=CARTESIAN_POINT('Ctrl Pts',(4.78856616752597,4.78457774688426,0.947104948749321));
#9065=CARTESIAN_POINT('Ctrl Pts',(4.66248925298099,4.90443503023914,0.955323131483434));
#9066=CARTESIAN_POINT('Ctrl Pts',(4.53660699102111,5.02410726361772,0.963528626006388));
#9067=CARTESIAN_POINT('Ctrl Pts',(4.40595248216271,5.13908368708086,0.971734120529341));
#9068=CARTESIAN_POINT('Ctrl Pts',(4.27091134853337,5.24896230249074,0.979939615052295));
#9069=CARTESIAN_POINT('Ctrl Pts',(4.13599006363772,5.35874340085109,0.988137827215413));
#9070=CARTESIAN_POINT('Ctrl Pts',(3.99669017928062,5.46343547027293,0.99633603937853));
#9071=CARTESIAN_POINT('Ctrl Pts',(3.8534339375994,5.56267344795263,1.00453425154165));
#9072=CARTESIAN_POINT('Ctrl Pts',(3.71030282712495,5.66182474342038,1.01272530274501));
#9073=CARTESIAN_POINT('Ctrl Pts',(3.5632225385651,5.75553123438426,1.02091635394837));
#9074=CARTESIAN_POINT('Ctrl Pts',(3.41264795723443,5.8434683981334,1.02910740515173));
#9075=CARTESIAN_POINT('Ctrl Pts',(3.30973763034577,5.9035691281976,1.03470558612923));
#9076=CARTESIAN_POINT('Ctrl Pts',(3.20519580383802,5.96097580166128,1.04030376710673));
#9077=CARTESIAN_POINT('Ctrl Pts',(3.0991757505326,6.01559628526639,1.04590194808422));
#9078=CARTESIAN_POINT('',(3.92888236737287,-5.50964357679755,0.));
#9079=CARTESIAN_POINT('Origin',(0.,0.,0.));
#9080=CARTESIAN_POINT('Ctrl Pts',(3.92888236737286,-5.50964357679756,-4.44089209850063E-16));
#9081=CARTESIAN_POINT('Ctrl Pts',(4.08032704765413,-5.40164959756899,0.00874944781300858));
#9082=CARTESIAN_POINT('Ctrl Pts',(4.2273164115086,-5.28740798007164,0.0174988956260169));
#9083=CARTESIAN_POINT('Ctrl Pts',(4.36935121050034,-5.16730674522998,0.0262483434390259));
#9084=CARTESIAN_POINT('Ctrl Pts',(4.51138486261615,-5.04720648015923,0.0349977206036361));
#9085=CARTESIAN_POINT('Ctrl Pts',(4.64846381108604,-4.9212468774719,0.0437470977682466));
#9086=CARTESIAN_POINT('Ctrl Pts',(4.78012247564787,-4.78985575125245,0.0524964749328567));
#9087=CARTESIAN_POINT('Ctrl Pts',(4.91178012085318,-4.65846564231811,0.0612457843561254));
#9088=CARTESIAN_POINT('Ctrl Pts',(5.03801736328267,-4.52164429644009,0.0699950937793945));
#9089=CARTESIAN_POINT('Ctrl Pts',(5.15840545249789,-4.37985641176056,0.0787444032026632));
#9090=CARTESIAN_POINT('Ctrl Pts',(5.27879264960788,-4.23806957776398,0.0874936477914066));
#9091=CARTESIAN_POINT('Ctrl Pts',(5.39333059476267,-4.09131649706054,0.0962428923801495));
#9092=CARTESIAN_POINT('Ctrl Pts',(5.50163027861608,-3.94009559242092,0.104992136968893));
#9093=CARTESIAN_POINT('Ctrl Pts',(5.60992919591457,-3.78887575813648,0.113741319629695));
#9094=CARTESIAN_POINT('Ctrl Pts',(5.71198977342317,-3.63318839617191,0.122490502290497));
#9095=CARTESIAN_POINT('Ctrl Pts',(5.80746538403055,-3.47356226564127,0.131239684951299));
#9096=CARTESIAN_POINT('Ctrl Pts',(5.90294035056408,-3.3139372119408,0.139988808590537));
#9097=CARTESIAN_POINT('Ctrl Pts',(5.99183029200292,-3.15037368876134,0.148737932229775));
#9098=CARTESIAN_POINT('Ctrl Pts',(6.07383331657755,-2.98342719744131,0.157487055869014));
#9099=CARTESIAN_POINT('Ctrl Pts',(6.15583581519874,-2.81648177688769,0.166236123392861));
#9100=CARTESIAN_POINT('Ctrl Pts',(6.23095135902003,-2.64615368880009,0.174985190916708));
#9101=CARTESIAN_POINT('Ctrl Pts',(6.2989248407314,-2.4730214012048,0.183734258440555));
#9102=CARTESIAN_POINT('Ctrl Pts',(6.36689790904675,-2.29989016655244,0.192483272754981));
#9103=CARTESIAN_POINT('Ctrl Pts',(6.4277288974603,-2.12395503322982,0.201232287069408));
#9104=CARTESIAN_POINT('Ctrl Pts',(6.48121121436041,-1.94581350464243,0.209981301383834));
#9105=CARTESIAN_POINT('Ctrl Pts',(6.53742627953525,-1.75856960384828,0.219177357920047));
#9106=CARTESIAN_POINT('Ctrl Pts',(6.5855219277559,-1.56888825318548,0.22837341445626));
#9107=CARTESIAN_POINT('Ctrl Pts',(6.62531771926539,-1.37748107747006,0.237569470992473));
#9108=CARTESIAN_POINT('Ctrl Pts',(6.6631831972433,-1.19535819658355,0.246319468493404));
#9109=CARTESIAN_POINT('Ctrl Pts',(6.69353484894203,-1.01167324970243,0.255069465994336));
#9110=CARTESIAN_POINT('Ctrl Pts',(6.71626957222991,-0.827050199890335,0.263819463495267));
#9111=CARTESIAN_POINT('Ctrl Pts',(6.73900383447862,-0.642430894063015,0.272569283554338));
#9112=CARTESIAN_POINT('Ctrl Pts',(6.75412144238072,-0.456873807891365,0.281319103613409));
#9113=CARTESIAN_POINT('Ctrl Pts',(6.76157104471273,-0.271009238407965,0.29006892367248));
#9114=CARTESIAN_POINT('Ctrl Pts',(6.76902050587629,-0.085148191020104,0.298818577924252));
#9115=CARTESIAN_POINT('Ctrl Pts',(6.76880224076615,0.101020041610374,0.307568232176024));
#9116=CARTESIAN_POINT('Ctrl Pts',(6.76091699075328,0.286863110461421,0.316317886427796));
#9117=CARTESIAN_POINT('Ctrl Pts',(6.75303187968407,0.472702904626974,0.32506738650451));
#9118=CARTESIAN_POINT('Ctrl Pts',(6.73748006620785,0.658217260123046,0.333816886581225));
#9119=CARTESIAN_POINT('Ctrl Pts',(6.71431437259024,0.842776071105572,0.342566386657939));
#9120=CARTESIAN_POINT('Ctrl Pts',(6.69114905638314,1.02733187529549,0.351315744189673));
#9121=CARTESIAN_POINT('Ctrl Pts',(6.66037014395277,1.21093188176617,0.360065101721407));
#9122=CARTESIAN_POINT('Ctrl Pts',(6.62208217352349,1.39295250712377,0.368814459253141));
#9123=CARTESIAN_POINT('Ctrl Pts',(6.58379477599824,1.57497040890141,0.377563685867982));
#9124=CARTESIAN_POINT('Ctrl Pts',(6.53799860430444,1.75540869642656,0.386312912482823));
#9125=CARTESIAN_POINT('Ctrl Pts',(6.48484919699013,1.9336545431634,0.395062139097663));
#9126=CARTESIAN_POINT('Ctrl Pts',(6.43170051433729,2.11189795962108,0.403811246421853));
#9127=CARTESIAN_POINT('Ctrl Pts',(6.37119887857043,2.28794872050952,0.412560353746043));
#9128=CARTESIAN_POINT('Ctrl Pts',(6.30354976713205,2.46120891703438,0.421309461070233));
#9129=CARTESIAN_POINT('Ctrl Pts',(6.23590148818025,2.63446698142792,0.430058460728346));
#9130=CARTESIAN_POINT('Ctrl Pts',(6.16110601378106,2.80493428327179,0.438807460386459));
#9131=CARTESIAN_POINT('Ctrl Pts',(6.07941736028839,2.97203189071453,0.447556460044571));
#9132=CARTESIAN_POINT('Ctrl Pts',(5.99771978801279,3.13914774190625,0.456306414920151));
#9133=CARTESIAN_POINT('Ctrl Pts',(5.90912765640074,3.30289290492367,0.465056369795731));
#9134=CARTESIAN_POINT('Ctrl Pts',(5.81394190290397,3.46271115596687,0.473806324671311));
#9135=CARTESIAN_POINT('Ctrl Pts',(5.71875982413551,3.6225232370883,0.482555941747317));
#9136=CARTESIAN_POINT('Ctrl Pts',(5.6169847795414,3.77840846333365,0.491305558823323));
#9137=CARTESIAN_POINT('Ctrl Pts',(5.50896246077205,3.92983735106231,0.500055175899329));
#9138=CARTESIAN_POINT('Ctrl Pts',(5.40094373802236,4.08126119778403,0.508804501704092));
#9139=CARTESIAN_POINT('Ctrl Pts',(5.28667832369811,4.22822876953944,0.517553827508855));
#9140=CARTESIAN_POINT('Ctrl Pts',(5.16655430873675,4.37024090581672,0.526303153313617));
#9141=CARTESIAN_POINT('Ctrl Pts',(5.04643365420422,4.51224906935235,0.535052234358939));
#9142=CARTESIAN_POINT('Ctrl Pts',(4.9204549120583,4.64930185603789,0.543801315404261));
#9143=CARTESIAN_POINT('Ctrl Pts',(4.78904593245666,4.78093380594422,0.552550396449583));
#9144=CARTESIAN_POINT('Ctrl Pts',(4.65762507998344,4.91257764886762,0.561300267979057));
#9145=CARTESIAN_POINT('Ctrl Pts',(4.52077321070996,5.0387994720143,0.57005013950853));
#9146=CARTESIAN_POINT('Ctrl Pts',(4.37895518611181,5.15917052228597,0.578800011038004));
#9147=CARTESIAN_POINT('Ctrl Pts',(4.23714700417698,5.27953321838881,0.587549275296012));
#9148=CARTESIAN_POINT('Ctrl Pts',(4.09037357512216,5.3940457687175,0.59629853955402));
#9149=CARTESIAN_POINT('Ctrl Pts',(3.9391333930669,5.50231924842836,0.605047803812028));
#9150=CARTESIAN_POINT('Ctrl Pts',(3.78788546298275,5.61059827498556,0.613797516294519));
#9151=CARTESIAN_POINT('Ctrl Pts',(3.63217055501693,5.71263742444897,0.62254722877701));
#9152=CARTESIAN_POINT('Ctrl Pts',(3.47251758582549,5.80809010055222,0.6312969412595));
#9153=CARTESIAN_POINT('Ctrl Pts',(3.35029497128432,5.8811640665259,0.63799529921369));
#9154=CARTESIAN_POINT('Ctrl Pts',(3.22576502399092,5.95037874273607,0.64469365716788));
#9155=CARTESIAN_POINT('Ctrl Pts',(3.09917575053259,6.01559628526639,0.651392015122069));
#9156=CARTESIAN_POINT('Origin',(0.,0.,-3.69717978381041));
#9157=CARTESIAN_POINT('',(3.09917575053259,6.01559628526639,3.04575158274221));
#9158=CARTESIAN_POINT('',(3.09917575053259,6.01559628526639,2.65160425626863));
#9159=CARTESIAN_POINT('',(3.09917575053259,6.01559628526639,-3.69717978381041));
#9160=CARTESIAN_POINT('',(-6.767,1.71693117622523E-12,1.69717978381002));
#9161=CARTESIAN_POINT('Ctrl Pts',(-6.767,1.71693091881772E-12,1.69717978381002));
#9162=CARTESIAN_POINT('Ctrl Pts',(-6.76700000000005,-0.186007249414028,
1.70592929561597));
#9163=CARTESIAN_POINT('Ctrl Pts',(-6.75932637295447,-0.372014355525948,
1.71467880742193));
#9164=CARTESIAN_POINT('Ctrl Pts',(-6.7440051826694,-0.557389537153533,1.72342831922788));
#9165=CARTESIAN_POINT('Ctrl Pts',(-6.72868405709661,-0.742763935809962,
1.73217779407843));
#9166=CARTESIAN_POINT('Ctrl Pts',(-6.7057154565301,-0.927506129693684,1.74092726892897));
#9167=CARTESIAN_POINT('Ctrl Pts',(-6.67517739415671,-1.11098863924849,1.74967674377952));
#9168=CARTESIAN_POINT('Ctrl Pts',(-6.64463945823092,-1.29447038906543,1.7584261824015));
#9169=CARTESIAN_POINT('Ctrl Pts',(-6.60653217027148,-1.47669218228261,1.76717562102349));
#9170=CARTESIAN_POINT('Ctrl Pts',(-6.560984961167,-1.65703510504169,1.77592505964547));
#9171=CARTESIAN_POINT('Ctrl Pts',(-6.51543793687501,-1.83737729604078,1.78467446276571));
#9172=CARTESIAN_POINT('Ctrl Pts',(-6.46245112202619,-2.0158403539712,1.79342386588594));
#9173=CARTESIAN_POINT('Ctrl Pts',(-6.40220448416217,-2.19181813638219,1.80217326900618));
#9174=CARTESIAN_POINT('Ctrl Pts',(-6.34195808575155,-2.36779521936031,1.81092263735146));
#9175=CARTESIAN_POINT('Ctrl Pts',(-6.27445201489195,-2.54128677544927,1.81967200569673));
#9176=CARTESIAN_POINT('Ctrl Pts',(-6.19991555136135,-2.71170355237951,1.82842137404201));
#9177=CARTESIAN_POINT('Ctrl Pts',(-6.12537937788984,-2.88211966613188,1.83717070833907));
#9178=CARTESIAN_POINT('Ctrl Pts',(-6.04381298133556,-3.04946076210566,1.84592004263613));
#9179=CARTESIAN_POINT('Ctrl Pts',(-5.95549339426238,-3.21315848206981,1.85466937693319));
#9180=CARTESIAN_POINT('Ctrl Pts',(-5.86717414355079,-3.37685557859778,1.86341867790876));
#9181=CARTESIAN_POINT('Ctrl Pts',(-5.77210188986143,-3.53690907467468,1.87216797888434));
#9182=CARTESIAN_POINT('Ctrl Pts',(-5.67059953466957,-3.69277536785075,1.88091727985991));
#9183=CARTESIAN_POINT('Ctrl Pts',(-5.56909755761648,-3.84864108035964,1.88966654824067));
#9184=CARTESIAN_POINT('Ctrl Pts',(-5.46116568337945,-4.0003193810445,1.89841581662144));
#9185=CARTESIAN_POINT('Ctrl Pts',(-5.34717048685982,-4.14729511663389,1.9071650850022));
#9186=CARTESIAN_POINT('Ctrl Pts',(-5.23317570555385,-4.29427031688201,1.91591432151482));
#9187=CARTESIAN_POINT('Ctrl Pts',(-5.11311782178674,-4.4365427598728,1.92466355802743));
#9188=CARTESIAN_POINT('Ctrl Pts',(-4.98740459171885,-4.57362924147791,1.93341279454005));
#9189=CARTESIAN_POINT('Ctrl Pts',(-4.86169180910691,-4.7107152351458,1.94216199991117));
#9190=CARTESIAN_POINT('Ctrl Pts',(-4.73032391415281,-4.8426150931667,1.95091120528229));
#9191=CARTESIAN_POINT('Ctrl Pts',(-4.59374707237132,-4.96888084331672,1.95966041065341));
#9192=CARTESIAN_POINT('Ctrl Pts',(-4.45717070537233,-5.09514615452872,1.96840958560964));
#9193=CARTESIAN_POINT('Ctrl Pts',(-4.31538563819332,-5.21577720253779,1.97715876056588));
#9194=CARTESIAN_POINT('Ctrl Pts',(-4.16887341290463,-5.33036429028795,1.98590793552211));
#9195=CARTESIAN_POINT('Ctrl Pts',(-4.02236168477139,-5.44495098921324,1.99465708079003));
#9196=CARTESIAN_POINT('Ctrl Pts',(-3.87112305634225,-5.55349359238908,2.00340622605795));
#9197=CARTESIAN_POINT('Ctrl Pts',(-3.71567117316504,-5.65562346102623,2.01215537132588));
#9198=CARTESIAN_POINT('Ctrl Pts',(-3.56021980457083,-5.75775299158903,2.02090448763203));
#9199=CARTESIAN_POINT('Ctrl Pts',(-3.40055544862183,-5.85346967275472,2.02965360393819));
#9200=CARTESIAN_POINT('Ctrl Pts',(-3.23722036323211,-5.94244842803666,2.03840272024434));
#9201=CARTESIAN_POINT('Ctrl Pts',(-3.07388580495863,-6.03142689616568,2.04715180831528));
#9202=CARTESIAN_POINT('Ctrl Pts',(-2.90688079257533,-6.11366734484905,2.05590089638622));
#9203=CARTESIAN_POINT('Ctrl Pts',(-2.73677251094451,-6.18889046787375,2.06464998445716));
#9204=CARTESIAN_POINT('Ctrl Pts',(-2.56666476416466,-6.26411335438344,2.0733990450194));
#9205=CARTESIAN_POINT('Ctrl Pts',(-2.39345402971899,-6.33231884350364,2.08214810558163));
#9206=CARTESIAN_POINT('Ctrl Pts',(-2.21772856473829,-6.39327529621116,2.09089716614387));
#9207=CARTESIAN_POINT('Ctrl Pts',(-2.04200363768054,-6.4542315623215,2.09964619992387));
#9208=CARTESIAN_POINT('Ctrl Pts',(-1.86376426619872,-6.50793874252119,2.10839523370387));
#9209=CARTESIAN_POINT('Ctrl Pts',(-1.6836157819446,-6.55421443796181,2.11714426748388));
#9210=CARTESIAN_POINT('Ctrl Pts',(-1.50346783419614,-6.60048999558738,2.12589327520812));
#9211=CARTESIAN_POINT('Ctrl Pts',(-1.32141106256967,-6.63933404145552,2.13464228293236));
#9212=CARTESIAN_POINT('Ctrl Pts',(-1.13806375958738,-6.67061465527082,2.1433912906566));
#9213=CARTESIAN_POINT('Ctrl Pts',(-0.954716987416449,-6.70189517852518,
2.15214027305146));
#9214=CARTESIAN_POINT('Ctrl Pts',(-0.770079973807536,-6.72561226535854,
2.16088925544633));
#9215=CARTESIAN_POINT('Ctrl Pts',(-0.584779770550486,-6.74168536939799,
2.1696382378412));
#9216=CARTESIAN_POINT('Ctrl Pts',(-0.391490647551969,-6.75845143942405,
2.17876441851725));
#9217=CARTESIAN_POINT('Ctrl Pts',(-0.19748021310242,-6.76689975924032,2.1878905991933));
#9218=CARTESIAN_POINT('Ctrl Pts',(-0.00346532629591402,-6.76699911271708,
2.19701677986935));
#9219=CARTESIAN_POINT('Ctrl Pts',(0.184486595297895,-6.76709536139768,2.20585776739928));
#9220=CARTESIAN_POINT('Ctrl Pts',(0.372442378187021,-6.7593565972676,2.2146987549292));
#9221=CARTESIAN_POINT('Ctrl Pts',(0.559750217723831,-6.74380965729002,2.22353974245913));
#9222=CARTESIAN_POINT('Ctrl Pts',(0.745129914459458,-6.72842275717234,2.23228972105689));
#9223=CARTESIAN_POINT('Ctrl Pts',(0.929874656315847,-6.7053877227345,2.24103969965466));
#9224=CARTESIAN_POINT('Ctrl Pts',(1.11335688289939,-6.67478280180715,2.24978967825243));
#9225=CARTESIAN_POINT('Ctrl Pts',(1.29683723119015,-6.64417819417992,2.25853956727737));
#9226=CARTESIAN_POINT('Ctrl Pts',(1.4790548073039,-6.6060039023004,2.26728945630231));
#9227=CARTESIAN_POINT('Ctrl Pts',(1.65939064804959,-6.56038959797096,2.27603934532725));
#9228=CARTESIAN_POINT('Ctrl Pts',(1.83972470264408,-6.51477574543215,2.28478914768819));
#9229=CARTESIAN_POINT('Ctrl Pts',(2.01817678125982,-6.46172209820058,2.29353895004914));
#9230=CARTESIAN_POINT('Ctrl Pts',(2.19414072347805,-6.40140886723971,2.30228875241008));
#9231=CARTESIAN_POINT('Ctrl Pts',(2.37010298132218,-6.34109621361329,2.31103847101557));
#9232=CARTESIAN_POINT('Ctrl Pts',(2.5435768792703,-6.27352420825923,2.31978818962105));
#9233=CARTESIAN_POINT('Ctrl Pts',(2.71397317790084,-6.19892237325447,2.32853790822654));
#9234=CARTESIAN_POINT('Ctrl Pts',(2.88436790207312,-6.12432122756911,2.33728754598481));
#9235=CARTESIAN_POINT('Ctrl Pts',(3.05168482126366,-6.04269049717362,2.34603718374307));
#9236=CARTESIAN_POINT('Ctrl Pts',(3.21535561997496,-5.95430745234871,2.35478682150134));
#9237=CARTESIAN_POINT('Ctrl Pts',(3.3790249607538,-5.86592519481459,2.36353638132035));
#9238=CARTESIAN_POINT('Ctrl Pts',(3.53904799384966,-5.77079087940176,2.37228594113936));
#9239=CARTESIAN_POINT('Ctrl Pts',(3.69488118815067,-5.66922763746971,2.38103550095836));
#9240=CARTESIAN_POINT('Ctrl Pts',(3.85071304610917,-5.56766526648994,2.3897849857458));
#9241=CARTESIAN_POINT('Ctrl Pts',(4.00235489706053,-5.45967423580651,2.39853447053324));
#9242=CARTESIAN_POINT('Ctrl Pts',(4.1492916860774,-5.34562133936262,2.40728395532068));
#9243=CARTESIAN_POINT('Ctrl Pts',(4.29622726385845,-5.23156938308459,2.41603336798399));
#9244=CARTESIAN_POINT('Ctrl Pts',(4.43845763092155,-5.11145583677126,2.42478278064729));
#9245=CARTESIAN_POINT('Ctrl Pts',(4.57549970661051,-4.9856886620413,2.43353219331059));
#9246=CARTESIAN_POINT('Ctrl Pts',(4.71254069815378,-4.85992248226081,2.44228153675691));
#9247=CARTESIAN_POINT('Ctrl Pts',(4.8443932693139,-4.72850295733924,2.45103088020324));
#9248=CARTESIAN_POINT('Ctrl Pts',(4.97060959434769,-4.59187644221605,2.45978022364957));
#9249=CARTESIAN_POINT('Ctrl Pts',(5.09682496280587,-4.45525096256581,2.46852950078586));
#9250=CARTESIAN_POINT('Ctrl Pts',(5.21740397615913,-4.31341878218237,2.47727877792216));
#9251=CARTESIAN_POINT('Ctrl Pts',(5.33193710452009,-4.16686161438582,2.48602805505845));
#9252=CARTESIAN_POINT('Ctrl Pts',(5.44646940289459,-4.02030550864411,2.49477726879142));
#9253=CARTESIAN_POINT('Ctrl Pts',(5.55495572749741,-3.86902470980024,2.50352648252438));
#9254=CARTESIAN_POINT('Ctrl Pts',(5.65702762491532,-3.71353301465665,2.51227569625735));
#9255=CARTESIAN_POINT('Ctrl Pts',(5.75909881655227,-3.55804239466774,2.52102484949346));
#9256=CARTESIAN_POINT('Ctrl Pts',(5.85475551250852,-3.39834117619432,2.52977400272958));
#9257=CARTESIAN_POINT('Ctrl Pts',(5.94367283728161,-3.23497174691847,2.53852315596569));
#9258=CARTESIAN_POINT('Ctrl Pts',(6.03258957676374,-3.07160339300843,2.54727225161123));
#9259=CARTESIAN_POINT('Ctrl Pts',(6.11476689685343,-2.9045671282938,2.55602134725676));
#9260=CARTESIAN_POINT('Ctrl Pts',(6.18992570525316,-2.7344302447578,2.56477044290229));
#9261=CARTESIAN_POINT('Ctrl Pts',(6.2650840438876,-2.56429442462879,2.57351948386333));
#9262=CARTESIAN_POINT('Ctrl Pts',(6.33322384283383,-2.39105828655815,2.58226852482437));
#9263=CARTESIAN_POINT('Ctrl Pts',(6.39411368720104,-2.21531017131876,2.59101756578541));
#9264=CARTESIAN_POINT('Ctrl Pts',(6.45500317120952,-2.03956309619317,2.59976655496781));
#9265=CARTESIAN_POINT('Ctrl Pts',(6.50864269270127,-1.86130434438443,2.60851554415021));
#9266=CARTESIAN_POINT('Ctrl Pts',(6.5548500844638,-1.68113930719762,2.61726453333261));
#9267=CARTESIAN_POINT('Ctrl Pts',(6.60199664749445,-1.49731239211659,2.62619134686198));
#9268=CARTESIAN_POINT('Ctrl Pts',(6.64140563640942,-1.31150116499492,2.63511816039135));
#9269=CARTESIAN_POINT('Ctrl Pts',(6.67293772282202,-1.12436255155483,2.64404497392071));
#9270=CARTESIAN_POINT('Ctrl Pts',(6.70384494949896,-0.940932395049558,2.65279488807624));
#9271=CARTESIAN_POINT('Ctrl Pts',(6.72718449348951,-0.756227260504914,2.66154480223177));
#9272=CARTESIAN_POINT('Ctrl Pts',(6.74287707373947,-0.57087456453988,2.67029471638729));
#9273=CARTESIAN_POINT('Ctrl Pts',(6.7585693453868,-0.385525513630672,2.67904445847127));
#9274=CARTESIAN_POINT('Ctrl Pts',(6.76661493004108,-0.199529212416435,2.68779420055525));
#9275=CARTESIAN_POINT('Ctrl Pts',(6.76698649908907,-0.0135174385986461,
2.69654394263923));
#9276=CARTESIAN_POINT('Ctrl Pts',(6.76735806132385,0.172490924447578,2.70529352428513));
#9277=CARTESIAN_POINT('Ctrl Pts',(6.7600558889628,0.358514472903222,2.71404310593102));
#9278=CARTESIAN_POINT('Ctrl Pts',(6.7451047845457,0.543921359664041,2.72279268757692));
#9279=CARTESIAN_POINT('Ctrl Pts',(6.73015393440668,0.729325093152314,2.73154212041597));
#9280=CARTESIAN_POINT('Ctrl Pts',(6.70755443556871,0.914111900258259,2.74029155325501));
#9281=CARTESIAN_POINT('Ctrl Pts',(6.67738304682287,1.09765415591732,2.74904098609406));
#9282=CARTESIAN_POINT('Ctrl Pts',(6.64721213111822,1.2811935339147,2.75779028175539));
#9283=CARTESIAN_POINT('Ctrl Pts',(6.6094696095545,1.46348811672852,2.76653957741671));
#9284=CARTESIAN_POINT('Ctrl Pts',(6.56428366991132,1.64391876348423,2.77528887307804));
#9285=CARTESIAN_POINT('Ctrl Pts',(6.51909837867661,1.82434682109917,2.78403804318887));
#9286=CARTESIAN_POINT('Ctrl Pts',(6.46646995271859,2.00291071820645,2.79278721329969));
#9287=CARTESIAN_POINT('Ctrl Pts',(6.40657713281481,2.17900400212903,2.80153638341052));
#9288=CARTESIAN_POINT('Ctrl Pts',(6.34668509278988,2.3550949930985,2.81028543959629));
#9289=CARTESIAN_POINT('Ctrl Pts',(6.27952894037451,2.52871516398307,2.81903449578206));
#9290=CARTESIAN_POINT('Ctrl Pts',(6.2053367506137,2.69927486771596,2.82778355196784));
#9291=CARTESIAN_POINT('Ctrl Pts',(6.12832117907839,2.87632521636088,2.8368655532501));
#9292=CARTESIAN_POINT('Ctrl Pts',(6.04372366626002,3.05007728920149,2.84594755453237));
#9293=CARTESIAN_POINT('Ctrl Pts',(5.95185378007792,3.21989527478336,2.85502955581463));
#9294=CARTESIAN_POINT('Ctrl Pts',(5.8633445081729,3.38350129286893,2.86377933612176));
#9295=CARTESIAN_POINT('Ctrl Pts',(5.76808562057168,3.54345567125104,2.87252911642888));
#9296=CARTESIAN_POINT('Ctrl Pts',(5.66640068804391,3.69921508465452,2.881278896736));
#9297=CARTESIAN_POINT('Ctrl Pts',(5.56471941107827,3.85496889852422,2.89002836248949));
#9298=CARTESIAN_POINT('Ctrl Pts',(5.45661270815014,4.00652780919772,2.89877782824297));
#9299=CARTESIAN_POINT('Ctrl Pts',(5.34244776449012,4.1533770456936,2.90752729399645));
#9300=CARTESIAN_POINT('Ctrl Pts',(5.22828631819485,4.30022178356384,2.91627649171605));
#9301=CARTESIAN_POINT('Ctrl Pts',(5.1080671784395,4.44235690972816,2.92502568943565));
#9302=CARTESIAN_POINT('Ctrl Pts',(4.98219864544591,4.57929969070785,2.93377488715526));
#9303=CARTESIAN_POINT('Ctrl Pts',(4.85633329943897,4.71623900430132,2.94252386334549));
#9304=CARTESIAN_POINT('Ctrl Pts',(4.72481904033522,4.84798602483739,2.95127283953573));
#9305=CARTESIAN_POINT('Ctrl Pts',(4.58810250737074,4.9740933225924,2.96002181572596));
#9306=CARTESIAN_POINT('Ctrl Pts',(4.45137708685513,5.10020881822248,2.96877136066214));
#9307=CARTESIAN_POINT('Ctrl Pts',(4.30944892635918,5.22068366308043,2.97752090559831));
#9308=CARTESIAN_POINT('Ctrl Pts',(4.16280009466523,5.33510865604958,2.98627045053449));
#9309=CARTESIAN_POINT('Ctrl Pts',(4.01615988348655,5.4495269227299,2.99501948114276));
#9310=CARTESIAN_POINT('Ctrl Pts',(3.86479978232101,5.55789587288716,3.00376851175104));
#9311=CARTESIAN_POINT('Ctrl Pts',(3.70923383580943,5.65984746713959,3.01251754235931));
#9312=CARTESIAN_POINT('Ctrl Pts',(3.5536657779941,5.76180044505463,3.02126669170734));
#9313=CARTESIAN_POINT('Ctrl Pts',(3.39389200026703,5.85733573571139,3.03001584105536));
#9314=CARTESIAN_POINT('Ctrl Pts',(3.23045513625898,5.94612887622006,3.03876499040338));
#9315=CARTESIAN_POINT('Ctrl Pts',(3.18695122151483,5.96976399206739,3.04109385451632));
#9316=CARTESIAN_POINT('Ctrl Pts',(3.14318791262616,5.99292165435357,3.04342271862927));
#9317=CARTESIAN_POINT('Ctrl Pts',(3.09917575053259,6.01559628526639,3.04575158274221));
#9318=CARTESIAN_POINT('Ctrl Pts',(3.0991757505326,6.01559628526639,1.04590194808422));
#9319=CARTESIAN_POINT('Ctrl Pts',(2.93899076682749,6.0981220056699,1.05436020197771));
#9320=CARTESIAN_POINT('Ctrl Pts',(2.77543011409295,6.17428487827924,1.0628184558712));
#9321=CARTESIAN_POINT('Ctrl Pts',(2.60904700143327,6.24380995421162,1.07127670976468));
#9322=CARTESIAN_POINT('Ctrl Pts',(2.44807637543265,6.31107336103624,1.07945981442202));
#9323=CARTESIAN_POINT('Ctrl Pts',(2.28446439899782,6.37212391638201,1.08764291907935));
#9324=CARTESIAN_POINT('Ctrl Pts',(2.11873390604186,6.42676089763643,1.09582602373668));
#9325=CARTESIAN_POINT('Ctrl Pts',(1.95300550772517,6.48139718834342,1.10400902496916));
#9326=CARTESIAN_POINT('Ctrl Pts',(1.7851589879776,6.52961995329728,1.11219202620163));
#9327=CARTESIAN_POINT('Ctrl Pts',(1.61573361158904,6.57127795001714,1.12037502743411));
#9328=CARTESIAN_POINT('Ctrl Pts',(1.44627930262977,6.61294306062373,1.12855942606801));
#9329=CARTESIAN_POINT('Ctrl Pts',(1.27524594961246,6.64804108434614,1.13674382470191));
#9330=CARTESIAN_POINT('Ctrl Pts',(1.10318434504944,6.67647162061203,1.1449282233358));
#9331=CARTESIAN_POINT('Ctrl Pts',(0.931061800160809,6.70491222633033,1.15311552069844));
#9332=CARTESIAN_POINT('Ctrl Pts',(0.757910633300328,6.72668058281044,1.16130281806107));
#9333=CARTESIAN_POINT('Ctrl Pts',(0.584288150258786,6.74172799491845,1.16949011542371));
#9334=CARTESIAN_POINT('Ctrl Pts',(0.410491565226955,6.75679049599623,1.17768562269523));
#9335=CARTESIAN_POINT('Ctrl Pts',(0.23622307891755,6.76511856369256,1.18588112996675));
#9336=CARTESIAN_POINT('Ctrl Pts',(0.0620422149731795,6.76671558169554,1.19407663723826));
#9337=CARTESIAN_POINT('Ctrl Pts',(-0.112242861460377,6.76831355519512,1.20227704788547));
#9338=CARTESIAN_POINT('Ctrl Pts',(-0.286439852232708,6.76317246294877,1.21047745853267));
#9339=CARTESIAN_POINT('Ctrl Pts',(-0.459993091321101,6.75134766960915,1.21867786917987));
#9340=CARTESIAN_POINT('Ctrl Pts',(-0.633758091792142,6.73950844822082,1.22688828557693));
#9341=CARTESIAN_POINT('Ctrl Pts',(-0.806877415747976,6.72096928098195,1.23509870197399));
#9342=CARTESIAN_POINT('Ctrl Pts',(-0.978803580777068,6.69583695666628,1.24330911837105));
#9343=CARTESIAN_POINT('Ctrl Pts',(-1.01782823477954,6.69013229699141,1.24517275942334));
#9344=CARTESIAN_POINT('Ctrl Pts',(-1.05679146850773,6.68408814897662,1.24703640047563));
#9345=CARTESIAN_POINT('Ctrl Pts',(-1.09568698135607,6.67770612103339,1.24890004152792));
#9346=CARTESIAN_POINT('Ctrl Pts',(-1.27638429160621,6.64805706388433,1.25755797918603));
#9347=CARTESIAN_POINT('Ctrl Pts',(-1.4560377233974,6.61104300179464,1.26621591684414));
#9348=CARTESIAN_POINT('Ctrl Pts',(-1.63403926172985,6.56674993365252,1.27487385450225));
#9349=CARTESIAN_POINT('Ctrl Pts',(-1.8118097449023,6.52251436019299,1.28352055371158));
#9350=CARTESIAN_POINT('Ctrl Pts',(-1.98793231762334,6.4710186949504,1.29216725292091));
#9351=CARTESIAN_POINT('Ctrl Pts',(-2.16180789265776,6.41240014622003,1.30081395213024));
#9352=CARTESIAN_POINT('Ctrl Pts',(-2.34145041084909,6.35183739205194,1.309747437007));
#9353=CARTESIAN_POINT('Ctrl Pts',(-2.51869400074864,6.2836711745779,1.31868092188375));
#9354=CARTESIAN_POINT('Ctrl Pts',(-2.69289047092689,6.20811001123459,1.32761440676051));
#9355=CARTESIAN_POINT('Ctrl Pts',(-2.86101743343772,6.13518161685499,1.33623662324646));
#9356=CARTESIAN_POINT('Ctrl Pts',(-3.0263057022571,6.05536500245165,1.34485883973241));
#9357=CARTESIAN_POINT('Ctrl Pts',(-3.18818833214442,5.96889806905581,1.35348105621836));
#9358=CARTESIAN_POINT('Ctrl Pts',(-3.34991343823498,5.88251527439463,1.36209488264864));
#9359=CARTESIAN_POINT('Ctrl Pts',(-3.50823924606549,5.78949520530867,1.37070870907892));
#9360=CARTESIAN_POINT('Ctrl Pts',(-3.66262035967817,5.69012311825245,1.37932253550919));
#9361=CARTESIAN_POINT('Ctrl Pts',(-3.81682114161615,5.59086710714916,1.38792630017926));
#9362=CARTESIAN_POINT('Ctrl Pts',(-3.96708616736431,5.4852740441412,1.39653006484934));
#9363=CARTESIAN_POINT('Ctrl Pts',(-4.11289597547628,5.37367431976585,1.40513382951941));
#9364=CARTESIAN_POINT('Ctrl Pts',(-4.12917626282904,5.36121373426173,1.40609447656337));
#9365=CARTESIAN_POINT('Ctrl Pts',(-4.14540103557206,5.34867831175663,1.40705512360734));
#9366=CARTESIAN_POINT('Ctrl Pts',(-4.16156959154005,5.33606854667078,1.40801577065131));
#9367=CARTESIAN_POINT('Ctrl Pts',(-4.30619743622049,5.22327411098318,1.41660876508709));
#9368=CARTESIAN_POINT('Ctrl Pts',(-4.44615136592851,5.10466300999673,1.42520175952288));
#9369=CARTESIAN_POINT('Ctrl Pts',(-4.58098069078672,4.98065306065773,1.43379475395866));
#9370=CARTESIAN_POINT('Ctrl Pts',(-4.71593654636555,4.85652673405237,1.44239581249904));
#9371=CARTESIAN_POINT('Ctrl Pts',(-4.84575797284515,4.72699165302455,1.45099687103942));
#9372=CARTESIAN_POINT('Ctrl Pts',(-4.97003164824036,4.59250197773384,1.4595979295798));
#9373=CARTESIAN_POINT('Ctrl Pts',(-5.09950788202557,4.45238206429071,1.46855906042938));
#9374=CARTESIAN_POINT('Ctrl Pts',(-5.22296162407326,4.3068840874192,1.47752019127895));
#9375=CARTESIAN_POINT('Ctrl Pts',(-5.33997329198447,4.15655797997485,1.48648132212853));
#9376=CARTESIAN_POINT('Ctrl Pts',(-5.45259162315717,4.01187603795759,1.49510599708373));
#9377=CARTESIAN_POINT('Ctrl Pts',(-5.55924268538611,3.86272218531277,1.50373067203892));
#9378=CARTESIAN_POINT('Ctrl Pts',(-5.659597629749,3.70961502980289,1.51235534699412));
#9379=CARTESIAN_POINT('Ctrl Pts',(-5.76004892269622,3.55636087946602,1.52098830231086));
#9380=CARTESIAN_POINT('Ctrl Pts',(-5.85419187260608,3.39914611040372,1.5296212576276));
#9381=CARTESIAN_POINT('Ctrl Pts',(-5.94174325319159,3.23851449173108,1.53825421294434));
#9382=CARTESIAN_POINT('Ctrl Pts',(-6.02942535205559,3.07764304258949,1.54690005766443));
#9383=CARTESIAN_POINT('Ctrl Pts',(-6.11049607590235,2.91334482106544,1.55554590238451));
#9384=CARTESIAN_POINT('Ctrl Pts',(-6.18471940918936,2.74618550531395,1.56419174710459));
#9385=CARTESIAN_POINT('Ctrl Pts',(-6.1931318604605,2.72723971648984,1.5651716646613));
#9386=CARTESIAN_POINT('Ctrl Pts',(-6.2014564030209,2.70825719217792,1.56615158221801));
#9387=CARTESIAN_POINT('Ctrl Pts',(-6.209692733347,2.68923876913477,1.56713149977472));
#9388=CARTESIAN_POINT('Ctrl Pts',(-6.2847318510522,2.51596673792696,1.57605928022646));
#9389=CARTESIAN_POINT('Ctrl Pts',(-6.35258133209611,2.33939829260565,1.58498706067819));
#9390=CARTESIAN_POINT('Ctrl Pts',(-6.41296689791982,2.16012605330908,1.59391484112993));
#9391=CARTESIAN_POINT('Ctrl Pts',(-6.47316786112979,1.98140186094215,1.60281532877446));
#9392=CARTESIAN_POINT('Ctrl Pts',(-6.52595035309913,1.7999906094939,1.61171581641899));
#9393=CARTESIAN_POINT('Ctrl Pts',(-6.57108874529099,1.61650292344622,1.62061630406351));
#9394=CARTESIAN_POINT('Ctrl Pts',(-6.61614205175235,1.43336111112258,1.6295000143162));
#9395=CARTESIAN_POINT('Ctrl Pts',(-6.65357993410146,1.24815091814942,1.63838372456888));
#9396=CARTESIAN_POINT('Ctrl Pts',(-6.68322586262152,1.06149944379957,1.64726743482156));
#9397=CARTESIAN_POINT('Ctrl Pts',(-6.71278037808465,0.875423508240538,1.65612375220271));
#9398=CARTESIAN_POINT('Ctrl Pts',(-6.73459082912758,0.687915409948818,1.66498006958387));
#9399=CARTESIAN_POINT('Ctrl Pts',(-6.74853140626713,0.499612708631656,1.67383638696503));
#9400=CARTESIAN_POINT('Ctrl Pts',(-6.76077955300093,0.334170554191592,1.68161751924669));
#9401=CARTESIAN_POINT('Ctrl Pts',(-6.76695336728736,0.168115363848341,1.68939865152836));
#9402=CARTESIAN_POINT('Ctrl Pts',(-6.76699973671697,0.00188766322821155,
1.69717978381002));
#9403=CARTESIAN_POINT('',(-6.7669988871634,0.00388086708922883,1.30263766580882));
#9404=CARTESIAN_POINT('Ctrl Pts',(3.09917575053259,6.01559628526639,0.651392015122069));
#9405=CARTESIAN_POINT('Ctrl Pts',(2.93382385406851,6.10078394805573,0.660141462533071));
#9406=CARTESIAN_POINT('Ctrl Pts',(2.76495774058454,6.17915009368906,0.668890909944073));
#9407=CARTESIAN_POINT('Ctrl Pts',(2.59315096270441,6.25042855207747,0.677640357355075));
#9408=CARTESIAN_POINT('Ctrl Pts',(2.42134557177907,6.32170643505203,0.686389734133892));
#9409=CARTESIAN_POINT('Ctrl Pts',(2.2465998286745,6.38589663545787,0.695139110912711));
#9410=CARTESIAN_POINT('Ctrl Pts',(2.06950724656412,6.44278113522558,0.703888487691529));
#9411=CARTESIAN_POINT('Ctrl Pts',(1.89241603525059,6.49966519467506,0.712637796745217));
#9412=CARTESIAN_POINT('Ctrl Pts',(1.71297829413072,6.54924357900826,0.721387105798904));
#9413=CARTESIAN_POINT('Ctrl Pts',(1.53180346303543,6.59134790089498,0.730136414852592));
#9414=CARTESIAN_POINT('Ctrl Pts',(1.35062997415456,6.63345191085632,0.738885659087957));
#9415=CARTESIAN_POINT('Ctrl Pts',(1.16771970017938,6.6680819043066,0.747634903323322));
#9416=CARTESIAN_POINT('Ctrl Pts',(0.983693865807499,6.69512026616197,0.756384147558687));
#9417=CARTESIAN_POINT('Ctrl Pts',(0.79966933364614,6.72215843668747,0.765133329882321));
#9418=CARTESIAN_POINT('Ctrl Pts',(0.614529540397793,6.74160504146313,0.773882512205955));
#9419=CARTESIAN_POINT('Ctrl Pts',(0.428903274066081,6.75339403422423,0.782631694529589));
#9420=CARTESIAN_POINT('Ctrl Pts',(0.243278259616313,6.76518294747919,0.79138081784787));
#9421=CARTESIAN_POINT('Ctrl Pts',(0.0571670646193069,6.76931433390325,0.80012994116615));
#9422=CARTESIAN_POINT('Ctrl Pts',(-0.128798232278501,6.76577416230855,0.808879064484431));
#9423=CARTESIAN_POINT('Ctrl Pts',(-0.314762336770819,6.76223401341335,0.817628131703521));
#9424=CARTESIAN_POINT('Ctrl Pts',(-0.500580258550281,6.75102241038819,0.826377198922611));
#9425=CARTESIAN_POINT('Ctrl Pts',(-0.685620923081958,6.73217743006171,0.835126266141701));
#9426=CARTESIAN_POINT('Ctrl Pts',(-0.870660462589858,6.71333256431032,0.843875280167572));
#9427=CARTESIAN_POINT('Ctrl Pts',(-1.05492246925224,6.68685444316035,0.852624294193443));
#9428=CARTESIAN_POINT('Ctrl Pts',(-1.23778116033235,6.65283299047303,0.861373308219314));
#9429=CARTESIAN_POINT('Ctrl Pts',(-1.42991953208325,6.6170850230927,0.870566315669095));
#9430=CARTESIAN_POINT('Ctrl Pts',(-1.62050811672427,6.57300825457429,0.879759323118877));
#9431=CARTESIAN_POINT('Ctrl Pts',(-1.808832359327,6.52076793758615,0.888952330568658));
#9432=CARTESIAN_POINT('Ctrl Pts',(-1.98808125918661,6.47104508077799,0.897702327111858));
#9433=CARTESIAN_POINT('Ctrl Pts',(-2.16527861796168,6.41392703709576,0.906452323655057));
#9434=CARTESIAN_POINT('Ctrl Pts',(-2.33982251053777,6.34960783192007,0.915202320198256));
#9435=CARTESIAN_POINT('Ctrl Pts',(-2.51436286473782,6.28528993063151,0.92395213936041));
#9436=CARTESIAN_POINT('Ctrl Pts',(-2.68624959139652,6.21377125909801,0.932701958522564));
#9437=CARTESIAN_POINT('Ctrl Pts',(-2.85489882883657,6.13529475062996,0.941451777684718));
#9438=CARTESIAN_POINT('Ctrl Pts',(-3.02354487157988,6.05681972873043,0.950201431100385));
#9439=CARTESIAN_POINT('Ctrl Pts',(-3.18895328794629,5.97138725457424,0.958951084516051));
#9440=CARTESIAN_POINT('Ctrl Pts',(-3.35056224292841,5.87928751263812,0.967700737931717));
#9441=CARTESIAN_POINT('Ctrl Pts',(-3.5121683513698,5.7871893929244,0.976450237233122));
#9442=CARTESIAN_POINT('Ctrl Pts',(-3.66997488333246,5.68842438234431,0.985199736534526));
#9443=CARTESIAN_POINT('Ctrl Pts',(-3.82344584363613,5.58332793956987,0.99394923583593));
#9444=CARTESIAN_POINT('Ctrl Pts',(-3.97691430468979,5.47823320827418,1.00269859265314));
#9445=CARTESIAN_POINT('Ctrl Pts',(-4.12604709891178,5.36680741303859,1.01144794947035));
#9446=CARTESIAN_POINT('Ctrl Pts',(-4.27033770824381,5.24942900300129,1.02019730628756));
#9447=CARTESIAN_POINT('Ctrl Pts',(-4.41462615955329,5.1320523484854,1.02894653224865));
#9448=CARTESIAN_POINT('Ctrl Pts',(-4.55407234859234,5.008723438162,1.03769575820974));
#9449=CARTESIAN_POINT('Ctrl Pts',(-4.68820267126408,4.87986113666694,1.04644498417083));
#9450=CARTESIAN_POINT('Ctrl Pts',(-4.82233116607775,4.75100059124012,1.05519409090203));
#9451=CARTESIAN_POINT('Ctrl Pts',(-4.95114373285208,4.61660700405917,1.06394319763323));
#9452=CARTESIAN_POINT('Ctrl Pts',(-5.07420289460218,4.47713680653282,1.07269230436443));
#9453=CARTESIAN_POINT('Ctrl Pts',(-5.19726054284679,4.33766832435139,1.08144130349031));
#9454=CARTESIAN_POINT('Ctrl Pts',(-5.31456473809728,4.19312357162134,1.09019030261618));
#9455=CARTESIAN_POINT('Ctrl Pts',(-5.42571709822437,4.04399344337201,1.09893930174206));
#9456=CARTESIAN_POINT('Ctrl Pts',(-5.53688157678416,3.89484705614786,1.10768925473124));
#9457=CARTESIAN_POINT('Ctrl Pts',(-5.64189270668245,3.74111452275908,1.11643920772042));
#9458=CARTESIAN_POINT('Ctrl Pts',(-5.7403937771409,3.5833180550102,1.12518916070959));
#9459=CARTESIAN_POINT('Ctrl Pts',(-5.83889104761745,3.42552767474563,1.13393877614241));
#9460=CARTESIAN_POINT('Ctrl Pts',(-5.93087860943509,3.2636739170053,1.14268839157523));
#9461=CARTESIAN_POINT('Ctrl Pts',(-6.01604401546832,3.09830653808622,1.15143800700804));
#9462=CARTESIAN_POINT('Ctrl Pts',(-6.10120658874526,2.93294465958691,1.16018733141274));
#9463=CARTESIAN_POINT('Ctrl Pts',(-6.17954732910422,2.76406964856331,1.16893665581743));
#9464=CARTESIAN_POINT('Ctrl Pts',(-6.25080016021907,2.59225507174839,1.17768598022213));
#9465=CARTESIAN_POINT('Ctrl Pts',(-6.32205100003899,2.4204452966163,1.18643506011043));
#9466=CARTESIAN_POINT('Ctrl Pts',(-6.38621421723416,2.24569638477739,1.19518413999873));
#9467=CARTESIAN_POINT('Ctrl Pts',(-6.44307190015638,2.06860181992941,1.20393321988703));
#9468=CARTESIAN_POINT('Ctrl Pts',(-6.49993470395433,1.89149130509521,1.21268308775944));
#9469=CARTESIAN_POINT('Ctrl Pts',(-6.54949056911377,1.71203498737916,1.22143295563185));
#9470=CARTESIAN_POINT('Ctrl Pts',(-6.5915711633095,1.53084244748656,1.23018282350427));
#9471=CARTESIAN_POINT('Ctrl Pts',(-6.63364884164169,1.34966246285206,1.23893208507771));
#9472=CARTESIAN_POINT('Ctrl Pts',(-6.66825222068406,1.16674677594928,1.24768134665116));
#9473=CARTESIAN_POINT('Ctrl Pts',(-6.69526377527894,0.982716632319621,1.25643060822461));
#9474=CARTESIAN_POINT('Ctrl Pts',(-6.72227670080852,0.798677148490385,1.26518031385493));
#9475=CARTESIAN_POINT('Ctrl Pts',(-6.74169698918657,0.613523378321138,1.27393001948524));
#9476=CARTESIAN_POINT('Ctrl Pts',(-6.75345867564419,0.427884232434633,1.28267972511556));
#9477=CARTESIAN_POINT('Ctrl Pts',(-6.76240141614664,0.286737576745467,1.28933237201331));
#9478=CARTESIAN_POINT('Ctrl Pts',(-6.76691777740362,0.145310511934777,1.29598501891107));
#9479=CARTESIAN_POINT('Ctrl Pts',(-6.7669988871634,0.00388086708923183,
1.30263766580882));
#9480=CARTESIAN_POINT('Ctrl Pts',(-6.76699888234511,0.00388925958011982,
1.30282022489417));
#9481=CARTESIAN_POINT('Ctrl Pts',(-6.76709704828634,-0.166911583330251,
1.31088823850834));
#9482=CARTESIAN_POINT('Ctrl Pts',(-6.76072447256501,-0.337975125809719,
1.31895625212251));
#9483=CARTESIAN_POINT('Ctrl Pts',(-6.74784790637245,-0.508760879456122,
1.32702426573667));
#9484=CARTESIAN_POINT('Ctrl Pts',(-6.73498437417603,-0.679373759308398,
1.33508411269704));
#9485=CARTESIAN_POINT('Ctrl Pts',(-6.71562998115061,-0.849709041106061,
1.3431439596574));
#9486=CARTESIAN_POINT('Ctrl Pts',(-6.68980346698226,-1.01922449595371,1.35120380661777));
#9487=CARTESIAN_POINT('Ctrl Pts',(-6.66399744413831,-1.18860545351101,1.35925725871828));
#9488=CARTESIAN_POINT('Ctrl Pts',(-6.631729577102,-1.3571675119843,1.36731071081879));
#9489=CARTESIAN_POINT('Ctrl Pts',(-6.59307054474703,-1.52437193361366,1.3753641629193));
#9490=CARTESIAN_POINT('Ctrl Pts',(-6.55443373493223,-1.69148024039619,1.38341298561882));
#9491=CARTESIAN_POINT('Ctrl Pts',(-6.50941315756628,-1.8572321015694,1.39146180831834));
#9492=CARTESIAN_POINT('Ctrl Pts',(-6.45813084501019,-2.02109747135758,1.39951063101786));
#9493=CARTESIAN_POINT('Ctrl Pts',(-6.40685982948131,-2.18492674309461,1.40755768063491));
#9494=CARTESIAN_POINT('Ctrl Pts',(-6.34932992906808,-2.34686999290344,1.41560473025197));
#9495=CARTESIAN_POINT('Ctrl Pts',(-6.28571348724989,-2.50641077164235,1.42365177986902));
#9496=CARTESIAN_POINT('Ctrl Pts',(-6.22210246312151,-2.66593796360361,1.43169814418496));
#9497=CARTESIAN_POINT('Ctrl Pts',(-6.15240606641361,-2.82306274460335,1.4397445085009));
#9498=CARTESIAN_POINT('Ctrl Pts',(-6.07684530578212,-2.97728737773058,1.44779087281684));
#9499=CARTESIAN_POINT('Ctrl Pts',(-6.00127603156627,-3.13152938766044,1.45583814373299));
#9500=CARTESIAN_POINT('Ctrl Pts',(-5.91984124224131,-3.28287026394481,1.46388541464914));
#9501=CARTESIAN_POINT('Ctrl Pts',(-5.83280847428983,-3.43083580228679,1.47193268556529));
#9502=CARTESIAN_POINT('Ctrl Pts',(-5.74574867847249,-3.57884729105428,1.47998245554661));
#9503=CARTESIAN_POINT('Ctrl Pts',(-5.65308763304491,-3.72348103402496,1.48803222552792));
#9504=CARTESIAN_POINT('Ctrl Pts',(-5.55513677578713,-3.86429093137375,1.49608199550924));
#9505=CARTESIAN_POINT('Ctrl Pts',(-5.45707735362938,-4.0052568969066,1.50414068754083));
#9506=CARTESIAN_POINT('Ctrl Pts',(-5.35371662344936,-4.14239024572985,1.51219937957242));
#9507=CARTESIAN_POINT('Ctrl Pts',(-5.24540748325654,-4.27527652141897,1.52025807160401));
#9508=CARTESIAN_POINT('Ctrl Pts',(-5.13703552073096,-4.40823987486733,1.52832143790253));
#9509=CARTESIAN_POINT('Ctrl Pts',(-5.02370967782438,-4.53695096962361,1.53638480420105));
#9510=CARTESIAN_POINT('Ctrl Pts',(-4.90582009191361,-4.66103188422658,1.54444817049957));
#9511=CARTESIAN_POINT('Ctrl Pts',(-4.78774817794154,-4.78530470240126,1.55252400760231));
#9512=CARTESIAN_POINT('Ctrl Pts',(-4.66509868858995,-4.90493277636546,1.56059984470504));
#9513=CARTESIAN_POINT('Ctrl Pts',(-4.53829604923321,-5.01957746922131,1.56867568180778));
#9514=CARTESIAN_POINT('Ctrl Pts',(-4.43183989767127,-5.11582651309254,1.57545568688464));
#9515=CARTESIAN_POINT('Ctrl Pts',(-4.32245714146461,-5.20856377686059,1.5822356919615));
#9516=CARTESIAN_POINT('Ctrl Pts',(-4.21041417240527,-5.29761281114512,1.58901569703837));
#9517=CARTESIAN_POINT('Ctrl Pts',(-4.07461375508114,-5.40554368909021,1.59723332574482));
#9518=CARTESIAN_POINT('Ctrl Pts',(-3.93445583250538,-5.50841221031713,1.60545095445126));
#9519=CARTESIAN_POINT('Ctrl Pts',(-3.79035361516694,-5.6058459193944,1.61366858315771));
#9520=CARTESIAN_POINT('Ctrl Pts',(-3.64642540015359,-5.70316197801332,1.62187628914036));
#9521=CARTESIAN_POINT('Ctrl Pts',(-3.49856266833718,-5.7950560916103,1.63008399512301));
#9522=CARTESIAN_POINT('Ctrl Pts',(-3.34721244403314,-5.88119527430519,1.63829170110566));
#9523=CARTESIAN_POINT('Ctrl Pts',(-3.19601434056076,-5.96724787923536,1.64649115759237));
#9524=CARTESIAN_POINT('Ctrl Pts',(-3.04133603523146,-6.04755689511507,1.65469061407908));
#9525=CARTESIAN_POINT('Ctrl Pts',(-2.88365440396457,-6.12183193811262,1.66289007056579));
#9526=CARTESIAN_POINT('Ctrl Pts',(-2.72609935444989,-6.19604735548979,1.67108294479203));
#9527=CARTESIAN_POINT('Ctrl Pts',(-2.56554610473802,-6.26423829474248,1.67927581901827));
#9528=CARTESIAN_POINT('Ctrl Pts',(-2.40249712904587,-6.32615969960657,1.68746869324451));
#9529=CARTESIAN_POINT('Ctrl Pts',(-2.2395460639878,-6.3880439207718,1.69565664766363));
#9530=CARTESIAN_POINT('Ctrl Pts',(-2.07410259367583,-6.44366597973139,1.70384460208275));
#9531=CARTESIAN_POINT('Ctrl Pts',(-1.9066902882976,-6.49282843947933,1.71203255650188));
#9532=CARTESIAN_POINT('Ctrl Pts',(-1.73932881463813,-6.54197597193551,1.72021802479673));
#9533=CARTESIAN_POINT('Ctrl Pts',(-1.57000004024041,-6.58466770686101,1.72840349309158));
#9534=CARTESIAN_POINT('Ctrl Pts',(-1.39924407841513,-6.62075562220961,1.73658896138643));
#9535=CARTESIAN_POINT('Ctrl Pts',(-1.2285124106804,-6.65683840319527,1.74477326510403));
#9536=CARTESIAN_POINT('Ctrl Pts',(-1.0563543116645,-6.6863191605116,1.75295756882163));
#9537=CARTESIAN_POINT('Ctrl Pts',(-0.883321511936119,-6.70910069283141,
1.76114187253924));
#9538=CARTESIAN_POINT('Ctrl Pts',(-0.71028162461133,-6.73188315830555,1.7693265114941));
#9539=CARTESIAN_POINT('Ctrl Pts',(-0.536367321981056,-6.74796580506379,
1.77751115044896));
#9540=CARTESIAN_POINT('Ctrl Pts',(-0.362136944529296,-6.75730314795829,
1.78569578940383));
#9541=CARTESIAN_POINT('Ctrl Pts',(-0.187867505324042,-6.7666425842477,1.79388226332199));
#9542=CARTESIAN_POINT('Ctrl Pts',(-0.0132822094303347,-6.76923368560635,
1.80206873724016));
#9543=CARTESIAN_POINT('Ctrl Pts',(0.161059064643997,-6.76508307249039,1.81025521115833));
#9544=CARTESIAN_POINT('Ctrl Pts',(0.335565213747655,-6.76092853412802,1.81844942704772));
#9545=CARTESIAN_POINT('Ctrl Pts',(0.509826519751691,-6.75001955194915,1.82664364293712));
#9546=CARTESIAN_POINT('Ctrl Pts',(0.683285754315221,-6.73241484000725,1.83483785882651));
#9547=CARTESIAN_POINT('Ctrl Pts',(0.856828512439003,-6.71480165109829,1.84303602036968));
#9548=CARTESIAN_POINT('Ctrl Pts',(1.02956807303185,-6.69048635478854,1.85123418191286));
#9549=CARTESIAN_POINT('Ctrl Pts',(1.20095600065172,-6.65957909214228,1.85943234345603));
#9550=CARTESIAN_POINT('Ctrl Pts',(1.37258163648686,-6.62862896235629,1.86764187552207));
#9551=CARTESIAN_POINT('Ctrl Pts',(1.54285154136209,-6.59106867194669,1.8758514075881));
#9552=CARTESIAN_POINT('Ctrl Pts',(1.71122987766881,-6.54705898138803,1.88406093965413));
#9553=CARTESIAN_POINT('Ctrl Pts',(1.86681880238214,-6.50639210831407,1.89164690525144));
#9554=CARTESIAN_POINT('Ctrl Pts',(2.02079255608343,-6.46021898958428,1.89923287084874));
#9555=CARTESIAN_POINT('Ctrl Pts',(2.17274339940872,-6.40870307631161,1.90681883644604));
#9556=CARTESIAN_POINT('Ctrl Pts',(2.34617658434546,-6.34990400209602,1.9154772824643));
#9557=CARTESIAN_POINT('Ctrl Pts',(2.51737466941937,-6.28400871360894,1.92413572848256));
#9558=CARTESIAN_POINT('Ctrl Pts',(2.68575184058637,-6.21120165916282,1.93279417450082));
#9559=CARTESIAN_POINT('Ctrl Pts',(2.85391124251773,-6.13848876912442,1.94144142218881));
#9560=CARTESIAN_POINT('Ctrl Pts',(3.01925672896684,-6.05888205885241,1.95008866987681));
#9561=CARTESIAN_POINT('Ctrl Pts',(3.18121968350465,-5.97261503240269,1.95873591756481));
#9562=CARTESIAN_POINT('Ctrl Pts',(3.34820464494508,-5.88367311277425,1.96765129161356));
#9563=CARTESIAN_POINT('Ctrl Pts',(3.51159362552328,-5.7876512745346,1.97656666566232));
#9564=CARTESIAN_POINT('Ctrl Pts',(3.67078501067243,-5.68485940067322,1.98548203971107));
#9565=CARTESIAN_POINT('Ctrl Pts',(3.8247536597855,-5.58543991297035,1.99410491900406));
#9566=CARTESIAN_POINT('Ctrl Pts',(3.97479546597253,-5.47968771741926,2.00272779829704));
#9567=CARTESIAN_POINT('Ctrl Pts',(4.12038995361317,-5.36793029296801,2.01135067759003));
#9568=CARTESIAN_POINT('Ctrl Pts',(4.27339245822644,-5.25048652069846,2.02041229901667));
#9569=CARTESIAN_POINT('Ctrl Pts',(4.42148297714327,-5.12641061677613,2.02947392044331));
#9570=CARTESIAN_POINT('Ctrl Pts',(4.56409038230586,-4.99613530462728,2.03853554186995));
#9571=CARTESIAN_POINT('Ctrl Pts',(4.69949920388821,-4.87243607260469,2.04713974778483));
#9572=CARTESIAN_POINT('Ctrl Pts',(4.82996451064429,-4.74314806876094,2.05574395369972));
#9573=CARTESIAN_POINT('Ctrl Pts',(4.95502957298067,-4.60868429498995,2.0643481596146));
#9574=CARTESIAN_POINT('Ctrl Pts',(4.96167826317439,-4.60153595190051,2.06480557512635));
#9575=CARTESIAN_POINT('Ctrl Pts',(4.96831169919643,-4.59437299049623,2.06526299063811));
#9576=CARTESIAN_POINT('Ctrl Pts',(4.9749298151216,-4.58719547595415,2.06572040614986));
#9577=CARTESIAN_POINT('Ctrl Pts',(5.09926231861951,-4.45235372310475,2.07431373034638));
#9578=CARTESIAN_POINT('Ctrl Pts',(5.21803628917243,-4.31253349391377,2.08290705454289));
#9579=CARTESIAN_POINT('Ctrl Pts',(5.33087497953295,-4.16822035796928,2.09150037873941));
#9580=CARTESIAN_POINT('Ctrl Pts',(5.44381910882233,-4.02377237268877,2.10010173272514));
#9581=CARTESIAN_POINT('Ctrl Pts',(5.55081669959559,-3.87482334158127,2.10870308671086));
#9582=CARTESIAN_POINT('Ctrl Pts',(5.65153378452362,-3.72188861767627,2.11730444069659));
#9583=CARTESIAN_POINT('Ctrl Pts',(5.75625285279107,-3.56287704774733,2.12624756862635));
#9584=CARTESIAN_POINT('Ctrl Pts',(5.85418190555349,-3.39955689125769,2.13519069655611));
#9585=CARTESIAN_POINT('Ctrl Pts',(5.94499829711266,-3.2325352662156,2.14413382448587));
#9586=CARTESIAN_POINT('Ctrl Pts',(6.03258260228007,-3.0714578139397,2.15275867328578));
#9587=CARTESIAN_POINT('Ctrl Pts',(6.11355169969962,-2.90693810381944,2.16138352208569));
#9588=CARTESIAN_POINT('Ctrl Pts',(6.18766535016368,-2.73954129634576,2.1700083708856));
#9589=CARTESIAN_POINT('Ctrl Pts',(6.26184988137288,-2.57198439406669,2.1786414683105));
#9590=CARTESIAN_POINT('Ctrl Pts',(6.32916576362738,-2.40154518468651,2.18727456573541));
#9591=CARTESIAN_POINT('Ctrl Pts',(6.38942186041684,-2.2288062476643,2.19590766316031));
#9592=CARTESIAN_POINT('Ctrl Pts',(6.44976743376656,-2.05581080405222,2.20455358019855));
#9593=CARTESIAN_POINT('Ctrl Pts',(6.50303217958239,-1.88050909936569,2.21319949723679));
#9594=CARTESIAN_POINT('Ctrl Pts',(6.54907510496199,-1.70349765763476,2.22184541427503));
#9595=CARTESIAN_POINT('Ctrl Pts',(6.55400386756034,-1.68454909243631,2.22277093480126));
#9596=CARTESIAN_POINT('Ctrl Pts',(6.55884992321818,-1.66558094336064,2.22369645532748));
#9597=CARTESIAN_POINT('Ctrl Pts',(6.5636131339237,-1.64659394757308,2.22462197585371));
#9598=CARTESIAN_POINT('Ctrl Pts',(6.60594263129275,-1.47786112470964,2.23284685211935));
#9599=CARTESIAN_POINT('Ctrl Pts',(6.64181725648561,-1.30727253348678,2.24107172838499));
#9600=CARTESIAN_POINT('Ctrl Pts',(6.6710748893297,-1.13536285871732,2.24929660465063));
#9601=CARTESIAN_POINT('Ctrl Pts',(6.7003017416724,-0.963634041572632,2.25751282793273));
#9602=CARTESIAN_POINT('Ctrl Pts',(6.72292540467277,-0.790587258972482,2.26572905121483));
#9603=CARTESIAN_POINT('Ctrl Pts',(6.7388339249604,-0.616770890852404,2.27394527449693));
#9604=CARTESIAN_POINT('Ctrl Pts',(6.7547288948653,-0.443102574107876,2.28215449945561));
#9605=CARTESIAN_POINT('Ctrl Pts',(6.76392008114605,-0.268666332271811,2.2903637244143));
#9606=CARTESIAN_POINT('Ctrl Pts',(6.76634682560446,-0.0940193364815904,
2.29857294937299));
#9607=CARTESIAN_POINT('Ctrl Pts',(6.76877198893167,0.0805138690767463,2.30677682565902));
#9608=CARTESIAN_POINT('Ctrl Pts',(6.76444148450205,0.255257197980979,2.31498070194504));
#9609=CARTESIAN_POINT('Ctrl Pts',(6.75334658911855,0.429649679670336,2.32318457823107));
#9610=CARTESIAN_POINT('Ctrl Pts',(6.74225670153002,0.603963447522276,2.33138475161329));
#9611=CARTESIAN_POINT('Ctrl Pts',(6.72440852847687,0.777926326716095,2.33958492499551));
#9612=CARTESIAN_POINT('Ctrl Pts',(6.69984542688093,0.950978578046184,2.34778509837773));
#9613=CARTESIAN_POINT('Ctrl Pts',(6.6752843512477,1.12401655604,2.35598459541029));
#9614=CARTESIAN_POINT('Ctrl Pts',(6.64400949203572,1.29614369999235,2.36418409244284));
#9615=CARTESIAN_POINT('Ctrl Pts',(6.60611598786299,1.46680624313542,2.3723835894754));
#9616=CARTESIAN_POINT('Ctrl Pts',(6.56822277133648,1.63746749079427,2.3805830242663));
#9617=CARTESIAN_POINT('Ctrl Pts',(6.52371108658861,1.8066638095827,2.3887824590572));
#9618=CARTESIAN_POINT('Ctrl Pts',(6.47272701235145,1.9738525840538,2.3969818938481));
#9619=CARTESIAN_POINT('Ctrl Pts',(6.42173407708048,2.14107041593953,2.40518275370104));
#9620=CARTESIAN_POINT('Ctrl Pts',(6.36426661572915,2.30627966545076,2.41338361355399));
#9621=CARTESIAN_POINT('Ctrl Pts',(6.30052032183935,2.46895376102699,2.42158447340693));
#9622=CARTESIAN_POINT('Ctrl Pts',(6.23675138571998,2.63168563728338,2.42978824614688));
#9623=CARTESIAN_POINT('Ctrl Pts',(6.16669930513151,2.79188023225607,2.43799201888684));
#9624=CARTESIAN_POINT('Ctrl Pts',(6.09060758166292,2.94903175401524,2.44619579162679));
#9625=CARTESIAN_POINT('Ctrl Pts',(6.01442912047239,3.10636241437681,2.45440891592992));
#9626=CARTESIAN_POINT('Ctrl Pts',(5.93219741848239,3.26064274842366,2.46262204023304));
#9627=CARTESIAN_POINT('Ctrl Pts',(5.84420205173538,3.41139141385037,2.47083516453617));
#9628=CARTESIAN_POINT('Ctrl Pts',(5.75615469141516,3.56222915171421,2.4790531417048));
#9629=CARTESIAN_POINT('Ctrl Pts',(5.66233707004052,3.70953075941405,2.48727111887342));
#9630=CARTESIAN_POINT('Ctrl Pts',(5.56308156368259,3.85284473030188,2.49548909604205));
#9631=CARTESIAN_POINT('Ctrl Pts',(5.46367237026505,3.9963806083019,2.50371979791275));
#9632=CARTESIAN_POINT('Ctrl Pts',(5.35880868062565,4.13591622413822,2.51195049978345));
#9633=CARTESIAN_POINT('Ctrl Pts',(5.24886338443184,4.27103291623593,2.52018120165414));
#9634=CARTESIAN_POINT('Ctrl Pts',(5.14981902958912,4.39275295393276,2.52759583952322));
#9635=CARTESIAN_POINT('Ctrl Pts',(5.04665142495269,4.51088722119783,2.5350104773923));
#9636=CARTESIAN_POINT('Ctrl Pts',(4.93965759606199,4.62515641180567,2.54242511526138));
#9637=CARTESIAN_POINT('Ctrl Pts',(4.82192603404906,4.75089347944494,2.55058387457617));
#9638=CARTESIAN_POINT('Ctrl Pts',(4.69919892592138,4.87233694864273,2.55874263389096));
#9639=CARTESIAN_POINT('Ctrl Pts',(4.57182321124844,4.9890601845528,2.56690139320575));
#9640=CARTESIAN_POINT('Ctrl Pts',(4.44464415896944,5.10560320501866,2.57504755576187));
#9641=CARTESIAN_POINT('Ctrl Pts',(4.31283106579809,5.21744026702449,2.58319371831799));
#9642=CARTESIAN_POINT('Ctrl Pts',(4.17677003524039,5.32417891066012,2.59133988087411));
#9643=CARTESIAN_POINT('Ctrl Pts',(4.04083006405777,5.4308225843147,2.59947879543758));
#9644=CARTESIAN_POINT('Ctrl Pts',(3.900649961062,5.53237664176759,2.60761771000106));
#9645=CARTESIAN_POINT('Ctrl Pts',(3.75665199545179,5.62848601180354,2.61575662456454));
#9646=CARTESIAN_POINT('Ctrl Pts',(3.61277866478679,5.72451219603879,2.62388849463147));
#9647=CARTESIAN_POINT('Ctrl Pts',(3.46509435600694,5.81510287755278,2.63202036469841));
#9648=CARTESIAN_POINT('Ctrl Pts',(3.31405342985844,5.89994397126308,2.64015223476534));
#9649=CARTESIAN_POINT('Ctrl Pts',(3.24315034852982,5.93977089182523,2.64396957526644));
#9650=CARTESIAN_POINT('Ctrl Pts',(3.17150803856598,5.97833140537366,2.64778691576753));
#9651=CARTESIAN_POINT('Ctrl Pts',(3.09917575053259,6.01559628526639,2.65160425626863));
#9652=CARTESIAN_POINT('Origin',(0.,0.,-3.69717978381041));
#9653=CARTESIAN_POINT('',(3.09917575053259,6.01559628526639,5.04568623149126));
#9654=CARTESIAN_POINT('',(3.09917575053259,6.01559628526639,4.6512641878525));
#9655=CARTESIAN_POINT('',(3.09917575053259,6.01559628526639,-3.69717978381041));
#9656=CARTESIAN_POINT('',(-6.767,1.74262947821857E-12,3.69717978381002));
#9657=CARTESIAN_POINT('Ctrl Pts',(-6.76699874815404,-0.00411612459687825,
3.69717978381002));
#9658=CARTESIAN_POINT('Ctrl Pts',(-6.76687514509871,-0.207322247497207,
3.70672388776635));
#9659=CARTESIAN_POINT('Ctrl Pts',(-6.75759441333246,-0.410217053170746,
3.71626799172269));
#9660=CARTESIAN_POINT('Ctrl Pts',(-6.73926461418622,-0.612046942625711,
3.72581209567903));
#9661=CARTESIAN_POINT('Ctrl Pts',(-6.72085546075771,-0.814750604122016,
3.73539751844705));
#9662=CARTESIAN_POINT('Ctrl Pts',(-6.69331880047275,-1.01638001069333,3.74498294121508));
#9663=CARTESIAN_POINT('Ctrl Pts',(-6.65681420104171,-1.21618818149556,3.75456836398311));
#9664=CARTESIAN_POINT('Ctrl Pts',(-6.62013581135308,-1.41694759444292,3.76419942081144));
#9665=CARTESIAN_POINT('Ctrl Pts',(-6.57440394949044,-1.61586829355856,3.77383047763978));
#9666=CARTESIAN_POINT('Ctrl Pts',(-6.51982988362059,-1.81221060824836,3.78346153446811));
#9667=CARTESIAN_POINT('Ctrl Pts',(-6.49850475257701,-1.88893250029406,3.78722492547955));
#9668=CARTESIAN_POINT('Ctrl Pts',(-6.47583003097947,-1.9652609000595,3.79098831649099));
#9669=CARTESIAN_POINT('Ctrl Pts',(-6.45182033297249,-2.04115246638823,3.79475170750244));
#9670=CARTESIAN_POINT('Ctrl Pts',(-6.39934861310573,-2.20700882191145,3.80297636733964));
#9671=CARTESIAN_POINT('Ctrl Pts',(-6.34040815136586,-2.37105913358796,3.81120102717685));
#9672=CARTESIAN_POINT('Ctrl Pts',(-6.27514141282242,-2.53276316482239,3.81942568701406));
#9673=CARTESIAN_POINT('Ctrl Pts',(-6.20994328005258,-2.69429721927526,3.82764170141925));
#9674=CARTESIAN_POINT('Ctrl Pts',(-6.13843224588407,-2.85348957496219,3.83585771582444));
#9675=CARTESIAN_POINT('Ctrl Pts',(-6.06080066937938,-3.00981465310582,3.84407373022964));
#9676=CARTESIAN_POINT('Ctrl Pts',(-5.98323514607949,-3.16600672129568,3.85228275399897));
#9677=CARTESIAN_POINT('Ctrl Pts',(-5.89955961069964,-3.31933605155709,3.86049177776831));
#9678=CARTESIAN_POINT('Ctrl Pts',(-5.81001470431116,-3.46929649002331,3.86870080153765));
#9679=CARTESIAN_POINT('Ctrl Pts',(-5.72052805641934,-3.61915936325602,3.8769044844629));
#9680=CARTESIAN_POINT('Ctrl Pts',(-5.6251798270287,-3.76565740397587,3.88510816738816));
#9681=CARTESIAN_POINT('Ctrl Pts',(-5.52425686518469,-3.90830846882124,3.89331185031341));
#9682=CARTESIAN_POINT('Ctrl Pts',(-5.42337935892376,-4.05089528379511,3.90151183830954));
#9683=CARTESIAN_POINT('Ctrl Pts',(-5.3169323290966,-4.18963828286598,3.90971182630567));
#9684=CARTESIAN_POINT('Ctrl Pts',(-5.2052463170163,-4.32408369243569,3.9179118143018));
#9685=CARTESIAN_POINT('Ctrl Pts',(-5.09356924072396,-4.45851834528081,3.9261111462323));
#9686=CARTESIAN_POINT('Ctrl Pts',(-4.97665423921318,-4.58865581243468,3.9343104781628));
#9687=CARTESIAN_POINT('Ctrl Pts',(-4.85487280636697,-4.7140745681415,3.94250981009329));
#9688=CARTESIAN_POINT('Ctrl Pts',(-4.73309217086887,-4.83949250268532,3.95070908833973));
#9689=CARTESIAN_POINT('Ctrl Pts',(-4.60644541647417,-4.96019152935117,3.95890836658617));
#9690=CARTESIAN_POINT('Ctrl Pts',(-4.47534155471156,-5.07578633993512,3.96710764483261));
#9691=CARTESIAN_POINT('Ctrl Pts',(-4.34421476743135,-5.1914013640416,3.97530835684839));
#9692=CARTESIAN_POINT('Ctrl Pts',(-4.20862958889401,-5.30191015669955,3.98350906886417));
#9693=CARTESIAN_POINT('Ctrl Pts',(-4.06902885310209,-5.40696709742372,3.99170978087996));
#9694=CARTESIAN_POINT('Ctrl Pts',(-3.92937838036582,-5.51206146783037,3.99991341464507));
#9695=CARTESIAN_POINT('Ctrl Pts',(-3.78570978670595,-5.61169990152915,4.00811704841019));
#9696=CARTESIAN_POINT('Ctrl Pts',(-3.63849570577419,-5.7055795497971,4.01632068217531));
#9697=CARTESIAN_POINT('Ctrl Pts',(-3.49111298434392,-5.79956674151865,4.0245337135801));
#9698=CARTESIAN_POINT('Ctrl Pts',(-3.3401769639609,-5.88778177515888,4.0327467449849));
#9699=CARTESIAN_POINT('Ctrl Pts',(-3.18618668325835,-5.96996678545427,4.04095977638969));
#9700=CARTESIAN_POINT('Ctrl Pts',(-3.0321052852362,-6.05220042529832,4.04917766751293));
#9701=CARTESIAN_POINT('Ctrl Pts',(-2.87496634646817,-6.12839677324508,4.05739555863617));
#9702=CARTESIAN_POINT('Ctrl Pts',(-2.71528969016249,-6.19834581953099,4.0656134497594));
#9703=CARTESIAN_POINT('Ctrl Pts',(-2.55536399152904,-6.26840396299939,4.07384415805193));
#9704=CARTESIAN_POINT('Ctrl Pts',(-2.39289299910971,-6.33219520177195,4.08207486634445));
#9705=CARTESIAN_POINT('Ctrl Pts',(-2.22841381171218,-6.38955873936302,4.09030557463697));
#9706=CARTESIAN_POINT('Ctrl Pts',(-2.07735383705311,-6.44224221057887,4.0978647716744));
#9707=CARTESIAN_POINT('Ctrl Pts',(-1.92460035350539,-6.48950454530975,4.10542396871184));
#9708=CARTESIAN_POINT('Ctrl Pts',(-1.77057662546198,-6.53125925173452,4.11298316574927));
#9709=CARTESIAN_POINT('Ctrl Pts',(-1.60443543898398,-6.57629891253597,4.12113706502553));
#9710=CARTESIAN_POINT('Ctrl Pts',(-1.43630241505965,-6.61506879967032,4.12929096430179));
#9711=CARTESIAN_POINT('Ctrl Pts',(-1.26669608406012,-6.647388211217,4.13744486357804));
#9712=CARTESIAN_POINT('Ctrl Pts',(-1.09729671869426,-6.67966818433323,4.14558881289005));
#9713=CARTESIAN_POINT('Ctrl Pts',(-0.926427980106585,-6.705513282256,4.15373276220206));
#9714=CARTESIAN_POINT('Ctrl Pts',(-0.754624309461781,-6.72479227571896,
4.16187671151406));
#9715=CARTESIAN_POINT('Ctrl Pts',(-0.58299412470652,-6.74405180141782,4.17001243713512));
#9716=CARTESIAN_POINT('Ctrl Pts',(-0.410431248022078,-6.75675838200398,
4.17814816275618));
#9717=CARTESIAN_POINT('Ctrl Pts',(-0.237481088370139,-6.7628316356883,4.18628388837724));
#9718=CARTESIAN_POINT('Ctrl Pts',(-0.0646691923669045,-6.76890003415761,
4.19441310995626));
#9719=CARTESIAN_POINT('Ctrl Pts',(0.108529006420706,-6.76834565170371,4.20254233153528));
#9720=CARTESIAN_POINT('Ctrl Pts',(0.281562188883845,-6.76113982504363,4.2106715531143));
#9721=CARTESIAN_POINT('Ctrl Pts',(0.454493423549635,-6.75393824391694,4.21879598511352));
#9722=CARTESIAN_POINT('Ctrl Pts',(0.627259471093833,-6.74009303809521,4.22692041711275));
#9723=CARTESIAN_POINT('Ctrl Pts',(0.799308222788764,-6.71962762100567,4.23504484911198));
#9724=CARTESIAN_POINT('Ctrl Pts',(0.972401168918694,-6.69903799566454,4.24321858973215));
#9725=CARTESIAN_POINT('Ctrl Pts',(1.14476770881433,-6.67174752452259,4.25139233035232));
#9726=CARTESIAN_POINT('Ctrl Pts',(1.31584942939305,-6.63783317650918,4.25956607097249));
#9727=CARTESIAN_POINT('Ctrl Pts',(1.48583584150506,-6.60413595673365,4.26768748123687));
#9728=CARTESIAN_POINT('Ctrl Pts',(1.65455347901243,-6.56389952228322,4.27580889150126));
#9729=CARTESIAN_POINT('Ctrl Pts',(1.82146379873784,-6.51725084908411,4.28393030176565));
#9730=CARTESIAN_POINT('Ctrl Pts',(1.98838702354686,-6.47059856912761,4.29205233995692));
#9731=CARTESIAN_POINT('Ctrl Pts',(2.15350229973429,-6.41753316134611,4.3001743781482));
#9732=CARTESIAN_POINT('Ctrl Pts',(2.31628549880373,-6.35823171078497,4.30829641633948));
#9733=CARTESIAN_POINT('Ctrl Pts',(2.47911228141139,-6.29891438286639,4.3164206291235));
#9734=CARTESIAN_POINT('Ctrl Pts',(2.63960539989487,-6.23335781284451,4.32454484190751));
#9735=CARTESIAN_POINT('Ctrl Pts',(2.79726002877108,-6.16178751105875,4.33266905469152));
#9736=CARTESIAN_POINT('Ctrl Pts',(2.95662075258456,-6.08944269519494,4.3408811854669));
#9737=CARTESIAN_POINT('Ctrl Pts',(3.11308084356436,-6.0109533872662,4.34909331624228));
#9738=CARTESIAN_POINT('Ctrl Pts',(3.26614451899616,-5.92660011988588,4.35730544701766));
#9739=CARTESIAN_POINT('Ctrl Pts',(3.41781127900701,-5.84301669146101,4.36544263086597));
#9740=CARTESIAN_POINT('Ctrl Pts',(3.5661430787814,-5.75367613426408,4.37357981471428));
#9741=CARTESIAN_POINT('Ctrl Pts',(3.71068719452792,-5.6588947281573,4.3817169985626));
#9742=CARTESIAN_POINT('Ctrl Pts',(3.85722827952742,-5.56280385640558,4.38996660280151));
#9743=CARTESIAN_POINT('Ctrl Pts',(3.99987593618909,-5.46112092530692,4.39821620704042));
#9744=CARTESIAN_POINT('Ctrl Pts',(4.13819382896349,-5.35421710747038,4.40646581127933));
#9745=CARTESIAN_POINT('Ctrl Pts',(4.27651172173791,-5.24731328963384,4.41471541551824));
#9746=CARTESIAN_POINT('Ctrl Pts',(4.41049959614208,-5.13518888050348,4.42296501975715));
#9747=CARTESIAN_POINT('Ctrl Pts',(4.5397608289452,-5.01825274532629,4.43121462399606));
#9748=CARTESIAN_POINT('Ctrl Pts',(4.6686344797541,-4.90166723608299,4.43943949229526));
#9749=CARTESIAN_POINT('Ctrl Pts',(4.79319512442212,-4.77995045954151,4.44766436059445));
#9750=CARTESIAN_POINT('Ctrl Pts',(4.91300921252629,-4.65345350010418,4.45588922889364));
#9751=CARTESIAN_POINT('Ctrl Pts',(5.03268831700465,-4.5270990532754,4.46410483098248));
#9752=CARTESIAN_POINT('Ctrl Pts',(5.14763126871457,-4.3959754053497,4.47232043307131));
#9753=CARTESIAN_POINT('Ctrl Pts',(5.25743829939608,-4.26047315776585,4.48053603516014));
#9754=CARTESIAN_POINT('Ctrl Pts',(5.36714368291744,-4.12509634312172,4.48874403215651));
#9755=CARTESIAN_POINT('Ctrl Pts',(5.47172238916977,-3.98534927787293,4.49695202915288));
#9756=CARTESIAN_POINT('Ctrl Pts',(5.57081212771845,-3.84165865709917,4.50516002614925));
#9757=CARTESIAN_POINT('Ctrl Pts',(5.66983004266583,-3.69807218815797,4.51336207371117));
#9758=CARTESIAN_POINT('Ctrl Pts',(5.76336671165853,-3.55054815128399,4.5215641212731));
#9759=CARTESIAN_POINT('Ctrl Pts',(5.85110066242351,-3.39954556348157,4.52976616883502));
#9760=CARTESIAN_POINT('Ctrl Pts',(5.93878863840104,-3.24862210481691,4.53796391831861));
#9761=CARTESIAN_POINT('Ctrl Pts',(6.02067977404064,-3.0942240361053,4.54616166780219));
#9762=CARTESIAN_POINT('Ctrl Pts',(6.0964963675306,-2.9368386133198,4.55435941728578));
#9763=CARTESIAN_POINT('Ctrl Pts',(6.17229850081262,-2.77948320805207,4.56255560324406));
#9764=CARTESIAN_POINT('Ctrl Pts',(6.2420282385286,-2.61914190380967,4.57075178920234));
#9765=CARTESIAN_POINT('Ctrl Pts',(6.30545409585691,-2.45632604615946,4.57894797516063));
#9766=CARTESIAN_POINT('Ctrl Pts',(6.36887526122796,-2.29352223288794,4.58714355480225));
#9767=CARTESIAN_POINT('Ctrl Pts',(6.42599334384335,-2.1282445647956,4.59533913444387));
#9768=CARTESIAN_POINT('Ctrl Pts',(6.47662525903511,-1.96102377701762,4.60353471408549));
#9769=CARTESIAN_POINT('Ctrl Pts',(6.52726264058033,-1.79378493564775,4.61173117854324));
#9770=CARTESIAN_POINT('Ctrl Pts',(6.57141235555588,-1.62460290014048,4.61992764300099));
#9771=CARTESIAN_POINT('Ctrl Pts',(6.60894137641023,-1.45402299953366,4.62812410745874));
#9772=CARTESIAN_POINT('Ctrl Pts',(6.64648127698161,-1.28339364756873,4.6363229480833));
#9773=CARTESIAN_POINT('Ctrl Pts',(6.67739658325312,-1.11136597367322,4.64452178870787));
#9774=CARTESIAN_POINT('Ctrl Pts',(6.7016054944437,-0.938494963674312,4.65272062933243));
#9775=CARTESIAN_POINT('Ctrl Pts',(6.72583969259791,-0.765443384507747,4.66092803390203));
#9776=CARTESIAN_POINT('Ctrl Pts',(6.74335345068524,-0.591547065171197,4.66913543847162));
#9777=CARTESIAN_POINT('Ctrl Pts',(6.75411682876472,-0.417366581552912,4.67734284304122));
#9778=CARTESIAN_POINT('Ctrl Pts',(6.764885972297,-0.243092797360377,4.68555464394468));
#9779=CARTESIAN_POINT('Ctrl Pts',(6.76889751925103,-0.0685349038397829,
4.69376644484815));
#9780=CARTESIAN_POINT('Ctrl Pts',(6.7661736998704,0.105747166308009,4.70197824575162));
#9781=CARTESIAN_POINT('Ctrl Pts',(6.76344587064204,0.280285804335476,4.71020213558852));
#9782=CARTESIAN_POINT('Ctrl Pts',(6.75396287890137,0.454547449203377,4.71842602542543));
#9783=CARTESIAN_POINT('Ctrl Pts',(6.73779892515249,0.627976627123945,4.72664991526234));
#9784=CARTESIAN_POINT('Ctrl Pts',(6.7228637304116,0.788221984555494,4.73424863758919));
#9785=CARTESIAN_POINT('Ctrl Pts',(6.70222532253822,0.947756493134326,4.74184735991604));
#9786=CARTESIAN_POINT('Ctrl Pts',(6.67598072542722,1.10615114415903,4.7494460822429));
#9787=CARTESIAN_POINT('Ctrl Pts',(6.64757229195141,1.27760524907543,4.75767131034644));
#9788=CARTESIAN_POINT('Ctrl Pts',(6.61251475319008,1.44820490932618,4.76589653844998));
#9789=CARTESIAN_POINT('Ctrl Pts',(6.57086910197774,1.61739551275323,4.77412176655352));
#9790=CARTESIAN_POINT('Ctrl Pts',(6.52927076183557,1.78639390911235,4.78233765047987));
#9791=CARTESIAN_POINT('Ctrl Pts',(6.48109929797756,1.953986090966,4.79055353440623));
#9792=CARTESIAN_POINT('Ctrl Pts',(6.42646721677411,2.11962452140175,4.79876941833258));
#9793=CARTESIAN_POINT('Ctrl Pts',(6.37188622260497,2.28510806159735,4.80697761949938));
#9794=CARTESIAN_POINT('Ctrl Pts',(6.31085675483196,2.44864115035205,4.81518582066617));
#9795=CARTESIAN_POINT('Ctrl Pts',(6.24354194746007,2.60968828604232,4.82339402183297));
#9796=CARTESIAN_POINT('Ctrl Pts',(6.17627656594569,2.77061717296844,4.83159619613291));
#9797=CARTESIAN_POINT('Ctrl Pts',(6.10273517536377,2.92906341298115,4.83979837043286));
#9798=CARTESIAN_POINT('Ctrl Pts',(6.02313016636458,3.08450838854898,4.8480005447328));
#9799=CARTESIAN_POINT('Ctrl Pts',(5.94318809705292,3.24061154295122,4.85623744834774));
#9800=CARTESIAN_POINT('Ctrl Pts',(5.85713105593703,3.39368761115387,4.86447435196267));
#9801=CARTESIAN_POINT('Ctrl Pts',(5.76522269587831,3.54323246018796,4.87271125557761));
#9802=CARTESIAN_POINT('Ctrl Pts',(5.67377311696107,3.69203082265109,4.88090704284534));
#9803=CARTESIAN_POINT('Ctrl Pts',(5.57653070104813,3.83733283623083,4.88910283011308));
#9804=CARTESIAN_POINT('Ctrl Pts',(5.47380066331511,3.97866752799113,4.89729861738081));
#9805=CARTESIAN_POINT('Ctrl Pts',(5.37107953619944,4.11998996063635,4.90549369376081));
#9806=CARTESIAN_POINT('Ctrl Pts',(5.26287194613215,4.25734546662081,4.91368877014081));
#9807=CARTESIAN_POINT('Ctrl Pts',(5.14952554808702,4.39029334208992,4.92188384652081));
#9808=CARTESIAN_POINT('Ctrl Pts',(5.03616836004626,4.52325387351475,4.93007970303003));
#9809=CARTESIAN_POINT('Ctrl Pts',(4.91767162284475,4.65180566603528,4.93827555953926));
#9810=CARTESIAN_POINT('Ctrl Pts',(4.79442228751602,4.77554226543643,4.94647141604849));
#9811=CARTESIAN_POINT('Ctrl Pts',(4.67008954242387,4.90036655784238,4.95473931733539));
#9812=CARTESIAN_POINT('Ctrl Pts',(4.54092049909171,5.02029032542614,4.96300721862229));
#9813=CARTESIAN_POINT('Ctrl Pts',(4.40734890870411,5.1349356955024,4.97127511990918));
#9814=CARTESIAN_POINT('Ctrl Pts',(4.27479143544765,5.24871064220897,4.97948024871348));
#9815=CARTESIAN_POINT('Ctrl Pts',(4.1378983484203,5.35728687916309,4.98768537751777));
#9816=CARTESIAN_POINT('Ctrl Pts',(3.99712506123443,5.46033700835871,4.99589050632207));
#9817=CARTESIAN_POINT('Ctrl Pts',(3.85473631700978,5.56456969896128,5.00418979385027));
#9818=CARTESIAN_POINT('Ctrl Pts',(3.70837807988881,5.66314845353252,5.01248908137847));
#9819=CARTESIAN_POINT('Ctrl Pts',(3.55854948648691,5.75578096805497,5.02078836890666));
#9820=CARTESIAN_POINT('Ctrl Pts',(3.40872089308502,5.84841348257741,5.02908765643486));
#9821=CARTESIAN_POINT('Ctrl Pts',(3.25542229250714,5.93509961111655,5.03738694396306));
#9822=CARTESIAN_POINT('Ctrl Pts',(3.09917575053259,6.01559628526639,5.04568623149126));
#9823=CARTESIAN_POINT('Ctrl Pts',(3.09917575053259,6.01559628526639,3.04575158274221));
#9824=CARTESIAN_POINT('Ctrl Pts',(2.93382384459267,6.10078395293758,3.05450103065462));
#9825=CARTESIAN_POINT('Ctrl Pts',(2.76495772122989,6.17915010267047,3.06325047856702));
#9826=CARTESIAN_POINT('Ctrl Pts',(2.59315093316718,6.25042856433175,3.07199992647943));
#9827=CARTESIAN_POINT('Ctrl Pts',(2.42134553245621,6.3217064504145,3.08074930373944));
#9828=CARTESIAN_POINT('Ctrl Pts',(2.24659977927592,6.38589665313457,3.08949868099945));
#9829=CARTESIAN_POINT('Ctrl Pts',(2.06950718689917,6.44278115439076,3.09824805825945));
#9830=CARTESIAN_POINT('Ctrl Pts',(1.8924159657286,6.49966521519724,3.10699736777411));
#9831=CARTESIAN_POINT('Ctrl Pts',(1.71297821457198,6.54924360009546,3.11574667728876));
#9832=CARTESIAN_POINT('Ctrl Pts',(1.53180337335845,6.59134792173556,3.12449598680342));
#9833=CARTESIAN_POINT('Ctrl Pts',(1.3506298747778,6.63345193135305,3.13324523147954));
#9834=CARTESIAN_POINT('Ctrl Pts',(1.16771959102946,6.66808192368239,3.14199447615567));
#9835=CARTESIAN_POINT('Ctrl Pts',(0.983693746906757,6.6951202836317,3.15074372083179));
#9836=CARTESIAN_POINT('Ctrl Pts',(0.799669205419815,6.72215845218868,3.15949290357597));
#9837=CARTESIAN_POINT('Ctrl Pts',(0.614529402873452,6.74160505424579,3.16824208632015));
#9838=CARTESIAN_POINT('Ctrl Pts',(0.428903127363257,6.75339404354122,3.17699126906432));
#9839=CARTESIAN_POINT('Ctrl Pts',(0.243278104163808,6.76518295330331,3.18574039278293));
#9840=CARTESIAN_POINT('Ctrl Pts',(0.0571669005389651,6.76931433552276,3.19448951650154));
#9841=CARTESIAN_POINT('Ctrl Pts',(-0.128798404777745,6.76577415902472,3.20323864022016));
#9842=CARTESIAN_POINT('Ctrl Pts',(-0.314762517259277,6.7622340052344,3.21198770781936));
#9843=CARTESIAN_POINT('Ctrl Pts',(-0.500580446819634,6.75102239665088,3.22073677541857));
#9844=CARTESIAN_POINT('Ctrl Pts',(-0.685621118842681,6.73217741012497,3.22948584301777));
#9845=CARTESIAN_POINT('Ctrl Pts',(-0.870660665414701,6.71333253821769,3.23823485740356));
#9846=CARTESIAN_POINT('Ctrl Pts',(-1.05492267885522,6.68685441030607,3.24698387178934));
#9847=CARTESIAN_POINT('Ctrl Pts',(-1.23778137635301,6.65283295028168,3.25573288617513));
#9848=CARTESIAN_POINT('Ctrl Pts',(-1.42999922978895,6.61707018861855,3.26492969654252));
#9849=CARTESIAN_POINT('Ctrl Pts',(-1.62066601233743,6.57297172934401,3.27412650690992));
#9850=CARTESIAN_POINT('Ctrl Pts',(-1.80906628500433,6.52070304311281,3.28332331727731));
#9851=CARTESIAN_POINT('Ctrl Pts',(-1.98831342545571,6.47097374915017,3.29207331501507));
#9852=CARTESIAN_POINT('Ctrl Pts',(-2.16550875896742,6.41384933989515,3.30082331275283));
#9853=CARTESIAN_POINT('Ctrl Pts',(-2.34005036714047,6.34952386240462,3.30957331049059));
#9854=CARTESIAN_POINT('Ctrl Pts',(-2.51458843547124,6.28519968948582,3.31832313077146));
#9855=CARTESIAN_POINT('Ctrl Pts',(-2.6864726171809,6.21367483971084,3.32707295105232));
#9856=CARTESIAN_POINT('Ctrl Pts',(-2.85511905908764,6.13519226743828,3.33582277133319));
#9857=CARTESIAN_POINT('Ctrl Pts',(-3.02376230488918,6.0567111825292,3.34457242579172));
#9858=CARTESIAN_POINT('Ctrl Pts',(-3.18916767379939,5.97127275992615,3.35332208025025));
#9859=CARTESIAN_POINT('Ctrl Pts',(-3.35077334102822,5.87916720437977,3.36207173470879));
#9860=CARTESIAN_POINT('Ctrl Pts',(-3.51237616037398,5.78706327195624,3.37082123497723));
#9861=CARTESIAN_POINT('Ctrl Pts',(-3.67017916302325,5.68829258362281,3.37957073524567));
#9862=CARTESIAN_POINT('Ctrl Pts',(-3.82364636566484,5.58319061741027,3.38832023551411));
#9863=CARTESIAN_POINT('Ctrl Pts',(-3.9771110677882,5.47809036367686,3.39706959322255));
#9864=CARTESIAN_POINT('Ctrl Pts',(-4.12623987481949,5.36665920043208,3.40581895093099));
#9865=CARTESIAN_POINT('Ctrl Pts',(-4.27052628213952,5.24927559512316,3.41456830863943));
#9866=CARTESIAN_POINT('Ctrl Pts',(-4.41481053025008,5.13189374643011,3.42331753541595));
#9867=CARTESIAN_POINT('Ctrl Pts',(-4.55425230136567,5.0085598147732,3.43206676219247));
#9868=CARTESIAN_POINT('Ctrl Pts',(-4.68837800630591,4.87969268192035,3.44081598896899));
#9869=CARTESIAN_POINT('Ctrl Pts',(-4.82250188228962,4.75082730631742,3.44956509643985));
#9870=CARTESIAN_POINT('Ctrl Pts',(-4.95130963053056,4.61642907903431,3.45831420391071));
#9871=CARTESIAN_POINT('Ctrl Pts',(-5.07436379033477,4.47695444731565,3.46706331138157));
#9872=CARTESIAN_POINT('Ctrl Pts',(-5.19741643562917,4.33748153220453,3.47581231117132));
#9873=CARTESIAN_POINT('Ctrl Pts',(-5.31471544462885,4.19293255254448,3.48456131096107));
#9874=CARTESIAN_POINT('Ctrl Pts',(-5.42586245275739,4.04379841779453,3.49331031075082));
#9875=CARTESIAN_POINT('Ctrl Pts',(-5.53702160019253,3.89464799484199,3.50206026609297));
#9876=CARTESIAN_POINT('Ctrl Pts',(-5.64202723081342,3.74091164443713,3.51081022143512));
#9877=CARTESIAN_POINT('Ctrl Pts',(-5.74052265233048,3.58311159163103,3.51956017677727));
#9878=CARTESIAN_POINT('Ctrl Pts',(-5.83901427066995,3.42531763191653,3.52830979425972));
#9879=CARTESIAN_POINT('Ctrl Pts',(-5.93099603115812,3.26346052695481,3.53705941174217));
#9880=CARTESIAN_POINT('Ctrl Pts',(-6.01615550622822,3.09809004466944,3.54580902922461));
#9881=CARTESIAN_POINT('Ctrl Pts',(-6.10131214578869,2.93272506863683,3.55455835537571));
#9882=CARTESIAN_POINT('Ctrl Pts',(-6.17964682328819,2.76384720416736,3.56330768152681));
#9883=CARTESIAN_POINT('Ctrl Pts',(-6.25089348288635,2.59203002791423,3.57205700767791));
#9884=CARTESIAN_POINT('Ctrl Pts',(-6.32213814889406,2.42021765936833,3.58080608900949));
#9885=CARTESIAN_POINT('Ctrl Pts',(-6.38629508412663,2.24546640831697,3.58955517034107));
#9886=CARTESIAN_POINT('Ctrl Pts',(-6.44314639819891,2.06836976659795,3.59830425167265));
#9887=CARTESIAN_POINT('Ctrl Pts',(-6.50000285283774,1.89125711158024,3.60705412410705));
#9888=CARTESIAN_POINT('Ctrl Pts',(-6.54955227673317,1.71179891439998,3.61580399654145));
#9889=CARTESIAN_POINT('Ctrl Pts',(-6.59162635926446,1.53060476278169,3.62455386897585));
#9890=CARTESIAN_POINT('Ctrl Pts',(-6.63369752055247,1.34942319164445,3.63330313389834));
#9891=CARTESIAN_POINT('Ctrl Pts',(-6.66829431424295,1.16650618642466,3.64205239882084));
#9892=CARTESIAN_POINT('Ctrl Pts',(-6.6952992374545,0.982474997616297,3.65080166374333));
#9893=CARTESIAN_POINT('Ctrl Pts',(-6.72230554731469,0.798434359175536,3.65955137792303));
#9894=CARTESIAN_POINT('Ctrl Pts',(-6.74171916496722,0.613279706238185,3.66830109210272));
#9895=CARTESIAN_POINT('Ctrl Pts',(-6.75347414817288,0.427639953653287,3.67705080628242));
#9896=CARTESIAN_POINT('Ctrl Pts',(-6.76248837758749,0.285283364197234,3.68376046545829));
#9897=CARTESIAN_POINT('Ctrl Pts',(-6.76699999999996,0.142641701104535,3.69047012463415));
#9898=CARTESIAN_POINT('Ctrl Pts',(-6.767,1.74262956926013E-12,3.69717978381002));
#9899=CARTESIAN_POINT('',(-6.76699897167863,0.00373058981880235,3.30282021616294));
#9900=CARTESIAN_POINT('Ctrl Pts',(3.09917575053259,6.01559628526639,2.65160425626863));
#9901=CARTESIAN_POINT('Ctrl Pts',(2.94520675288169,6.09491959109098,2.65972997863448));
#9902=CARTESIAN_POINT('Ctrl Pts',(2.78810984876472,6.16836926240051,2.66785570100033));
#9903=CARTESIAN_POINT('Ctrl Pts',(2.62837909668337,6.23569661899277,2.67598142336617));
#9904=CARTESIAN_POINT('Ctrl Pts',(2.46866863440386,6.30301542332628,2.68410611356198));
#9905=CARTESIAN_POINT('Ctrl Pts',(2.30632532403241,6.36421331269895,2.69223080375779));
#9906=CARTESIAN_POINT('Ctrl Pts',(2.14186485538603,6.41908902736691,2.7003554939536));
#9907=CARTESIAN_POINT('Ctrl Pts',(1.97740802041331,6.47396352958277,2.70848000463836));
#9908=CARTESIAN_POINT('Ctrl Pts',(1.81083446692612,6.5225160187193,2.71660451532311));
#9909=CARTESIAN_POINT('Ctrl Pts',(1.64267658948007,6.56459462742172,2.72472902600786));
#9910=CARTESIAN_POINT('Ctrl Pts',(1.47449045949953,6.60668030583364,2.73285490170757));
#9911=CARTESIAN_POINT('Ctrl Pts',(1.30471983022654,6.6422898490823,2.74098077740728));
#9912=CARTESIAN_POINT('Ctrl Pts',(1.13390883005738,6.67132219017474,2.74910665310699));
#9913=CARTESIAN_POINT('Ctrl Pts',(0.963036657325268,6.70036492862281,2.75723543892749));
#9914=CARTESIAN_POINT('Ctrl Pts',(0.791123732014469,6.72282571346218,2.76536422474799));
#9915=CARTESIAN_POINT('Ctrl Pts',(0.618720828427367,6.7386551726936,2.77349301056849));
#9916=CARTESIAN_POINT('Ctrl Pts',(0.446129455341023,6.75450193656543,2.78163068271377));
#9917=CARTESIAN_POINT('Ctrl Pts',(0.273047398515536,6.7637028639598,2.78976835485904));
#9918=CARTESIAN_POINT('Ctrl Pts',(0.10002782907235,6.76626066844983,2.79790602700432));
#9919=CARTESIAN_POINT('Ctrl Pts',(-0.0730973733828469,6.76882003454697,
2.80604866741314));
#9920=CARTESIAN_POINT('Ctrl Pts',(-0.246159647961955,6.76472820531347,2.81419130782195));
#9921=CARTESIAN_POINT('Ctrl Pts',(-0.418609710536651,6.75403989551768,2.82233394823077));
#9922=CARTESIAN_POINT('Ctrl Pts',(-0.591303279505669,6.74333649340043,2.83048808637393));
#9923=CARTESIAN_POINT('Ctrl Pts',(-0.763382547419845,6.72601804475287,2.83864222451709));
#9924=CARTESIAN_POINT('Ctrl Pts',(-0.934306249721319,6.70219074868298,2.84679636266025));
#9925=CARTESIAN_POINT('Ctrl Pts',(-1.02815752174827,6.68910758926733,2.85127365999651));
#9926=CARTESIAN_POINT('Ctrl Pts',(-1.12166061344754,6.67406295807002,2.85575095733278));
#9927=CARTESIAN_POINT('Ctrl Pts',(-1.21472783458636,6.65708083831653,2.86022825466904));
#9928=CARTESIAN_POINT('Ctrl Pts',(-1.38571430848921,6.62588067202261,2.86845410771133));
#9929=CARTESIAN_POINT('Ctrl Pts',(-1.55573714104419,6.58804497094957,2.87667996075363));
#9930=CARTESIAN_POINT('Ctrl Pts',(-1.72424274715405,6.54364393506299,2.88490581379592));
#9931=CARTESIAN_POINT('Ctrl Pts',(-1.89255898443555,6.49929279764767,2.89312242251579));
#9932=CARTESIAN_POINT('Ctrl Pts',(-2.05936104686051,6.44839110797352,2.90133903123566));
#9933=CARTESIAN_POINT('Ctrl Pts',(-2.22410326461305,6.39106044943541,2.90955563995553));
#9934=CARTESIAN_POINT('Ctrl Pts',(-2.38869341676192,6.33378271006592,2.91776466431978));
#9935=CARTESIAN_POINT('Ctrl Pts',(-2.55122717421177,6.2700879372776,2.92597368868403));
#9936=CARTESIAN_POINT('Ctrl Pts',(-2.71117172540353,6.20014813334105,2.93418271304828));
#9937=CARTESIAN_POINT('Ctrl Pts',(-2.87100073986314,6.13025885076539,2.94238580758346));
#9938=CARTESIAN_POINT('Ctrl Pts',(-3.02824394613097,6.05413366553863,2.95058890211865));
#9939=CARTESIAN_POINT('Ctrl Pts',(-3.18238621523416,5.97199355132669,2.95879199665383));
#9940=CARTESIAN_POINT('Ctrl Pts',(-3.33644806769062,5.88989628994536,2.96699081160133));
#9941=CARTESIAN_POINT('Ctrl Pts',(-3.48741189008429,5.80179051932399,2.97518962654884));
#9942=CARTESIAN_POINT('Ctrl Pts',(-3.63478489442442,5.70794426840908,2.98338844149634));
#9943=CARTESIAN_POINT('Ctrl Pts',(-3.7821301124861,5.6141157116307,2.99158571060744));
#9944=CARTESIAN_POINT('Ctrl Pts',(-3.92588555548995,5.51454901765805,2.99978297971854));
#9945=CARTESIAN_POINT('Ctrl Pts',(-4.06558503985017,5.40955703211885,3.00798024882964));
#9946=CARTESIAN_POINT('Ctrl Pts',(-4.20527443122158,5.30457263202594,3.01617692570559));
#9947=CARTESIAN_POINT('Ctrl Pts',(-4.34090816025273,5.19416393579372,3.02437360258154));
#9948=CARTESIAN_POINT('Ctrl Pts',(-4.47205097788837,5.07868576023046,3.03257027945749));
#9949=CARTESIAN_POINT('Ctrl Pts',(-4.60320816200925,4.96319493421837,3.04076785426624));
#9950=CARTESIAN_POINT('Ctrl Pts',(-4.72987318530872,4.84263375956345,3.04896542907498));
#9951=CARTESIAN_POINT('Ctrl Pts',(-4.85164566609175,4.71739582086273,3.05716300388373));
#9952=CARTESIAN_POINT('Ctrl Pts',(-4.97345362471786,4.59212139467397,3.06536296701758));
#9953=CARTESIAN_POINT('Ctrl Pts',(-5.09036595156392,4.46216774752229,3.07356293015143));
#9954=CARTESIAN_POINT('Ctrl Pts',(-5.20202072554249,4.32796365176816,3.08176289328529));
#9955=CARTESIAN_POINT('Ctrl Pts',(-5.31379188115593,4.19361967044072,3.08997140352448));
#9956=CARTESIAN_POINT('Ctrl Pts',(-5.42029430570767,4.05501666538604,3.09817991376367));
#9957=CARTESIAN_POINT('Ctrl Pts',(-5.52120722161112,3.91261546999309,3.10638842400287));
#9958=CARTESIAN_POINT('Ctrl Pts',(-5.62217430664552,3.77013783493995,3.11460134049534));
#9959=CARTESIAN_POINT('Ctrl Pts',(-5.71754570592351,3.62385824527043,3.12281425698781));
#9960=CARTESIAN_POINT('Ctrl Pts',(-5.80704532664466,3.47426446522057,3.13102717348027));
#9961=CARTESIAN_POINT('Ctrl Pts',(-5.89667590943826,3.32445178914297,3.13925210768361));
#9962=CARTESIAN_POINT('Ctrl Pts',(-5.98041737103897,3.1713155458808,3.14747704188695));
#9963=CARTESIAN_POINT('Ctrl Pts',(-6.05804014883562,3.01536706805253,3.15570197609028));
#9964=CARTESIAN_POINT('Ctrl Pts',(-6.128284741187,2.8742417751448,3.1631451154191));
#9965=CARTESIAN_POINT('Ctrl Pts',(-6.19351909483421,2.73081390417555,3.17058825474792));
#9966=CARTESIAN_POINT('Ctrl Pts',(-6.25360800368249,2.58547402545033,3.17803139407673));
#9967=CARTESIAN_POINT('Ctrl Pts',(-6.32747811552127,2.40680090087797,3.18718159409184));
#9968=CARTESIAN_POINT('Ctrl Pts',(-6.39374764619014,2.22481332471955,3.19633179410695));
#9969=CARTESIAN_POINT('Ctrl Pts',(-6.45214081017707,2.04013920251721,3.20548199412205));
#9970=CARTESIAN_POINT('Ctrl Pts',(-6.510302139696,1.8561982796134,3.21459586571089));
#9971=CARTESIAN_POINT('Ctrl Pts',(-6.56064941685709,1.66959229364365,3.22370973729973));
#9972=CARTESIAN_POINT('Ctrl Pts',(-6.60295632276621,1.48096482052808,3.23282360888856));
#9973=CARTESIAN_POINT('Ctrl Pts',(-6.64515326820406,1.29282761171784,3.2419137924862));
#9974=CARTESIAN_POINT('Ctrl Pts',(-6.67935147609421,1.10267960418178,3.25100397608384));
#9975=CARTESIAN_POINT('Ctrl Pts',(-6.70537402831222,0.911179532494014,3.26009415968147));
#9976=CARTESIAN_POINT('Ctrl Pts',(-6.73128437064188,0.720505213848521,3.26914514618276));
#9977=CARTESIAN_POINT('Ctrl Pts',(-6.74908932618658,0.528490671122382,3.27819613268405));
#9978=CARTESIAN_POINT('Ctrl Pts',(-6.75866297586654,0.335803184396522,3.28724711918534));
#9979=CARTESIAN_POINT('Ctrl Pts',(-6.76415377236239,0.225290703548003,3.2924381515112));
#9980=CARTESIAN_POINT('Ctrl Pts',(-6.76693787391787,0.114557162636319,3.29762918383707));
#9981=CARTESIAN_POINT('Ctrl Pts',(-6.76699897167863,0.00373058981880468,
3.30282021616294));
#9982=CARTESIAN_POINT('Ctrl Pts',(-6.76699897167895,0.00373058924357801,
3.30282021618988));
#9983=CARTESIAN_POINT('Ctrl Pts',(-6.76709684169258,-0.173798009695901,
3.31113552065549));
#9984=CARTESIAN_POINT('Ctrl Pts',(-6.76020431043818,-0.351321971043665,
3.31945082512111));
#9985=CARTESIAN_POINT('Ctrl Pts',(-6.74634909808389,-0.528263993456603,
3.32776612958672));
#9986=CARTESIAN_POINT('Ctrl Pts',(-6.73249065934686,-0.705247219329472,
3.33608337038893));
#9987=CARTESIAN_POINT('Ctrl Pts',(-6.71166633374003,-0.88164789311043,3.34440061119115));
#9988=CARTESIAN_POINT('Ctrl Pts',(-6.68395576145156,-1.05689374061849,3.35271785199336));
#9989=CARTESIAN_POINT('Ctrl Pts',(-6.65623432495978,-1.23220829499037,3.3610383536519));
#9990=CARTESIAN_POINT('Ctrl Pts',(-6.62162131335795,-1.40636678086737,3.36935885531044));
#9991=CARTESIAN_POINT('Ctrl Pts',(-6.5802475750166,-1.57880678092292,3.37767935696899));
#9992=CARTESIAN_POINT('Ctrl Pts',(-6.53885102718628,-1.75134184776324,3.38600444574966));
#9993=CARTESIAN_POINT('Ctrl Pts',(-6.49068640260336,-1.92215620608231,3.39432953453034));
#9994=CARTESIAN_POINT('Ctrl Pts',(-6.4359345866935,-2.09070203419866,3.40265462331101));
#9995=CARTESIAN_POINT('Ctrl Pts',(-6.38110929144823,-2.25947405819964,3.41099088472552));
#9996=CARTESIAN_POINT('Ctrl Pts',(-6.31967924721766,-2.42597114142646,3.41932714614002));
#9997=CARTESIAN_POINT('Ctrl Pts',(-6.25187420606412,-2.58966366765071,3.42766340755453));
#9998=CARTESIAN_POINT('Ctrl Pts',(-6.18402023240115,-2.75347432500427,3.43600568495521));
#9999=CARTESIAN_POINT('Ctrl Pts',(-6.10978223002811,-2.91447607712649,3.44434796235589));
#10000=CARTESIAN_POINT('Ctrl Pts',(-6.02943630481958,-3.07216321931691,
3.45269023975658));
#10001=CARTESIAN_POINT('Ctrl Pts',(-5.94896154971195,-3.2301032034351,3.46104589350152));
#10002=CARTESIAN_POINT('Ctrl Pts',(-5.86235946643278,-3.38471765599889,
3.46940154724647));
#10003=CARTESIAN_POINT('Ctrl Pts',(-5.769950702733,-3.53552795039594,3.47775720099142));
#10004=CARTESIAN_POINT('Ctrl Pts',(-5.70330904118431,-3.64428655937289,
3.48378297848908));
#10005=CARTESIAN_POINT('Ctrl Pts',(-5.63364838875367,-3.75106733002901,
3.48980875598674));
#10006=CARTESIAN_POINT('Ctrl Pts',(-5.56110198131188,-3.85570146062284,
3.4958345334844));
#10007=CARTESIAN_POINT('Ctrl Pts',(-5.46294839384705,-3.99726898479401,
3.50398726908519));
#10008=CARTESIAN_POINT('Ctrl Pts',(-5.35923204261449,-4.13530739791128,
3.51214000468598));
#10009=CARTESIAN_POINT('Ctrl Pts',(-5.25023597555782,-4.2693455237259,3.52029274028678));
#10010=CARTESIAN_POINT('Ctrl Pts',(-5.14136615543722,-4.40322839712494,
3.5284360328139));
#10011=CARTESIAN_POINT('Ctrl Pts',(-5.02722902094046,-4.53311992577148,
3.53657932534103));
#10012=CARTESIAN_POINT('Ctrl Pts',(-4.90815148857804,-4.65857681756662,
3.54472261786816));
#10013=CARTESIAN_POINT('Ctrl Pts',(-4.78918684827596,-4.78391476931726,
3.55285819010539));
#10014=CARTESIAN_POINT('Ctrl Pts',(-4.66529138482328,-4.9048261910985,3.56099376234261));
#10015=CARTESIAN_POINT('Ctrl Pts',(-4.53683296001558,-5.02089988875662,
3.56912933457983));
#10016=CARTESIAN_POINT('Ctrl Pts',(-4.40846933145566,-5.13688792951043,
3.57725890314915));
#10017=CARTESIAN_POINT('Ctrl Pts',(-4.27554971641228,-5.24804511062683,
3.58538847171847));
#10018=CARTESIAN_POINT('Ctrl Pts',(-4.13847958908387,-5.35399623559227,
3.59351804028779));
#10019=CARTESIAN_POINT('Ctrl Pts',(-4.00148182471231,-5.45989142614784,
3.60164331704218));
#10020=CARTESIAN_POINT('Ctrl Pts',(-3.86033820042873,-5.560585811085,3.60976859379657));
#10021=CARTESIAN_POINT('Ctrl Pts',(-3.71548809435513,-5.65574373718482,
3.61789387055095));
#10022=CARTESIAN_POINT('Ctrl Pts',(-3.57009042878715,-5.75126137738712,
3.62604986231517));
#10023=CARTESIAN_POINT('Ctrl Pts',(-3.42095848583829,-5.84120037585115,
3.63420585407938));
#10024=CARTESIAN_POINT('Ctrl Pts',(-3.26856735302294,-5.92526425222982,
3.64236184584359));
#10025=CARTESIAN_POINT('Ctrl Pts',(-3.11678391566199,-6.00899290414622,
3.65048531367397));
#10026=CARTESIAN_POINT('Ctrl Pts',(-2.96176756699753,-6.08689304547798,
3.65860878150434));
#10027=CARTESIAN_POINT('Ctrl Pts',(-2.80401345750796,-6.15871719842,3.66673224933472));
#10028=CARTESIAN_POINT('Ctrl Pts',(-2.64623832554524,-6.23055092272172,
3.67485679970668));
#10029=CARTESIAN_POINT('Ctrl Pts',(-2.48572503902925,-6.29630689428214,
3.68298135007864));
#10030=CARTESIAN_POINT('Ctrl Pts',(-2.32298971280541,-6.35578537980951,
3.69110590045061));
#10031=CARTESIAN_POINT('Ctrl Pts',(-2.16020174222565,-6.4152831064361,3.69923307908855));
#10032=CARTESIAN_POINT('Ctrl Pts',(-1.99519064393342,-6.46849917765662,
3.70736025772649));
#10033=CARTESIAN_POINT('Ctrl Pts',(-1.82848866297087,-6.51528343277459,
3.71548743636443));
#10034=CARTESIAN_POINT('Ctrl Pts',(-1.66071991658294,-6.56236707141232,
3.72366662274174));
#10035=CARTESIAN_POINT('Ctrl Pts',(-1.49123893429748,-6.60293619267932,
3.73184580911904));
#10036=CARTESIAN_POINT('Ctrl Pts',(-1.32059876411721,-6.63688992708272,
3.74002499549634));
#10037=CARTESIAN_POINT('Ctrl Pts',(-1.15075111353853,-6.67068596708139,
3.74816619453736));
#10038=CARTESIAN_POINT('Ctrl Pts',(-0.979755390533758,-6.69792794448416,
3.75630739357837));
#10039=CARTESIAN_POINT('Ctrl Pts',(-0.808161859079969,-6.71856855360786,
3.76444859261939));
#10040=CARTESIAN_POINT('Ctrl Pts',(-0.635367328642229,-6.73935362826226,
3.77264677266483));
#10041=CARTESIAN_POINT('Ctrl Pts',(-0.46196696728385,-6.75344456246767,
3.78084495271028));
#10042=CARTESIAN_POINT('Ctrl Pts',(-0.288522019283917,-6.76084639999966,
3.78904313275573));
#10043=CARTESIAN_POINT('Ctrl Pts',(-0.115077071283985,-6.76824823753165,
3.79724131280118));
#10044=CARTESIAN_POINT('Ctrl Pts',(0.0584120919248692,-6.7689610416055,
3.80543949284662));
#10045=CARTESIAN_POINT('Ctrl Pts',(0.231390498827155,-6.76304276469198,
3.81363767289207));
#10046=CARTESIAN_POINT('Ctrl Pts',(0.405103527568918,-6.7570993534536,3.82187066978092));
#10047=CARTESIAN_POINT('Ctrl Pts',(0.578841395616977,-6.74445006384751,
3.83010366666977));
#10048=CARTESIAN_POINT('Ctrl Pts',(0.752046094964177,-6.72508109029543,
3.83833666355863));
#10049=CARTESIAN_POINT('Ctrl Pts',(0.925044525674072,-6.70573518316012,
3.84655985581137));
#10050=CARTESIAN_POINT('Ctrl Pts',(1.09751069954499,-6.67968556632619,3.85478304806411));
#10051=CARTESIAN_POINT('Ctrl Pts',(1.26888665828042,-6.64697041128046,3.86300624031686));
#10052=CARTESIAN_POINT('Ctrl Pts',(1.44009282883251,-6.61428766828823,3.87122128556413));
#10053=CARTESIAN_POINT('Ctrl Pts',(1.61021058589455,-6.57495260529816,3.8794363308114));
#10054=CARTESIAN_POINT('Ctrl Pts',(1.77868704744523,-6.52905516803546,3.88765137605867));
#10055=CARTESIAN_POINT('Ctrl Pts',(1.94703030351596,-6.4831940194632,3.89585992610159));
#10056=CARTESIAN_POINT('Ctrl Pts',(2.11373450476834,-6.43078092484251,3.90406847614452));
#10057=CARTESIAN_POINT('Ctrl Pts',(2.27825682815937,-6.37195690702199,3.91227702618745));
#10058=CARTESIAN_POINT('Ctrl Pts',(2.44268198274175,-6.31316763135447,3.9204807281647));
#10059=CARTESIAN_POINT('Ctrl Pts',(2.60492749024062,-6.24797509570972,3.92868443014195));
#10060=CARTESIAN_POINT('Ctrl Pts',(2.76446547667916,-6.17657021560098,3.93688813211921));
#10061=CARTESIAN_POINT('Ctrl Pts',(2.92395625777821,-6.10518646332317,3.94508940672135));
#10062=CARTESIAN_POINT('Ctrl Pts',(3.08074078552628,-6.02759417073968,3.9532906813235));
#10063=CARTESIAN_POINT('Ctrl Pts',(3.234310741282,-5.9440325561716,3.96149195592565));
#10064=CARTESIAN_POINT('Ctrl Pts',(3.38785951728152,-5.86048246608834,3.96969209944069));
#10065=CARTESIAN_POINT('Ctrl Pts',(3.53819428927971,-5.77096486415899,3.97789224295573));
#10066=CARTESIAN_POINT('Ctrl Pts',(3.68483093413852,-5.675765145495,3.98609238647077));
#10067=CARTESIAN_POINT('Ctrl Pts',(3.83147393003582,-5.58056130359784,3.99429288514552));
#10068=CARTESIAN_POINT('Ctrl Pts',(3.9744181791317,-5.47967504973398,4.00249338382026));
#10069=CARTESIAN_POINT('Ctrl Pts',(4.11320812387964,-5.37343539364255,4.01069388249501));
#10070=CARTESIAN_POINT('Ctrl Pts',(4.25202923225124,-5.26717188270585,4.01889622249374));
#10071=CARTESIAN_POINT('Ctrl Pts',(4.38669389395538,-5.15555279314839,4.02709856249247));
#10072=CARTESIAN_POINT('Ctrl Pts',(4.51677920984576,-5.03894776411753,4.0353009024912));
#10073=CARTESIAN_POINT('Ctrl Pts',(4.64698618487179,-4.92223368306227,4.04351091352941));
#10074=CARTESIAN_POINT('Ctrl Pts',(4.77260499042225,-4.80052458574869,4.05172092456763));
#10075=CARTESIAN_POINT('Ctrl Pts',(4.89324855634459,-4.67422801816852,4.05993093560584));
#10076=CARTESIAN_POINT('Ctrl Pts',(5.01394986229968,-4.54787100502797,4.06814487595685));
#10077=CARTESIAN_POINT('Ctrl Pts',(5.12967094387691,-4.41692241235564,4.07635881630785));
#10078=CARTESIAN_POINT('Ctrl Pts',(5.24006477789551,-4.28182322421874,4.08457275665885));
#10079=CARTESIAN_POINT('Ctrl Pts',(5.35060912579644,-4.1465398382642,4.09279789611407));
#10080=CARTESIAN_POINT('Ctrl Pts',(5.45581149447148,-4.00709483329603,4.10102303556928));
#10081=CARTESIAN_POINT('Ctrl Pts',(5.55536728286152,-3.86395954333269,4.1092481750245));
#10082=CARTESIAN_POINT('Ctrl Pts',(5.64490600790569,-3.7352261810702,4.11664572078291));
#10083=CARTESIAN_POINT('Ctrl Pts',(5.72987777030852,-3.60350832328702,4.12404326654133));
#10084=CARTESIAN_POINT('Ctrl Pts',(5.81009297579069,-3.46916540578101,4.13144081229974));
#10085=CARTESIAN_POINT('Ctrl Pts',(5.90384440396677,-3.31215227708771,4.14008668530699));
#10086=CARTESIAN_POINT('Ctrl Pts',(5.99131091009206,-3.15119672324539,4.14873255831424));
#10087=CARTESIAN_POINT('Ctrl Pts',(6.07216684534548,-2.98681750401446,4.15737843132149));
#10088=CARTESIAN_POINT('Ctrl Pts',(6.15291935100299,-2.82264855600438,4.16601324466876));
#10089=CARTESIAN_POINT('Ctrl Pts',(6.22707801385425,-2.65506494791864,4.17464805801603));
#10090=CARTESIAN_POINT('Ctrl Pts',(6.29436207283328,-2.48461165900789,4.1832828713633));
#10091=CARTESIAN_POINT('Ctrl Pts',(6.36388102804483,-2.30849662169808,4.19220449724999));
#10092=CARTESIAN_POINT('Ctrl Pts',(6.42606064646887,-2.12931824850697,4.20112612313668));
#10093=CARTESIAN_POINT('Ctrl Pts',(6.48064306107319,-1.9477049352928,4.21004774902337));
#10094=CARTESIAN_POINT('Ctrl Pts',(6.53332486058637,-1.77241558202708,4.21865871483903));
#10095=CARTESIAN_POINT('Ctrl Pts',(6.5789294816883,-1.59485832255998,4.2272696806547));
#10096=CARTESIAN_POINT('Ctrl Pts',(6.61727384809151,-1.41561852889973,4.23588064647036));
#10097=CARTESIAN_POINT('Ctrl Pts',(6.65558205665078,-1.23654775418788,4.24448349234593));
#10098=CARTESIAN_POINT('Ctrl Pts',(6.68664359655048,-1.05579790576891,4.2530863382215));
#10099=CARTESIAN_POINT('Ctrl Pts',(6.71032549532368,-0.87396839005139,4.26168918409707));
#10100=CARTESIAN_POINT('Ctrl Pts',(6.73398087924588,-0.692342455244416,
4.27028239800948));
#10101=CARTESIAN_POINT('Ctrl Pts',(6.75027306605747,-0.509639566479221,
4.27887561192189));
#10102=CARTESIAN_POINT('Ctrl Pts',(6.75912031192382,-0.326468388881435,
4.2874688258343));
#10103=CARTESIAN_POINT('Ctrl Pts',(6.76010647993188,-0.306051011759411,
4.28842667789073));
#10104=CARTESIAN_POINT('Ctrl Pts',(6.76100019942572,-0.28562782510727,4.28938452994716));
#10105=CARTESIAN_POINT('Ctrl Pts',(6.76180139687412,-0.26519967803756,4.29034238200358));
#10106=CARTESIAN_POINT('Ctrl Pts',(6.76899140555886,-0.0818758854607504,
4.29893822141634));
#10107=CARTESIAN_POINT('Ctrl Pts',(6.76871754992939,0.101632850524437,4.3075340608291));
#10108=CARTESIAN_POINT('Ctrl Pts',(6.76100790797412,0.284712255288441,4.31612990024186));
#10109=CARTESIAN_POINT('Ctrl Pts',(6.75329107009757,0.467962540229786,4.32473376272289));
#10110=CARTESIAN_POINT('Ctrl Pts',(6.73812460561502,0.650782389070587,4.33333762520391));
#10111=CARTESIAN_POINT('Ctrl Pts',(6.71558847263786,0.832562589943548,4.34194148768494));
#10112=CARTESIAN_POINT('Ctrl Pts',(6.69216698990923,1.02148416932313,4.35088335968682));
#10113=CARTESIAN_POINT('Ctrl Pts',(6.66078514618406,1.20928239056665,4.35982523168869));
#10114=CARTESIAN_POINT('Ctrl Pts',(6.62159082338148,1.39528633896783,4.36876710369056));
#10115=CARTESIAN_POINT('Ctrl Pts',(6.58377537545608,1.57474658018979,4.37739439639174));
#10116=CARTESIAN_POINT('Ctrl Pts',(6.53868789761558,1.75253636908757,4.38602168909292));
#10117=CARTESIAN_POINT('Ctrl Pts',(6.48651197892727,1.92806933154205,4.3946489817941));
#10118=CARTESIAN_POINT('Ctrl Pts',(6.43428636139952,2.10376949343908,4.40328449220271));
#10119=CARTESIAN_POINT('Ctrl Pts',(6.37495892132687,2.27720824858467,4.41192000261132));
#10120=CARTESIAN_POINT('Ctrl Pts',(6.30876192969389,2.44781778620163,4.42055551301993));
#10121=CARTESIAN_POINT('Ctrl Pts',(6.24246713047884,2.61867940334578,4.42920378259436));
#10122=CARTESIAN_POINT('Ctrl Pts',(6.16928261451574,2.78670316820374,4.43785205216879));
#10123=CARTESIAN_POINT('Ctrl Pts',(6.08948787542499,2.9513431544048,4.44650032174322));
#10124=CARTESIAN_POINT('Ctrl Pts',(6.0810496849766,2.96875361999207,4.44741486506461));
#10125=CARTESIAN_POINT('Ctrl Pts',(6.07253761502701,2.98612627013083,4.44832940838601));
#10126=CARTESIAN_POINT('Ctrl Pts',(6.06395202511095,3.00346047704191,4.44924395170741));
#10127=CARTESIAN_POINT('Ctrl Pts',(5.98492975694224,3.16300552408128,4.45766146154679));
#10128=CARTESIAN_POINT('Ctrl Pts',(5.89950056531221,3.31964412149655,4.46607897138617));
#10129=CARTESIAN_POINT('Ctrl Pts',(5.80790468167551,3.47282769635519,4.47449648122555));
#10130=CARTESIAN_POINT('Ctrl Pts',(5.71849559537438,3.62235410431883,4.48271302801552));
#10131=CARTESIAN_POINT('Ctrl Pts',(5.62321108275568,3.76858823202246,4.49092957480549));
#10132=CARTESIAN_POINT('Ctrl Pts',(5.52232284465145,3.91104070541854,4.49914612159546));
#10133=CARTESIAN_POINT('Ctrl Pts',(5.42151524506533,4.05337931860087,4.50735610101772));
#10134=CARTESIAN_POINT('Ctrl Pts',(5.31511304438239,4.19194200544041,4.51556608043998));
#10135=CARTESIAN_POINT('Ctrl Pts',(5.20343264862878,4.32626601946576,4.52377605986224));
#10136=CARTESIAN_POINT('Ctrl Pts',(5.09182127392538,4.46050701816461,4.53198096532862));
#10137=CARTESIAN_POINT('Ctrl Pts',(4.97493842906929,4.59051428673738,4.54018587079499));
#10138=CARTESIAN_POINT('Ctrl Pts',(4.85314245757157,4.7158559442074,4.54839077626136));
#10139=CARTESIAN_POINT('Ctrl Pts',(4.72588558709957,4.84681747662315,4.55696356056062));
#10140=CARTESIAN_POINT('Ctrl Pts',(4.59326508132317,4.9726850335613,4.56553634485988));
#10141=CARTESIAN_POINT('Ctrl Pts',(4.45573544088481,5.09300605544929,4.57410912915914));
#10142=CARTESIAN_POINT('Ctrl Pts',(4.32418742979502,5.20809390902911,4.58230905406606));
#10143=CARTESIAN_POINT('Ctrl Pts',(4.1881485802155,5.31810724398039,4.59050897897297));
#10144=CARTESIAN_POINT('Ctrl Pts',(4.0480528287496,5.42268912032142,4.59870890387989));
#10145=CARTESIAN_POINT('Ctrl Pts',(3.90796767698092,5.52726308395839,4.6069082083774));
#10146=CARTESIAN_POINT('Ctrl Pts',(3.76382652423189,5.62640619670433,4.61510751287492));
#10147=CARTESIAN_POINT('Ctrl Pts',(3.61609443087256,5.71980332415481,4.62330681737243));
#10148=CARTESIAN_POINT('Ctrl Pts',(3.46832615795948,5.81322332453911,4.63150812987763));
#10149=CARTESIAN_POINT('Ctrl Pts',(3.31696549318485,5.90089434166774,4.63970944238282));
#10150=CARTESIAN_POINT('Ctrl Pts',(3.16250461406014,5.98254574291315,4.64791075488801));
#10151=CARTESIAN_POINT('Ctrl Pts',(3.14145212181365,5.99367455107077,4.64902856587618));
#10152=CARTESIAN_POINT('Ctrl Pts',(3.12034207408623,6.00469160457064,4.65014637686434));
#10153=CARTESIAN_POINT('Ctrl Pts',(3.09917575053259,6.01559628526639,4.6512641878525));
#10154=CARTESIAN_POINT('Origin',(0.,0.,-3.69717978381041));
#10155=CARTESIAN_POINT('',(3.09917575053257,6.0155962852664,7.04594397030302));
#10156=CARTESIAN_POINT('',(3.0991757505326,6.01559628526638,6.65133473543275));
#10157=CARTESIAN_POINT('',(3.09917575053259,6.01559628526639,-3.69717978381041));
#10158=CARTESIAN_POINT('',(-6.76699981083753,-0.00160003901735913,5.69717978376657));
#10159=CARTESIAN_POINT('Ctrl Pts',(-6.76699981083731,-0.00160003993641796,
5.69717978381002));
#10160=CARTESIAN_POINT('Ctrl Pts',(-6.76698820601404,-0.0506799629623293,
5.69950000820113));
#10161=CARTESIAN_POINT('Ctrl Pts',(-6.76644265511029,-0.0997553428157312,
5.70182023259224));
#10162=CARTESIAN_POINT('Ctrl Pts',(-6.76536341443635,-0.148818246885836,
5.70414045698336));
#10163=CARTESIAN_POINT('Ctrl Pts',(-6.76134190307601,-0.331638474897428,
5.71278617333996));
#10164=CARTESIAN_POINT('Ctrl Pts',(-6.74990195841384,-0.514459101048899,
5.72143188969656));
#10165=CARTESIAN_POINT('Ctrl Pts',(-6.73104324404487,-0.69666767313971,
5.73007760605316));
#10166=CARTESIAN_POINT('Ctrl Pts',(-6.71220874041747,-0.878642326599372,
5.73871222307391));
#10167=CARTESIAN_POINT('Ctrl Pts',(-6.68597449005211,-1.06000619092076,
5.74734684009467));
#10168=CARTESIAN_POINT('Ctrl Pts',(-6.6523921143403,-1.24014844154358,5.75598145711543));
#10169=CARTESIAN_POINT('Ctrl Pts',(-6.61762372947053,-1.42665267086645,
5.76492101786471));
#10170=CARTESIAN_POINT('Ctrl Pts',(-6.57497870581106,-1.61184710402766,
5.77386057861398));
#10171=CARTESIAN_POINT('Ctrl Pts',(-6.52457313922218,-1.79505831407797,
5.78280013936326));
#10172=CARTESIAN_POINT('Ctrl Pts',(-6.47602212139883,-1.97152871857001,
5.79141079097663));
#10173=CARTESIAN_POINT('Ctrl Pts',(-6.42027148215713,-2.14615888479742,
5.80002144258999));
#10174=CARTESIAN_POINT('Ctrl Pts',(-6.35747716681006,-2.31835568312732,
5.80863209420336));
#10175=CARTESIAN_POINT('Ctrl Pts',(-6.29474229034639,-2.49038948604338,
5.81723459527771));
#10176=CARTESIAN_POINT('Ctrl Pts',(-6.22497713471703,-2.65999422771345,
5.82583709635205));
#10177=CARTESIAN_POINT('Ctrl Pts',(-6.14838754772299,-2.8265915097525,5.8344395974264));
#10178=CARTESIAN_POINT('Ctrl Pts',(-6.07188416047097,-2.99300129054892,
5.84303241659225));
#10179=CARTESIAN_POINT('Ctrl Pts',(-5.98857179181415,-3.156410087815,5.8516252357581));
#10180=CARTESIAN_POINT('Ctrl Pts',(-5.89870460580497,-3.31625888215248,
5.86021805492395));
#10181=CARTESIAN_POINT('Ctrl Pts',(-5.88811326999088,-3.33509793048024,
5.86123076531822));
#10182=CARTESIAN_POINT('Ctrl Pts',(-5.87743094336133,-3.3538875535566,5.86224347571249));
#10183=CARTESIAN_POINT('Ctrl Pts',(-5.86665808582902,-3.37262685513488,
5.86325618610676));
#10184=CARTESIAN_POINT('Ctrl Pts',(-5.77522474126469,-3.5316744442229,5.8718514448991));
#10185=CARTESIAN_POINT('Ctrl Pts',(-5.677373755905,-3.68690796342183,5.88044670369145));
#10186=CARTESIAN_POINT('Ctrl Pts',(-5.57345574042497,-3.83782231343818,
5.88904196248379));
#10187=CARTESIAN_POINT('Ctrl Pts',(-5.46944040975675,-3.98887798888597,
5.89764527040239));
#10188=CARTESIAN_POINT('Ctrl Pts',(-5.35934688157355,-4.13560617021424,
5.90624857832099));
#10189=CARTESIAN_POINT('Ctrl Pts',(-5.24356699655792,-4.27753365300714,
5.91485188623959));
#10190=CARTESIAN_POINT('Ctrl Pts',(-5.12298685932865,-4.42534547152348,
5.92381188865547));
#10191=CARTESIAN_POINT('Ctrl Pts',(-4.99623905480765,-4.56794974683564,
5.93277189107135));
#10192=CARTESIAN_POINT('Ctrl Pts',(-4.86380883061562,-4.70485415918767,
5.94173189348723));
#10193=CARTESIAN_POINT('Ctrl Pts',(-4.73630273460883,-4.83666808045537,
5.95035873781398));
#10194=CARTESIAN_POINT('Ctrl Pts',(-4.60352942197209,-4.9631981987936,5.95898558214072));
#10195=CARTESIAN_POINT('Ctrl Pts',(-4.46595639412251,-5.08404587762505,
5.96761242646746));
#10196=CARTESIAN_POINT('Ctrl Pts',(-4.32825188099425,-5.20500905650021,
5.97624751589172));
#10197=CARTESIAN_POINT('Ctrl Pts',(-4.18573873102094,-5.32027876107326,
5.98488260531599));
#10198=CARTESIAN_POINT('Ctrl Pts',(-4.03891577337752,-5.42949798559336,
5.99351769474025));
#10199=CARTESIAN_POINT('Ctrl Pts',(-3.89187475396772,-5.53887942273608,
6.00216560901754));
#10200=CARTESIAN_POINT('Ctrl Pts',(-3.74051138500744,-5.64219224681083,
6.01081352329483));
#10201=CARTESIAN_POINT('Ctrl Pts',(-3.58535282606466,-5.73912311356275,
6.01946143757212));
#10202=CARTESIAN_POINT('Ctrl Pts',(-3.56794648950848,-5.74999722389777,
6.02043159679147));
#10203=CARTESIAN_POINT('Ctrl Pts',(-3.55049241386118,-5.7607910635445,6.02140175601082));
#10204=CARTESIAN_POINT('Ctrl Pts',(-3.53299136149909,-5.77150422676557,
6.02237191523017));
#10205=CARTESIAN_POINT('Ctrl Pts',(-3.38462340153565,-5.86232677497461,
6.03059659459439));
#10206=CARTESIAN_POINT('Ctrl Pts',(-3.23255550819682,-5.94754419851678,
6.03882127395862));
#10207=CARTESIAN_POINT('Ctrl Pts',(-3.07724947677291,-6.02684201366693,
6.04704595332284));
#10208=CARTESIAN_POINT('Ctrl Pts',(-2.92210668960703,-6.10605647781726,
6.05526198761599));
#10209=CARTESIAN_POINT('Ctrl Pts',(-2.7637328588157,-6.17936356249282,6.06347802190914));
#10210=CARTESIAN_POINT('Ctrl Pts',(-2.60261784015299,-6.24649256608198,
6.07169405620228));
#10211=CARTESIAN_POINT('Ctrl Pts',(-2.44163990002671,-6.31356445553218,
6.07990310019766));
#10212=CARTESIAN_POINT('Ctrl Pts',(-2.27792574593822,-6.37446859553087,
6.08811214419304));
#10213=CARTESIAN_POINT('Ctrl Pts',(-2.11198895129626,-6.42898060889925,
6.09632118818841));
#10214=CARTESIAN_POINT('Ctrl Pts',(-1.94616010956576,-6.48345715858059,
6.10452489165518));
#10215=CARTESIAN_POINT('Ctrl Pts',(-1.77811184683441,-6.53154975353674,
6.11272859512194));
#10216=CARTESIAN_POINT('Ctrl Pts',(-1.60837688150384,-6.57308244334757,
6.12093229858871));
#10217=CARTESIAN_POINT('Ctrl Pts',(-1.43871835834537,-6.6145964284147,6.12913230741948));
#10218=CARTESIAN_POINT('Ctrl Pts',(-1.26737499339819,-6.64955630916641,
6.13733231625025));
#10219=CARTESIAN_POINT('Ctrl Pts',(-1.09489389232812,-6.67783620378207,
6.14553232508102));
#10220=CARTESIAN_POINT('Ctrl Pts',(-0.922426583258931,-6.70611383706981,
6.15373167821949));
#10221=CARTESIAN_POINT('Ctrl Pts',(-0.748822071284916,-6.72771248159113,
6.16193103135797));
#10222=CARTESIAN_POINT('Ctrl Pts',(-0.574637238014458,-6.74255745579429,
6.17013038449645));
#10223=CARTESIAN_POINT('Ctrl Pts',(-0.400453540407016,-6.75740233321009,
6.17832968417618));
#10224=CARTESIAN_POINT('Ctrl Pts',(-0.225689886167997,-6.76549359648846,
6.18652898385591));
#10225=CARTESIAN_POINT('Ctrl Pts',(-0.0509077364817006,-6.76680850936143,
6.19472828353565));
#10226=CARTESIAN_POINT('Ctrl Pts',(0.12390498084826,-6.76812365219948,6.2029290171906));
#10227=CARTESIAN_POINT('Ctrl Pts',(0.298735841557815,-6.76266008079018,
6.21112975084555));
#10228=CARTESIAN_POINT('Ctrl Pts',(0.473023870177445,-6.7504472013521,6.2193304845005));
#10229=CARTESIAN_POINT('Ctrl Pts',(0.647373997929306,-6.73822997044351,
6.22753414009133));
#10230=CARTESIAN_POINT('Ctrl Pts',(0.821180550889936,-6.71925866608624,
6.23573779568215));
#10231=CARTESIAN_POINT('Ctrl Pts',(0.993888098807123,-6.69361452782049,
6.24394145127298));
#10232=CARTESIAN_POINT('Ctrl Pts',(1.16679349431086,-6.66794101254762,6.25215450467808));
#10233=CARTESIAN_POINT('Ctrl Pts',(1.33859701452745,-6.6355794442417,6.26036755808319));
#10234=CARTESIAN_POINT('Ctrl Pts',(1.50875278765621,-6.59666233983062,6.26858061148829));
#10235=CARTESIAN_POINT('Ctrl Pts',(1.67900924576156,-6.55772220729846,6.27679852474078));
#10236=CARTESIAN_POINT('Ctrl Pts',(1.84761566766184,-6.51221889950933,6.28501643799327));
#10237=CARTESIAN_POINT('Ctrl Pts',(2.01404186673779,-6.46033469404081,6.29323435124576));
#10238=CARTESIAN_POINT('Ctrl Pts',(2.1807276345616,-6.4083695667083,6.30146508167166));
#10239=CARTESIAN_POINT('Ctrl Pts',(2.34522604641402,-6.35000377306232,6.30969581209757));
#10240=CARTESIAN_POINT('Ctrl Pts',(2.50702614051678,-6.28546807570968,6.31792654252347));
#10241=CARTESIAN_POINT('Ctrl Pts',(2.65562021793037,-6.22619973930026,6.32548548617464));
#10242=CARTESIAN_POINT('Ctrl Pts',(2.80193853728015,-6.16172820601175,6.33304442982581));
#10243=CARTESIAN_POINT('Ctrl Pts',(2.94560484711739,-6.09226567745027,6.34060337347697));
#10244=CARTESIAN_POINT('Ctrl Pts',(3.10057882950525,-6.01733589961927,6.34875726565667));
#10245=CARTESIAN_POINT('Ctrl Pts',(3.25294572789472,-5.93636621911992,6.35691115783636));
#10246=CARTESIAN_POINT('Ctrl Pts',(3.40219555097585,-5.84956019140928,6.36506505001605));
#10247=CARTESIAN_POINT('Ctrl Pts',(3.55126324757393,-5.76286009130517,6.37320899216917));
#10248=CARTESIAN_POINT('Ctrl Pts',(3.69722112764911,-5.67033800227159,6.38135293432229));
#10249=CARTESIAN_POINT('Ctrl Pts',(3.83957962510095,-5.57224526582505,6.3894968764754));
#10250=CARTESIAN_POINT('Ctrl Pts',(3.98179436903647,-5.47425158335871,6.39763259488114));
#10251=CARTESIAN_POINT('Ctrl Pts',(4.12041666740123,-5.37069865812758,6.40576831328687));
#10252=CARTESIAN_POINT('Ctrl Pts',(4.25498201289986,-5.26188341470035,6.4139040316926));
#10253=CARTESIAN_POINT('Ctrl Pts',(4.38943978025423,-5.15315516352148,6.42203324600558));
#10254=CARTESIAN_POINT('Ctrl Pts',(4.5198467695529,-5.03917319947558,6.43016246031856));
#10255=CARTESIAN_POINT('Ctrl Pts',(4.64576792213785,-4.92027737161585,6.43829167463154));
#10256=CARTESIAN_POINT('Ctrl Pts',(4.77161488365571,-4.80145159559538,6.44641609931964));
#10257=CARTESIAN_POINT('Ctrl Pts',(4.89298100668191,-4.677717971802,6.45454052400775));
#10258=CARTESIAN_POINT('Ctrl Pts',(5.00946478225142,-4.54945618677471,6.46266494869586));
#10259=CARTESIAN_POINT('Ctrl Pts',(5.12665568860967,-4.42041577093153,6.47083869382202));
#10260=CARTESIAN_POINT('Ctrl Pts',(5.23890448375643,-4.28679227231257,6.47901243894818));
#10261=CARTESIAN_POINT('Ctrl Pts',(5.34584001264921,-4.14900994927208,6.48718618407435));
#10262=CARTESIAN_POINT('Ctrl Pts',(5.45209075797299,-4.01210994356703,6.4953075869489));
#10263=CARTESIAN_POINT('Ctrl Pts',(5.55309587850924,-3.87110452812187,6.50342898982345));
#10264=CARTESIAN_POINT('Ctrl Pts',(5.64853201215003,-3.726442688103,6.511550392698));
#10265=CARTESIAN_POINT('Ctrl Pts',(5.74397552440886,-3.58176966359435,6.51967242347655));
#10266=CARTESIAN_POINT('Ctrl Pts',(5.83384899054407,-3.43343995688232,6.5277944542551));
#10267=CARTESIAN_POINT('Ctrl Pts',(5.91787278782245,-3.28193093576793,6.53591648503365));
#10268=CARTESIAN_POINT('Ctrl Pts',(6.00191908144825,-3.13038134996012,6.54404069038692));
#10269=CARTESIAN_POINT('Ctrl Pts',(6.08011241025209,-2.97565107474226,6.5521648957402));
#10270=CARTESIAN_POINT('Ctrl Pts',(6.15221947768191,-2.81824138398956,6.56028910109348));
#10271=CARTESIAN_POINT('Ctrl Pts',(6.22510705390718,-2.65912784294172,6.56850124531267));
#10272=CARTESIAN_POINT('Ctrl Pts',(6.29177567936625,-2.49727689032067,6.57671338953187));
#10273=CARTESIAN_POINT('Ctrl Pts',(6.35203496101377,-2.33322541861237,6.58492553375106));
#10274=CARTESIAN_POINT('Ctrl Pts',(6.41174414208941,-2.17067155533774,6.59306271017927));
#10275=CARTESIAN_POINT('Ctrl Pts',(6.46516046002134,-2.00595754963186,6.60119988660748));
#10276=CARTESIAN_POINT('Ctrl Pts',(6.51214947318962,-1.83961904720411,6.60933706303569));
#10277=CARTESIAN_POINT('Ctrl Pts',(6.55978785089153,-1.67098183031588,6.61758669115038));
#10278=CARTESIAN_POINT('Ctrl Pts',(6.60081988677828,-1.50067526997758,6.62583631926506));
#10279=CARTESIAN_POINT('Ctrl Pts',(6.63515950442006,-1.32926571869741,6.63408594737974));
#10280=CARTESIAN_POINT('Ctrl Pts',(6.66949912206185,-1.15785616741723,6.64233557549442));
#10281=CARTESIAN_POINT('Ctrl Pts',(6.69714632303405,-0.985344015134451,
6.65058520360911));
#10282=CARTESIAN_POINT('Ctrl Pts',(6.71806973041192,-0.812298034789663,
6.65883483172379));
#10283=CARTESIAN_POINT('Ctrl Pts',(6.73893033832974,-0.639771434196579,
6.66705969942628));
#10284=CARTESIAN_POINT('Ctrl Pts',(6.7531699834837,-0.466198525443087,6.67528456712877));
#10285=CARTESIAN_POINT('Ctrl Pts',(6.76069152120858,-0.292128661822798,
6.68350943483126));
#10286=CARTESIAN_POINT('Ctrl Pts',(6.76820458507971,-0.118254907378856,
6.69172503630008));
#10287=CARTESIAN_POINT('Ctrl Pts',(6.76901459738444,0.0561143319093995,
6.69994063776891));
#10288=CARTESIAN_POINT('Ctrl Pts',(6.76307583088638,0.230422016483844,6.70815623923773));
#10289=CARTESIAN_POINT('Ctrl Pts',(6.75714256185588,0.404568345860861,6.71636423559149));
#10290=CARTESIAN_POINT('Ctrl Pts',(6.74447296776536,0.578652877699234,6.72457223194525));
#10291=CARTESIAN_POINT('Ctrl Pts',(6.72507328449049,0.752115894149552,6.73278022829902));
#10292=CARTESIAN_POINT('Ctrl Pts',(6.70568766281652,0.925453178252891,6.74098227519642));
#10293=CARTESIAN_POINT('Ctrl Pts',(6.67958170815466,1.09816948917078,6.74918432209383));
#10294=CARTESIAN_POINT('Ctrl Pts',(6.64681366850358,1.2697074687478,6.75738636899124));
#10295=CARTESIAN_POINT('Ctrl Pts',(6.61406280021216,1.44115555767607,6.76558411778908));
#10296=CARTESIAN_POINT('Ctrl Pts',(6.57465686895185,1.61142619381439,6.77378186658691));
#10297=CARTESIAN_POINT('Ctrl Pts',(6.52870568679892,1.77996939725364,6.78197961538475));
#10298=CARTESIAN_POINT('Ctrl Pts',(6.48276326890898,1.94848045446964,6.79017580062702));
#10299=CARTESIAN_POINT('Ctrl Pts',(6.43027817500591,2.1152643878326,6.7983719858693));
#10300=CARTESIAN_POINT('Ctrl Pts',(6.37141090777295,2.27978333275597,6.80656817111157));
#10301=CARTESIAN_POINT('Ctrl Pts',(6.31254799540589,2.44429010694374,6.81476375001879));
#10302=CARTESIAN_POINT('Ctrl Pts',(6.2473039700302,2.60653188824039,6.82295932892601));
#10303=CARTESIAN_POINT('Ctrl Pts',(6.1758885915632,2.76598790752952,6.83115490783323));
#10304=CARTESIAN_POINT('Ctrl Pts',(6.10446550306057,2.92546114176053,6.83935137153874));
#10305=CARTESIAN_POINT('Ctrl Pts',(6.02686988076987,3.08214768724175,6.84754783524426));
#10306=CARTESIAN_POINT('Ctrl Pts',(5.94335884845949,3.23554857766629,6.85574429894977));
#10307=CARTESIAN_POINT('Ctrl Pts',(5.85982360635481,3.38899393890983,6.86394313880482));
#10308=CARTESIAN_POINT('Ctrl Pts',(5.7703697099494,3.53915143274394,6.87214197865987));
#10309=CARTESIAN_POINT('Ctrl Pts',(5.67529929279949,3.68554839028735,6.88034081851492));
#10310=CARTESIAN_POINT('Ctrl Pts',(5.58012957189289,3.83209826361977,6.88854822229156));
#10311=CARTESIAN_POINT('Ctrl Pts',(5.47933180520223,3.97487945171123,6.8967556260682));
#10312=CARTESIAN_POINT('Ctrl Pts',(5.37325094832126,4.11344906937775,6.90496302984484));
#10313=CARTESIAN_POINT('Ctrl Pts',(5.26711326891827,4.25209291226628,6.91317482994137));
#10314=CARTESIAN_POINT('Ctrl Pts',(5.15568708661717,4.38652041145342,6.92138663003791));
#10315=CARTESIAN_POINT('Ctrl Pts',(5.03935632556689,4.51632337460118,6.92959843013445));
#10316=CARTESIAN_POINT('Ctrl Pts',(4.92285430938292,4.64631742584642,6.93782231914806));
#10317=CARTESIAN_POINT('Ctrl Pts',(4.80143353468832,4.77167307777975,6.94604620816167));
#10318=CARTESIAN_POINT('Ctrl Pts',(4.67551424132182,4.89201958082721,6.95427009717528));
#10319=CARTESIAN_POINT('Ctrl Pts',(4.55916699638352,5.003217664085,6.96186882810706));
#10320=CARTESIAN_POINT('Ctrl Pts',(4.43897971397702,5.11013950919111,6.96946755903884));
#10321=CARTESIAN_POINT('Ctrl Pts',(4.31530694643228,5.21252481606307,6.97706628997062));
#10322=CARTESIAN_POINT('Ctrl Pts',(4.18143145231705,5.32335668163658,6.98529189920001));
#10323=CARTESIAN_POINT('Ctrl Pts',(4.04309549009467,5.4291832258518,6.99351750842941));
#10324=CARTESIAN_POINT('Ctrl Pts',(3.90070882041701,5.52962563817126,7.0017431176588));
#10325=CARTESIAN_POINT('Ctrl Pts',(3.75850810645129,5.62993687360223,7.00995798431641));
#10326=CARTESIAN_POINT('Ctrl Pts',(3.61226751526927,5.72487778127523,7.01817285097402));
#10327=CARTESIAN_POINT('Ctrl Pts',(3.46243083959908,5.81410884667575,7.02638771763162));
#10328=CARTESIAN_POINT('Ctrl Pts',(3.3435308009667,5.88491645820261,7.03290646852209));
#10329=CARTESIAN_POINT('Ctrl Pts',(3.22236708440406,5.95212932762741,7.03942521941255));
#10330=CARTESIAN_POINT('Ctrl Pts',(3.09917575053257,6.0155962852664,7.04594397030302));
#10331=CARTESIAN_POINT('Ctrl Pts',(3.09917575053259,6.01559628526639,5.04568623149126));
#10332=CARTESIAN_POINT('Ctrl Pts',(2.96116928620942,6.08669585168754,5.05301666782408));
#10333=CARTESIAN_POINT('Ctrl Pts',(2.82086347532898,6.15296737661428,5.0603471041569));
#10334=CARTESIAN_POINT('Ctrl Pts',(2.6786296007288,6.21427650351185,5.06767754048972));
#10335=CARTESIAN_POINT('Ctrl Pts',(2.52047449629172,6.28244838868821,5.07582852369992));
#10336=CARTESIAN_POINT('Ctrl Pts',(2.35946675698987,6.34468578280044,5.08397950691011));
#10337=CARTESIAN_POINT('Ctrl Pts',(2.19609554583758,6.40073850063822,5.0921304901203));
#10338=CARTESIAN_POINT('Ctrl Pts',(2.03291410529744,6.45672610811473,5.10027200521759));
#10339=CARTESIAN_POINT('Ctrl Pts',(1.86737500017405,6.50654322228651,5.10841352031487));
#10340=CARTESIAN_POINT('Ctrl Pts',(1.69998989059556,6.54998651692299,5.11655503541215));
#10341=CARTESIAN_POINT('Ctrl Pts',(1.53276399019445,6.59338849025425,5.12468880666696));
#10342=CARTESIAN_POINT('Ctrl Pts',(1.36369593248479,6.63042862233689,5.13282257792177));
#10343=CARTESIAN_POINT('Ctrl Pts',(1.19331516365316,6.66095247845197,5.14095634917658));
#10344=CARTESIAN_POINT('Ctrl Pts',(1.02306061877344,6.69145372144133,5.14908409465302));
#10345=CARTESIAN_POINT('Ctrl Pts',(0.851495657629336,6.71544823651412,5.15721184012945));
#10346=CARTESIAN_POINT('Ctrl Pts',(0.679162619569531,6.73283202940482,5.16533958560589));
#10347=CARTESIAN_POINT('Ctrl Pts',(0.506921020068551,6.75020659859132,5.1734630185643));
#10348=CARTESIAN_POINT('Ctrl Pts',(0.333912518318684,6.76097739442739,5.18158645152271));
#10349=CARTESIAN_POINT('Ctrl Pts',(0.160687322145687,6.76509191249473,5.18970988448112));
#10350=CARTESIAN_POINT('Ctrl Pts',(-0.0136367096904394,6.76923253057113,
5.1978848475751));
#10351=CARTESIAN_POINT('Ctrl Pts',(-0.188179824193343,6.76663207214025,
5.20605981066907));
#10352=CARTESIAN_POINT('Ctrl Pts',(-0.362377918111779,6.7572902294089,5.21423477376305));
#10353=CARTESIAN_POINT('Ctrl Pts',(-0.53543870436596,6.74800937786923,5.22235636401021));
#10354=CARTESIAN_POINT('Ctrl Pts',(-0.708158593633639,6.7320749528716,5.23047795425738));
#10355=CARTESIAN_POINT('Ctrl Pts',(-0.879986681490872,6.70953891414296,
5.23859954450454));
#10356=CARTESIAN_POINT('Ctrl Pts',(-1.05183745423552,6.6869999001877,5.24672220697082));
#10357=CARTESIAN_POINT('Ctrl Pts',(-1.22279582814528,6.65785758412463,5.2548448694371));
#10358=CARTESIAN_POINT('Ctrl Pts',(-1.39231836932743,6.62221553246596,5.26296753190337));
#10359=CARTESIAN_POINT('Ctrl Pts',(-1.56189557310442,6.58656198801692,5.27109281352463));
#10360=CARTESIAN_POINT('Ctrl Pts',(-1.73003566423887,6.54440460977088,5.27921809514588));
#10361=CARTESIAN_POINT('Ctrl Pts',(-1.89620775112108,6.49589756420068,5.28734337676714));
#10362=CARTESIAN_POINT('Ctrl Pts',(-2.0641901860791,6.44686206262888,5.29555717859792));
#10363=CARTESIAN_POINT('Ctrl Pts',(-2.2301611163303,6.39133783897611,5.3037709804287));
#10364=CARTESIAN_POINT('Ctrl Pts',(-2.39359110047914,6.32953478888513,5.31198478225949));
#10365=CARTESIAN_POINT('Ctrl Pts',(-2.555539556285,6.26829199688184,5.32012412419064));
#10366=CARTESIAN_POINT('Ctrl Pts',(-2.7149926340114,6.20088394956441,5.3282634661218));
#10367=CARTESIAN_POINT('Ctrl Pts',(-2.87145868722545,6.12756183221006,5.33640280805295));
#10368=CARTESIAN_POINT('Ctrl Pts',(-3.03007180221354,6.05323357255117,5.34465383983355));
#10369=CARTESIAN_POINT('Ctrl Pts',(-3.1856149723243,5.97282793781744,5.35290487161414));
#10370=CARTESIAN_POINT('Ctrl Pts',(-3.3376055319347,5.88665255584181,5.36115590339474));
#10371=CARTESIAN_POINT('Ctrl Pts',(-3.4895960915451,5.80047717386617,5.36940693517534));
#10372=CARTESIAN_POINT('Ctrl Pts',(-3.63803374962661,5.70853230380453,5.37765796695593));
#10373=CARTESIAN_POINT('Ctrl Pts',(-3.78247011302279,5.61116822454018,5.38590899873653));
#10374=CARTESIAN_POINT('Ctrl Pts',(-3.92610605910102,5.51434370396698,5.39411430609861));
#10375=CARTESIAN_POINT('Ctrl Pts',(-4.06623930133962,5.41185376680362,5.4023196134607));
#10376=CARTESIAN_POINT('Ctrl Pts',(-4.20239125627052,5.30397932963743,5.41052492082279));
#10377=CARTESIAN_POINT('Ctrl Pts',(-4.33838048651541,5.19623382072589,5.41872042145044));
#10378=CARTESIAN_POINT('Ctrl Pts',(-4.4703976232599,5.08311684669612,5.4269159220781));
#10379=CARTESIAN_POINT('Ctrl Pts',(-4.59799152353825,4.96495346901362,5.43511142270575));
#10380=CARTESIAN_POINT('Ctrl Pts',(-4.72545897646506,4.84690719290202,5.4432988014769));
#10381=CARTESIAN_POINT('Ctrl Pts',(-4.84851165873501,4.72382471526246,5.45148618024805));
#10382=CARTESIAN_POINT('Ctrl Pts',(-4.96673006214933,4.59607239822679,5.4596735590192));
#10383=CARTESIAN_POINT('Ctrl Pts',(-5.0848554348888,4.46842061447463,5.46785449482251));
#10384=CARTESIAN_POINT('Ctrl Pts',(-5.1981538612819,4.33610657394146,5.47603543062581));
#10385=CARTESIAN_POINT('Ctrl Pts',(-5.30624135968965,4.19953469240568,5.48421636642911));
#10386=CARTESIAN_POINT('Ctrl Pts',(-5.41426585178197,4.06304242128902,5.49239253340504));
#10387=CARTESIAN_POINT('Ctrl Pts',(-5.51708524309896,3.92229753546664,5.50056870038096));
#10388=CARTESIAN_POINT('Ctrl Pts',(-5.61435462919919,3.7777388868991,5.50874486735688));
#10389=CARTESIAN_POINT('Ctrl Pts',(-5.71159650740211,3.63322111968817,5.51691872210312));
#10390=CARTESIAN_POINT('Ctrl Pts',(-5.80329130197457,3.4848920348556,5.52509257684936));
#10391=CARTESIAN_POINT('Ctrl Pts',(-5.88913627471908,3.33322110544558,5.53326643159561));
#10392=CARTESIAN_POINT('Ctrl Pts',(-5.97497064196954,3.18156891382636,5.54143927652421));
#10393=CARTESIAN_POINT('Ctrl Pts',(-6.05495644819303,3.02657601364368,5.54961212145281));
#10394=CARTESIAN_POINT('Ctrl Pts',(-6.12883595213694,2.86873820203128,5.55778496638141));
#10395=CARTESIAN_POINT('Ctrl Pts',(-6.20271998252309,2.71089072002725,5.56595831204307));
#10396=CARTESIAN_POINT('Ctrl Pts',(-6.27049681243584,2.55019830651772,5.57413165770474));
#10397=CARTESIAN_POINT('Ctrl Pts',(-6.33195605887713,2.38717855814122,5.5823050033664));
#10398=CARTESIAN_POINT('Ctrl Pts',(-6.39343042916145,2.22411869399324,5.59048036031854));
#10399=CARTESIAN_POINT('Ctrl Pts',(-6.44858399277493,2.05873069227569,5.59865571727068));
#10400=CARTESIAN_POINT('Ctrl Pts',(-6.49725561951404,1.89154921022246,5.60683107422282));
#10401=CARTESIAN_POINT('Ctrl Pts',(-6.54597272310192,1.72421152038486,5.61501406990611));
#10402=CARTESIAN_POINT('Ctrl Pts',(-6.58819569097599,1.55507734991728,5.62319706558941));
#10403=CARTESIAN_POINT('Ctrl Pts',(-6.62381390017596,1.38469434021946,5.63138006127271));
#10404=CARTESIAN_POINT('Ctrl Pts',(-6.65945008661356,1.21422533473683,5.63956718708105));
#10405=CARTESIAN_POINT('Ctrl Pts',(-6.68847480924185,1.04250658917657,5.64775431288939));
#10406=CARTESIAN_POINT('Ctrl Pts',(-6.71082913503712,0.870092707897813,
5.65594143869773));
#10407=CARTESIAN_POINT('Ctrl Pts',(-6.73321254946114,0.69745447257546,5.66413921802636));
#10408=CARTESIAN_POINT('Ctrl Pts',(-6.74890819351579,0.524119653610915,
5.67233699735498));
#10409=CARTESIAN_POINT('Ctrl Pts',(-6.75790918579735,0.350645742189842,
5.6805347766836));
#10410=CARTESIAN_POINT('Ctrl Pts',(-6.76400114372378,0.233236934732492,
5.68608311237792));
#10411=CARTESIAN_POINT('Ctrl Pts',(-6.767027561351,0.115764423594308,5.69163144807225));
#10412=CARTESIAN_POINT('Ctrl Pts',(-6.76699981083753,-0.0016000390173538,
5.69717978376658));
#10413=CARTESIAN_POINT('',(-6.76699775674603,-0.00551000855003846,5.30282021621645));
#10414=CARTESIAN_POINT('Ctrl Pts',(3.09917575053259,6.01559628526639,4.6512641878525));
#10415=CARTESIAN_POINT('Ctrl Pts',(2.94379378017301,6.09564754066526,4.65947003774372));
#10416=CARTESIAN_POINT('Ctrl Pts',(2.78537750733939,6.16963903341803,4.66767588763494));
#10417=CARTESIAN_POINT('Ctrl Pts',(2.62444459443469,6.23735357108626,4.67588173752615));
#10418=CARTESIAN_POINT('Ctrl Pts',(2.46332583431231,6.30514630629777,4.68409706362919));
#10419=CARTESIAN_POINT('Ctrl Pts',(2.29968495923358,6.36664746761495,4.69231238973223));
#10420=CARTESIAN_POINT('Ctrl Pts',(2.13405782503788,6.42168873423453,4.70052771583526));
#10421=CARTESIAN_POINT('Ctrl Pts',(1.96832706039393,6.47676443936057,4.70874818214633));
#10422=CARTESIAN_POINT('Ctrl Pts',(1.8006079028474,6.52537209375087,4.71696864845741));
#10423=CARTESIAN_POINT('Ctrl Pts',(1.63144841051177,6.56739408622923,4.72518911476848));
#10424=CARTESIAN_POINT('Ctrl Pts',(1.46203675112782,6.60947872113848,4.73342183537694));
#10425=CARTESIAN_POINT('Ctrl Pts',(1.29118081740452,6.64495800742516,4.74165455598541));
#10426=CARTESIAN_POINT('Ctrl Pts',(1.11943700963936,6.67376578712871,4.74988727659387));
#10427=CARTESIAN_POINT('Ctrl Pts',(1.00011266853046,6.693780886227,4.7556072147676));
#10428=CARTESIAN_POINT('Ctrl Pts',(0.880359858345819,6.71057659890094,4.76132715294134));
#10429=CARTESIAN_POINT('Ctrl Pts',(0.760365468820596,6.72414554823327,4.76704709111507));
#10430=CARTESIAN_POINT('Ctrl Pts',(0.589277934671798,6.74349210344675,4.77520255672892));
#10431=CARTESIAN_POINT('Ctrl Pts',(0.417172491072261,6.75633628735233,4.78335802234277));
#10432=CARTESIAN_POINT('Ctrl Pts',(0.244589315295944,6.76257828545024,4.79151348795662));
#10433=CARTESIAN_POINT('Ctrl Pts',(0.0722161943895885,6.76881268627169,
4.7996590273696));
#10434=CARTESIAN_POINT('Ctrl Pts',(-0.100633140023653,6.7684608835869,4.80780456678259));
#10435=CARTESIAN_POINT('Ctrl Pts',(-0.27341030951152,6.7614743808324,4.81595010619557));
#10436=CARTESIAN_POINT('Ctrl Pts',(-0.44601351943161,6.75449491239269,4.82408744432525));
#10437=CARTESIAN_POINT('Ctrl Pts',(-0.618544346604936,6.7408940574451,4.83222478245492));
#10438=CARTESIAN_POINT('Ctrl Pts',(-0.790451303999063,6.72067524405146,
4.8403621205846));
#10439=CARTESIAN_POINT('Ctrl Pts',(-0.962221304617605,6.70047253881035,
4.84849297576787));
#10440=CARTESIAN_POINT('Ctrl Pts',(-1.13336806379849,6.67366241576214,4.85662383095114));
#10441=CARTESIAN_POINT('Ctrl Pts',(-1.30334211510246,6.640300319338,4.86475468613441));
#10442=CARTESIAN_POINT('Ctrl Pts',(-1.47321645540309,6.60695779394885,4.87288077155593));
#10443=CARTESIAN_POINT('Ctrl Pts',(-1.64191910008596,6.56707101975891,4.88100685697745));
#10444=CARTESIAN_POINT('Ctrl Pts',(-1.80890771665984,6.52074703332437,4.88913294239897));
#10445=CARTESIAN_POINT('Ctrl Pts',(-1.97648819713343,6.47425885907975,4.89728782940413));
#10446=CARTESIAN_POINT('Ctrl Pts',(-2.1423421084596,6.42128780712883,4.90544271640928));
#10447=CARTESIAN_POINT('Ctrl Pts',(-2.30593306370863,6.36199353235252,4.91359760341444));
#10448=CARTESIAN_POINT('Ctrl Pts',(-2.46888631352175,6.302930396769,4.92172070127964));
#10449=CARTESIAN_POINT('Ctrl Pts',(-2.62959387792738,6.23759338951028,4.92984379914484));
#10450=CARTESIAN_POINT('Ctrl Pts',(-2.78754251622039,6.16618972464063,4.93796689701004));
#10451=CARTESIAN_POINT('Ctrl Pts',(-2.94550355781162,6.09478045262579,4.94609063276112));
#10452=CARTESIAN_POINT('Ctrl Pts',(-3.10070490837661,6.01730372472583,4.95421436851219));
#10453=CARTESIAN_POINT('Ctrl Pts',(-3.25265517233035,5.9340140992344,4.96233810426327));
#10454=CARTESIAN_POINT('Ctrl Pts',(-3.40464627678165,5.85070208753805,4.97046402347491));
#10455=CARTESIAN_POINT('Ctrl Pts',(-3.55338423403857,5.76157424305647,4.97858994268655));
#10456=CARTESIAN_POINT('Ctrl Pts',(-3.69840406820863,5.66693006382273,4.9867158618982));
#10457=CARTESIAN_POINT('Ctrl Pts',(-3.84435093991683,5.57168087281651,4.99489372595025));
#10458=CARTESIAN_POINT('Ctrl Pts',(-3.98653167296087,5.47084478143509,5.0030715900023));
#10459=CARTESIAN_POINT('Ctrl Pts',(-4.12450434650044,5.36476960322612,5.01124945405434));
#10460=CARTESIAN_POINT('Ctrl Pts',(-4.26181886296236,5.25920042470181,5.01938830806935));
#10461=CARTESIAN_POINT('Ctrl Pts',(-4.39496513663363,5.14844231410795,5.02752716208435));
#10462=CARTESIAN_POINT('Ctrl Pts',(-4.52354328470869,5.03287642917715,5.03566601609935));
#10463=CARTESIAN_POINT('Ctrl Pts',(-4.65304585745895,4.91647967245949,5.04386338516992));
#10464=CARTESIAN_POINT('Ctrl Pts',(-4.77791410018989,4.79520601220695,5.05206075424049));
#10465=CARTESIAN_POINT('Ctrl Pts',(-4.89777978688905,4.66947985959261,5.06025812331106));
#10466=CARTESIAN_POINT('Ctrl Pts',(-5.01764547358821,4.54375370697827,5.06845549238163));
#10467=CARTESIAN_POINT('Ctrl Pts',(-5.13250840380614,4.41357538154202,5.0766528614522));
#10468=CARTESIAN_POINT('Ctrl Pts',(-5.24204411540993,4.27939978175633,5.08485023052277));
#10469=CARTESIAN_POINT('Ctrl Pts',(-5.35181758225108,4.14493294406195,5.09306539257976));
#10470=CARTESIAN_POINT('Ctrl Pts',(-5.45657409523093,4.00604321012243,5.10128055463675));
#10471=CARTESIAN_POINT('Ctrl Pts',(-5.55593672498614,3.86314070517116,5.10949571669374));
#10472=CARTESIAN_POINT('Ctrl Pts',(-5.65514609786602,3.72045861297909,5.11769820768848));
#10473=CARTESIAN_POINT('Ctrl Pts',(-5.74897796451272,3.57377637754121,5.12590069868322));
#10474=CARTESIAN_POINT('Ctrl Pts',(-5.83709498010553,3.42353781828488,5.13410318967796));
#10475=CARTESIAN_POINT('Ctrl Pts',(-5.92513272842456,3.27343440887366,5.14229830197183));
#10476=CARTESIAN_POINT('Ctrl Pts',(-6.00746567983744,3.11978135266527,5.15049341426569));
#10477=CARTESIAN_POINT('Ctrl Pts',(-6.08379874921153,2.96305278034196,5.15868852655956));
#10478=CARTESIAN_POINT('Ctrl Pts',(-6.16007713347613,2.80643648857032,5.1668777678644));
#10479=CARTESIAN_POINT('Ctrl Pts',(-6.23036403780076,2.64674938977569,5.17506700916924));
#10480=CARTESIAN_POINT('Ctrl Pts',(-6.29440943045395,2.48449168278189,5.18325625047408));
#10481=CARTESIAN_POINT('Ctrl Pts',(-6.35842067059958,2.32232050047526,5.19144112482738));
#10482=CARTESIAN_POINT('Ctrl Pts',(-6.41619689627616,2.15758177379574,5.19962599918069));
#10483=CARTESIAN_POINT('Ctrl Pts',(-6.4675354844331,1.99079726682521,5.207810873534));
#10484=CARTESIAN_POINT('Ctrl Pts',(-6.51886159240832,1.82405330442417,5.21599375818087));
#10485=CARTESIAN_POINT('Ctrl Pts',(-6.56375306949973,1.65526489418047,5.22417664282774));
#10486=CARTESIAN_POINT('Ctrl Pts',(-6.60205654749343,1.48497082250767,5.23235952747461));
#10487=CARTESIAN_POINT('Ctrl Pts',(-6.6403536107168,1.31470527036933,5.24054104171522));
#10488=CARTESIAN_POINT('Ctrl Pts',(-6.67206479634895,1.14293491054509,5.24872255595584));
#10489=CARTESIAN_POINT('Ctrl Pts',(-6.69708747044849,0.970210499408155,
5.25690407019646));
#10490=CARTESIAN_POINT('Ctrl Pts',(-6.72211774241653,0.797433642343305,
5.26508806866674));
#10491=CARTESIAN_POINT('Ctrl Pts',(-6.74045539111042,0.623702511082844,
5.27327206713702));
#10492=CARTESIAN_POINT('Ctrl Pts',(-6.75204939536963,0.449575313477734,
5.28145606560731));
#10493=CARTESIAN_POINT('Ctrl Pts',(-6.76213802762554,0.298056888685469,
5.28857744913483));
#10494=CARTESIAN_POINT('Ctrl Pts',(-6.76712131778368,0.146238821399111,
5.29569883266236));
#10495=CARTESIAN_POINT('Ctrl Pts',(-6.76699775674649,-0.005510007984206,
5.30282021618989));
#10496=CARTESIAN_POINT('Ctrl Pts',(-6.76699775674603,-0.00551000855004313,
5.30282021621645));
#10497=CARTESIAN_POINT('Ctrl Pts',(-6.76683015283113,-0.211349129456567,
5.31247998974423));
#10498=CARTESIAN_POINT('Ctrl Pts',(-6.7572668966955,-0.416798432664565,
5.32213976327201));
#10499=CARTESIAN_POINT('Ctrl Pts',(-6.73843761571402,-0.621085742172807,
5.3317995367998));
#10500=CARTESIAN_POINT('Ctrl Pts',(-6.71949010387446,-0.826655791256934,
5.34151996497044));
#10501=CARTESIAN_POINT('Ctrl Pts',(-6.69115993265996,-1.03104915348694,
5.35124039314108));
#10502=CARTESIAN_POINT('Ctrl Pts',(-6.65362825886052,-1.23349908507983,
5.36096082131172));
#10503=CARTESIAN_POINT('Ctrl Pts',(-6.61582629362638,-1.4374069980768,5.37075125298101));
#10504=CARTESIAN_POINT('Ctrl Pts',(-6.56868987512742,-1.63934333522378,
5.3805416846503));
#10505=CARTESIAN_POINT('Ctrl Pts',(-6.51245256702596,-1.83854577376713,
5.39033211631959));
#10506=CARTESIAN_POINT('Ctrl Pts',(-6.48886102517112,-1.92211116523296,
5.39443920085654));
#10507=CARTESIAN_POINT('Ctrl Pts',(-6.4636684854269,-2.00519570320228,5.39854628539348));
#10508=CARTESIAN_POINT('Ctrl Pts',(-6.43689467054598,-2.08774423728021,
5.40265336993043));
#10509=CARTESIAN_POINT('Ctrl Pts',(-6.38326861970604,-2.25308309186314,
5.41087956874304));
#10510=CARTESIAN_POINT('Ctrl Pts',(-6.32319315124855,-2.41658554801291,
5.41910576755564));
#10511=CARTESIAN_POINT('Ctrl Pts',(-6.25681139010063,-2.57771220827832,
5.42733196636825));
#10512=CARTESIAN_POINT('Ctrl Pts',(-6.19050419513153,-2.73865787606696,
5.43554892474792));
#10513=CARTESIAN_POINT('Ctrl Pts',(-6.11790494864706,-2.8972327335221,5.4437658831276));
#10514=CARTESIAN_POINT('Ctrl Pts',(-6.03920665213129,-3.05291205455598,
5.45198284150727));
#10515=CARTESIAN_POINT('Ctrl Pts',(-5.96058096147473,-3.20844774820064,
5.46019221904531));
#10516=CARTESIAN_POINT('Ctrl Pts',(-5.87586758773257,-3.36109290751923,
5.46840159658335));
#10517=CARTESIAN_POINT('Ctrl Pts',(-5.78530779642657,-3.51034224835785,
5.47661097412138));
#10518=CARTESIAN_POINT('Ctrl Pts',(-5.69481338394813,-3.659483839976,5.48481442497307));
#10519=CARTESIAN_POINT('Ctrl Pts',(-5.59848114623985,-3.80523419087512,
5.49301787582476));
#10520=CARTESIAN_POINT('Ctrl Pts',(-5.49659853754853,-3.94711204768998,
5.50122132667646));
#10521=CARTESIAN_POINT('Ctrl Pts',(-5.39476904465944,-4.08891593745314,
5.50942050071507));
#10522=CARTESIAN_POINT('Ctrl Pts',(-5.28739515414085,-4.22685106452199,
5.51761967475368));
#10523=CARTESIAN_POINT('Ctrl Pts',(-5.17480799130005,-4.36046456850381,
5.5258188487923));
#10524=CARTESIAN_POINT('Ctrl Pts',(-5.06224201381201,-4.49405293063869,
5.53401648000498));
#10525=CARTESIAN_POINT('Ctrl Pts',(-4.9444649440962,-4.62332101150091,5.54221411121767));
#10526=CARTESIAN_POINT('Ctrl Pts',(-4.82184879385737,-4.74784827149902,
5.55041174243035));
#10527=CARTESIAN_POINT('Ctrl Pts',(-4.69924147523692,-4.8723665622281,5.55860878319593));
#10528=CARTESIAN_POINT('Ctrl Pts',(-4.57179602126017,-4.99214445594116,
5.56680582396151));
#10529=CARTESIAN_POINT('Ctrl Pts',(-4.43992193486087,-5.10679764748333,
5.57500286472709));
#10530=CARTESIAN_POINT('Ctrl Pts',(-4.3080333789626,-5.22146341901208,5.58320080488903));
#10531=CARTESIAN_POINT('Ctrl Pts',(-4.17171549328966,-5.33100313273541,
5.59139874505098));
#10532=CARTESIAN_POINT('Ctrl Pts',(-4.03141157506078,-5.43507219017981,
5.59959668521292));
#10533=CARTESIAN_POINT('Ctrl Pts',(-3.89106676225446,-5.53917158077658,
5.60779701483983));
#10534=CARTESIAN_POINT('Ctrl Pts',(-3.74673389070807,-5.63779692533518,
5.61599734446675));
#10535=CARTESIAN_POINT('Ctrl Pts',(-3.5988860268442,-5.7306464177949,5.62419767409366));
#10536=CARTESIAN_POINT('Ctrl Pts',(-3.45088406562515,-5.82359268447135,
5.63240655067604));
#10537=CARTESIAN_POINT('Ctrl Pts',(-3.29936009697943,-5.91075088099942,
5.64061542725841));
#10538=CARTESIAN_POINT('Ctrl Pts',(-3.14481350150923,-5.99186423750783,
5.64882430384079));
#10539=CARTESIAN_POINT('Ctrl Pts',(-2.99018394195464,-6.07302113748825,
5.65703758713253));
#10540=CARTESIAN_POINT('Ctrl Pts',(-2.83252884433751,-6.14812657430631,
5.66525087042427));
#10541=CARTESIAN_POINT('Ctrl Pts',(-2.67236834906832,-6.21697164276128,
5.67346415371601));
#10542=CARTESIAN_POINT('Ctrl Pts',(-2.51197355847061,-6.2859174231796,5.68168945204244));
#10543=CARTESIAN_POINT('Ctrl Pts',(-2.34906638051688,-6.3485844044854,5.68991475036888));
#10544=CARTESIAN_POINT('Ctrl Pts',(-2.18418413767397,-6.40481292878515,
5.69814004869531));
#10545=CARTESIAN_POINT('Ctrl Pts',(-2.03506743547588,-6.45566505190331,
5.70557886890958));
#10546=CARTESIAN_POINT('Ctrl Pts',(-1.88433568322539,-6.50125170540708,
5.71301768912384));
#10547=CARTESIAN_POINT('Ctrl Pts',(-1.73239321362362,-6.54149086626213,
5.72045650933811));
#10548=CARTESIAN_POINT('Ctrl Pts',(-1.56587222656749,-6.58559087859873,
5.72860906660441));
#10549=CARTESIAN_POINT('Ctrl Pts',(-1.39740575776914,-6.62339724995082,
5.73676162387072));
#10550=CARTESIAN_POINT('Ctrl Pts',(-1.22751480718071,-6.65473488563986,
5.74491418113703));
#10551=CARTESIAN_POINT('Ctrl Pts',(-1.05782067914945,-6.68603621596024,
5.75305729347903));
#10552=CARTESIAN_POINT('Ctrl Pts',(-0.886705710220385,-6.71088366286189,
5.76120040582103));
#10553=CARTESIAN_POINT('Ctrl Pts',(-0.714706210401798,-6.72915180634329,
5.76934351816303));
#10554=CARTESIAN_POINT('Ctrl Pts',(-0.542869815212691,-6.74740262640934,
5.77747890850978));
#10555=CARTESIAN_POINT('Ctrl Pts',(-0.370150920070342,-6.75908652587784,
5.78561429885652));
#10556=CARTESIAN_POINT('Ctrl Pts',(-0.197096186913418,-6.76412907129249,
5.79374968920327));
#10557=CARTESIAN_POINT('Ctrl Pts',(-0.0241691960950483,-6.76916789449434,
5.80187907431821));
#10558=CARTESIAN_POINT('Ctrl Pts',(0.149092775254158,-6.7675751145626,5.81000845943315));
#10559=CARTESIAN_POINT('Ctrl Pts',(0.322137779497406,-6.75932809168341,
5.81813784454809));
#10560=CARTESIAN_POINT('Ctrl Pts',(0.495091396288253,-6.7510854241707,5.82626293642267));
#10561=CARTESIAN_POINT('Ctrl Pts',(0.667827909838346,-6.73619552974571,
5.83438802829725));
#10562=CARTESIAN_POINT('Ctrl Pts',(0.839795209358442,-6.71468785621034,
5.84251312017184));
#10563=CARTESIAN_POINT('Ctrl Pts',(1.01241890820848,-6.69309808786662,5.85066922552909));
#10564=CARTESIAN_POINT('Ctrl Pts',(1.18426713698976,-6.66483991755443,5.85882533088633));
#10565=CARTESIAN_POINT('Ctrl Pts',(1.35478594662076,-6.62999577969993,5.86698143624358));
#10566=CARTESIAN_POINT('Ctrl Pts',(1.52461848563241,-6.59529187568895,5.87510471650964));
#10567=CARTESIAN_POINT('Ctrl Pts',(1.69313192983739,-6.55405501238566,5.8832279967757));
#10568=CARTESIAN_POINT('Ctrl Pts',(1.85978889903861,-6.50641792778582,5.89135127704177));
#10569=CARTESIAN_POINT('Ctrl Pts',(2.02646806008045,-6.45877449988937,5.89947563899401));
#10570=CARTESIAN_POINT('Ctrl Pts',(2.19128990195624,-6.40472925373183,5.90760000094626));
#10571=CARTESIAN_POINT('Ctrl Pts',(2.35373205038518,-6.34446486592759,5.9157243628985));
#10572=CARTESIAN_POINT('Ctrl Pts',(2.51622673485063,-6.2841809877872,5.92385135238172));
#10573=CARTESIAN_POINT('Ctrl Pts',(2.67633985049586,-6.21767408993008,5.93197834186494));
#10574=CARTESIAN_POINT('Ctrl Pts',(2.83356889446269,-6.14517504391319,5.94010533134816));
#10575=CARTESIAN_POINT('Ctrl Pts',(2.99181434641751,-6.0722073274291,5.94828485779796));
#10576=CARTESIAN_POINT('Ctrl Pts',(3.14713796794377,-5.99316987903029,5.95646438424776));
#10577=CARTESIAN_POINT('Ctrl Pts',(3.29905329503049,-5.90834463759084,5.96464391069756));
#10578=CARTESIAN_POINT('Ctrl Pts',(3.4502532609927,-5.82391883366219,5.97278492019617));
#10579=CARTESIAN_POINT('Ctrl Pts',(3.59807668396,-5.73375987335539,5.98092592969477));
#10580=CARTESIAN_POINT('Ctrl Pts',(3.74207405287236,-5.63818860830493,5.98906693919338));
#10581=CARTESIAN_POINT('Ctrl Pts',(3.88709334780595,-5.54193908945458,5.99726572411878));
#10582=CARTESIAN_POINT('Ctrl Pts',(4.02823177706549,-5.44020038376709,6.00546450904418));
#10583=CARTESIAN_POINT('Ctrl Pts',(4.16506530151591,-5.3333404198596,6.01366329396958));
#10584=CARTESIAN_POINT('Ctrl Pts',(4.30189882596633,-5.22648045595211,6.02186207889498));
#10585=CARTESIAN_POINT('Ctrl Pts',(4.43442720375673,-5.11449952299128,6.03006086382038));
#10586=CARTESIAN_POINT('Ctrl Pts',(4.56226549995563,-4.99780176756888,6.03825964874578));
#10587=CARTESIAN_POINT('Ctrl Pts',(4.69063807453216,-4.88061629376089,6.04649269909585));
#10588=CARTESIAN_POINT('Ctrl Pts',(4.81468041406076,-4.75831030239312,6.05472574944592));
#10589=CARTESIAN_POINT('Ctrl Pts',(4.93395882092062,-4.63123518658464,6.06295879979599));
#10590=CARTESIAN_POINT('Ctrl Pts',(5.053095185574,-4.50431139766183,6.07118204585148));
#10591=CARTESIAN_POINT('Ctrl Pts',(5.16747867139335,-4.37263005177017,6.07940529190697));
#10592=CARTESIAN_POINT('Ctrl Pts',(5.27670932851735,-4.23658207312664,6.08762853796247));
#10593=CARTESIAN_POINT('Ctrl Pts',(5.38583177150484,-4.10066887637421,6.09584363729894));
#10594=CARTESIAN_POINT('Ctrl Pts',(5.48981132951567,-3.96039793952431,6.10405873663542));
#10595=CARTESIAN_POINT('Ctrl Pts',(5.58828549491801,-3.81619630355791,6.1122738359719));
#10596=CARTESIAN_POINT('Ctrl Pts',(5.68668180526696,-3.67210867542309,6.12048244033587));
#10597=CARTESIAN_POINT('Ctrl Pts',(5.77958119151103,-3.52409683248066,6.12869104469984));
#10598=CARTESIAN_POINT('Ctrl Pts',(5.86666192876941,-3.37262017036127,6.1368996490638));
#10599=CARTESIAN_POINT('Ctrl Pts',(5.95369123735051,-3.22123296826042,6.14510340553973));
#10600=CARTESIAN_POINT('Ctrl Pts',(6.03490856471226,-3.06638533313291,6.15330716201566));
#10601=CARTESIAN_POINT('Ctrl Pts',(6.11003592269379,-2.90856494226816,6.16151091849158));
#10602=CARTESIAN_POINT('Ctrl Pts',(6.18514105240366,-2.75079124643726,6.16971224768493));
#10603=CARTESIAN_POINT('Ctrl Pts',(6.25415964474432,-2.5900468682646,6.17791357687827));
#10604=CARTESIAN_POINT('Ctrl Pts',(6.31685992330173,-2.42684356920353,6.18611490607161));
#10605=CARTESIAN_POINT('Ctrl Pts',(6.37955155490192,-2.26366277741001,6.19431510422464));
#10606=CARTESIAN_POINT('Ctrl Pts',(6.43592647895956,-2.09802407416045,6.20251530237767));
#10607=CARTESIAN_POINT('Ctrl Pts',(6.48580128391907,-1.93045867749449,6.2107155005307));
#10608=CARTESIAN_POINT('Ctrl Pts',(6.53567824900255,-1.76288602341608,6.2189160538419));
#10609=CARTESIAN_POINT('Ctrl Pts',(6.5790544318461,-1.59338685307305,6.22711660715311));
#10610=CARTESIAN_POINT('Ctrl Pts',(6.61579645043946,-1.42250705669696,6.23531716046431));
#10611=CARTESIAN_POINT('Ctrl Pts',(6.65254671873605,-1.25158889259744,6.24351955504972));
#10612=CARTESIAN_POINT('Ctrl Pts',(6.68265978067487,-1.0792898352538,6.25172194963513));
#10613=CARTESIAN_POINT('Ctrl Pts',(6.7060534630617,-0.906165520508382,6.25992434422054));
#10614=CARTESIAN_POINT('Ctrl Pts',(6.72946902265369,-0.732879304096949,
6.2681344094867));
#10615=CARTESIAN_POINT('Ctrl Pts',(6.74615260014355,-0.558766643887226,
6.27634447475286));
#10616=CARTESIAN_POINT('Ctrl Pts',(6.75607387881625,-0.384388792730363,
6.28455454001902));
#10617=CARTESIAN_POINT('Ctrl Pts',(6.76599990563727,-0.209927487421393,
6.29276853447705));
#10618=CARTESIAN_POINT('Ctrl Pts',(6.76915717448567,-0.0352010961438072,
6.30098252893508));
#10619=CARTESIAN_POINT('Ctrl Pts',(6.76556753754379,0.139229648185006,6.30919652339312));
#10620=CARTESIAN_POINT('Ctrl Pts',(6.76197300673196,0.313898199676781,6.31742171625958));
#10621=CARTESIAN_POINT('Ctrl Pts',(6.75161320850349,0.48826994093554,6.32564690912605));
#10622=CARTESIAN_POINT('Ctrl Pts',(6.734561969058,0.661788550004968,6.33387210199252));
#10623=CARTESIAN_POINT('Ctrl Pts',(6.7192278320421,0.81783340145307,6.3412689973795));
#10624=CARTESIAN_POINT('Ctrl Pts',(6.69848280746823,0.973188206981381,6.34866589276647));
#10625=CARTESIAN_POINT('Ctrl Pts',(6.67241566428336,1.12745651935055,6.35606278815344));
#10626=CARTESIAN_POINT('Ctrl Pts',(6.64194671870187,1.30777519797171,6.36470875297664));
#10627=CARTESIAN_POINT('Ctrl Pts',(6.60413684375698,1.48701865212884,6.37335471779985));
#10628=CARTESIAN_POINT('Ctrl Pts',(6.55907461042364,1.66458080455592,6.38200068262305));
#10629=CARTESIAN_POINT('Ctrl Pts',(6.51407001780353,1.84191583088753,6.39063558808362));
#10630=CARTESIAN_POINT('Ctrl Pts',(6.4618316398377,2.01757354977261,6.3992704935442));
#10631=CARTESIAN_POINT('Ctrl Pts',(6.40249921940896,2.19095703870881,6.40790539900478));
#10632=CARTESIAN_POINT('Ctrl Pts',(6.34119699297558,2.37009677077723,6.41682697890915));
#10633=CARTESIAN_POINT('Ctrl Pts',(6.27232161673629,2.54680835028713,6.42574855881353));
#10634=CARTESIAN_POINT('Ctrl Pts',(6.19608434960343,2.72044623777047,6.4346701387179));
#10635=CARTESIAN_POINT('Ctrl Pts',(6.12250058011828,2.88804052291443,6.44328119606316));
#10636=CARTESIAN_POINT('Ctrl Pts',(6.04205885699316,3.0527711420892,6.45189225340842));
#10637=CARTESIAN_POINT('Ctrl Pts',(5.95499947385894,3.21407378047546,6.46050331075368));
#10638=CARTESIAN_POINT('Ctrl Pts',(5.86802219155686,3.37522430337039,6.46910624749265));
#10639=CARTESIAN_POINT('Ctrl Pts',(5.7744398360222,3.53295302322623,6.47770918423163));
#10640=CARTESIAN_POINT('Ctrl Pts',(5.67453994056898,3.68671743735364,6.4863121209706));
#10641=CARTESIAN_POINT('Ctrl Pts',(5.57475190951144,3.84030967148841,6.49490542444305));
#10642=CARTESIAN_POINT('Ctrl Pts',(5.46866061707592,3.989946200575,6.50349872791549));
#10643=CARTESIAN_POINT('Ctrl Pts',(5.3565985952027,4.13511069862373,6.51209203138793));
#10644=CARTESIAN_POINT('Ctrl Pts',(5.34411295400281,4.15128452636039,6.51304947354438));
#10645=CARTESIAN_POINT('Ctrl Pts',(5.33155323905529,4.16740286656107,6.51400691570084));
#10646=CARTESIAN_POINT('Ctrl Pts',(5.31891994443521,4.18346502611046,6.51496435785729));
#10647=CARTESIAN_POINT('Ctrl Pts',(5.20551707715331,4.32764712606281,6.52355884481129));
#10648=CARTESIAN_POINT('Ctrl Pts',(5.08631475608562,4.46713086329329,6.53215333176528));
#10649=CARTESIAN_POINT('Ctrl Pts',(4.96173253515189,4.6014670757939,6.54074781871927));
#10650=CARTESIAN_POINT('Ctrl Pts',(4.83703437850644,4.73592830103138,6.54935030366812));
#10651=CARTESIAN_POINT('Ctrl Pts',(4.70694653633858,4.8652322163818,6.55795278861697));
#10652=CARTESIAN_POINT('Ctrl Pts',(4.57192474548497,4.98896713976172,6.56655527356581));
#10653=CARTESIAN_POINT('Ctrl Pts',(4.43668617461203,5.11290072188339,6.5751715699657));
#10654=CARTESIAN_POINT('Ctrl Pts',(4.29649804557332,5.23124723238171,6.58378786636558));
#10655=CARTESIAN_POINT('Ctrl Pts',(4.15184981072849,5.34363473201096,6.59240416276547));
#10656=CARTESIAN_POINT('Ctrl Pts',(4.00707356132342,5.45612169525521,6.60102808463963));
#10657=CARTESIAN_POINT('Ctrl Pts',(3.85782957356289,5.56263894109501,6.6096520065138));
#10658=CARTESIAN_POINT('Ctrl Pts',(3.7046362967204,5.66285783937949,6.61827592838796));
#10659=CARTESIAN_POINT('Ctrl Pts',(3.55121921613449,5.76322314986338,6.62691244915705));
#10660=CARTESIAN_POINT('Ctrl Pts',(3.39384157512814,5.85727156267731,6.63554896992614));
#10661=CARTESIAN_POINT('Ctrl Pts',(3.23304779615372,5.94471958529463,6.64418549069524));
#10662=CARTESIAN_POINT('Ctrl Pts',(3.18867984950435,5.96884918301181,6.64656857227441));
#10663=CARTESIAN_POINT('Ctrl Pts',(3.14405193078544,5.99247652073751,6.64895165385358));
#10664=CARTESIAN_POINT('Ctrl Pts',(3.0991757505326,6.01559628526638,6.65133473543275));
#10665=CARTESIAN_POINT('Origin',(0.,0.,-3.69717978381041));
#10666=CARTESIAN_POINT('',(3.09917575053258,6.01559628526639,9.04575158274221));
#10667=CARTESIAN_POINT('',(3.09917575053261,6.01559628526638,8.65154848238438));
#10668=CARTESIAN_POINT('',(3.09917575053259,6.01559628526639,-3.69717978381041));
#10669=CARTESIAN_POINT('',(-6.767,1.71993712674845E-12,7.69717978381002));
#10670=CARTESIAN_POINT('Ctrl Pts',(-6.767,1.71993607050078E-12,7.69717978381002));
#10671=CARTESIAN_POINT('Ctrl Pts',(-6.76700000000005,-0.186007249414041,
7.70592929561598));
#10672=CARTESIAN_POINT('Ctrl Pts',(-6.75932637295447,-0.37201435552598,
7.71467880742193));
#10673=CARTESIAN_POINT('Ctrl Pts',(-6.7440051826694,-0.557389537153581,
7.72342831922788));
#10674=CARTESIAN_POINT('Ctrl Pts',(-6.7286840570966,-0.742763935810137,
7.73217779407844));
#10675=CARTESIAN_POINT('Ctrl Pts',(-6.70571545653006,-0.927506129693983,
7.74092726892899));
#10676=CARTESIAN_POINT('Ctrl Pts',(-6.67517739415664,-1.11098863924891,
7.74967674377954));
#10677=CARTESIAN_POINT('Ctrl Pts',(-6.64463945823084,-1.29447038906586,
7.75842618240152));
#10678=CARTESIAN_POINT('Ctrl Pts',(-6.60653217027137,-1.47669218228306,
7.76717562102351));
#10679=CARTESIAN_POINT('Ctrl Pts',(-6.56098496116688,-1.65703510504215,
7.77592505964549));
#10680=CARTESIAN_POINT('Ctrl Pts',(-6.51543793687484,-1.83737729604139,
7.78467446276574));
#10681=CARTESIAN_POINT('Ctrl Pts',(-6.46245112202596,-2.01584035397194,
7.79342386588598));
#10682=CARTESIAN_POINT('Ctrl Pts',(-6.40220448416187,-2.19181813638306,
7.80217326900622));
#10683=CARTESIAN_POINT('Ctrl Pts',(-6.34195808575123,-2.36779521936116,
7.8109226373515));
#10684=CARTESIAN_POINT('Ctrl Pts',(-6.27445201489161,-2.54128677545009,
7.81967200569678));
#10685=CARTESIAN_POINT('Ctrl Pts',(-6.199915551361,-2.71170355238031,7.82842137404205));
#10686=CARTESIAN_POINT('Ctrl Pts',(-6.12537937788953,-2.88211966613253,
7.83717070833911));
#10687=CARTESIAN_POINT('Ctrl Pts',(-6.0438129813353,-3.04946076210617,7.84592004263616));
#10688=CARTESIAN_POINT('Ctrl Pts',(-5.95549339426218,-3.21315848207018,
7.85466937693321));
#10689=CARTESIAN_POINT('Ctrl Pts',(-5.86717414355068,-3.37685557859797,
7.86341867790878));
#10690=CARTESIAN_POINT('Ctrl Pts',(-5.77210188986141,-3.5369090746747,7.87216797888434));
#10691=CARTESIAN_POINT('Ctrl Pts',(-5.67059953466966,-3.69277536785061,
7.8809172798599));
#10692=CARTESIAN_POINT('Ctrl Pts',(-5.56909755761657,-3.8486410803595,7.88966654824066));
#10693=CARTESIAN_POINT('Ctrl Pts',(-5.46116568337954,-4.00031938104437,
7.89841581662143));
#10694=CARTESIAN_POINT('Ctrl Pts',(-5.34717048685992,-4.14729511663377,
7.90716508500219));
#10695=CARTESIAN_POINT('Ctrl Pts',(-5.23317570555387,-4.294270316882,7.91591432151482));
#10696=CARTESIAN_POINT('Ctrl Pts',(-5.11311782178666,-4.4365427598729,7.92466355802744));
#10697=CARTESIAN_POINT('Ctrl Pts',(-4.98740459171866,-4.57362924147811,
7.93341279454006));
#10698=CARTESIAN_POINT('Ctrl Pts',(-4.86169180910669,-4.71071523514602,
7.94216199991119));
#10699=CARTESIAN_POINT('Ctrl Pts',(-4.73032391415257,-4.84261509316694,
7.95091120528231));
#10700=CARTESIAN_POINT('Ctrl Pts',(-4.59374707237105,-4.96888084331697,
7.95966041065343));
#10701=CARTESIAN_POINT('Ctrl Pts',(-4.45717070537202,-5.095146154529,7.96840958560966));
#10702=CARTESIAN_POINT('Ctrl Pts',(-4.31538563819296,-5.21577720253809,
7.9771587605659));
#10703=CARTESIAN_POINT('Ctrl Pts',(-4.16887341290422,-5.33036429028827,
7.98590793552213));
#10704=CARTESIAN_POINT('Ctrl Pts',(-4.02236168477122,-5.44495098921336,
7.99465708079004));
#10705=CARTESIAN_POINT('Ctrl Pts',(-3.87112305634232,-5.55349359238902,
8.00340622605795));
#10706=CARTESIAN_POINT('Ctrl Pts',(-3.71567117316537,-5.65562346102602,
8.01215537132586));
#10707=CARTESIAN_POINT('Ctrl Pts',(-3.5602198045709,-5.757752991589,8.02090448763203));
#10708=CARTESIAN_POINT('Ctrl Pts',(-3.40055544862162,-5.85346967275485,
8.0296536039382));
#10709=CARTESIAN_POINT('Ctrl Pts',(-3.23722036323162,-5.94244842803693,
8.03840272024437));
#10710=CARTESIAN_POINT('Ctrl Pts',(-3.07388580495802,-6.031426896166,8.04715180831531));
#10711=CARTESIAN_POINT('Ctrl Pts',(-2.90688079257459,-6.1136673448494,8.05590089638626));
#10712=CARTESIAN_POINT('Ctrl Pts',(-2.73677251094364,-6.18889046787413,
8.0646499844572));
#10713=CARTESIAN_POINT('Ctrl Pts',(-2.56666476416375,-6.26411335438381,
8.07339904501944));
#10714=CARTESIAN_POINT('Ctrl Pts',(-2.39345402971805,-6.332318843504,8.08214810558168));
#10715=CARTESIAN_POINT('Ctrl Pts',(-2.21772856473731,-6.3932752962115,8.09089716614392));
#10716=CARTESIAN_POINT('Ctrl Pts',(-2.04200363767987,-6.4542315623217,8.09964619992391));
#10717=CARTESIAN_POINT('Ctrl Pts',(-1.86376426619836,-6.50793874252129,
8.10839523370389));
#10718=CARTESIAN_POINT('Ctrl Pts',(-1.68361578194457,-6.55421443796182,
8.11714426748388));
#10719=CARTESIAN_POINT('Ctrl Pts',(-1.50346783419658,-6.60048999558727,
8.1258932752081));
#10720=CARTESIAN_POINT('Ctrl Pts',(-1.32141106257057,-6.63933404145532,
8.13464228293232));
#10721=CARTESIAN_POINT('Ctrl Pts',(-1.13806375958877,-6.67061465527058,
8.14339129065653));
#10722=CARTESIAN_POINT('Ctrl Pts',(-0.954716987417111,-6.70189517852511,
8.15214027305143));
#10723=CARTESIAN_POINT('Ctrl Pts',(-0.77007997380747,-6.72561226535856,
8.16088925544634));
#10724=CARTESIAN_POINT('Ctrl Pts',(-0.584779770549684,-6.74168536939806,
8.16963823784124));
#10725=CARTESIAN_POINT('Ctrl Pts',(-0.391490647551172,-6.7584514394241,
8.17876441851729));
#10726=CARTESIAN_POINT('Ctrl Pts',(-0.197480213101632,-6.76689975924034,
8.18789059919334));
#10727=CARTESIAN_POINT('Ctrl Pts',(-0.00346532629513419,-6.76699911271708,
8.19701677986939));
#10728=CARTESIAN_POINT('Ctrl Pts',(0.184486595298659,-6.76709536139766,
8.20585776739931));
#10729=CARTESIAN_POINT('Ctrl Pts',(0.37244237818777,-6.75935659726756,8.21469875492924));
#10730=CARTESIAN_POINT('Ctrl Pts',(0.559750217724562,-6.74380965728996,
8.22353974245916));
#10731=CARTESIAN_POINT('Ctrl Pts',(0.745129914460219,-6.72842275717226,
8.23228972105693));
#10732=CARTESIAN_POINT('Ctrl Pts',(0.929874656316636,-6.70538772273439,
8.2410396996547));
#10733=CARTESIAN_POINT('Ctrl Pts',(1.11335688290021,-6.67478280180702,8.24978967825247));
#10734=CARTESIAN_POINT('Ctrl Pts',(1.29683723119098,-6.64417819417976,8.25853956727741));
#10735=CARTESIAN_POINT('Ctrl Pts',(1.47905480730475,-6.60600390230022,8.26728945630235));
#10736=CARTESIAN_POINT('Ctrl Pts',(1.65939064805045,-6.56038959797074,8.27603934532729));
#10737=CARTESIAN_POINT('Ctrl Pts',(1.83972470264504,-6.51477574543189,8.28478914768824));
#10738=CARTESIAN_POINT('Ctrl Pts',(2.01817678126087,-6.46172209820025,8.29353895004919));
#10739=CARTESIAN_POINT('Ctrl Pts',(2.1941407234792,-6.40140886723932,8.30228875241014));
#10740=CARTESIAN_POINT('Ctrl Pts',(2.37010298132331,-6.34109621361287,8.31103847101562));
#10741=CARTESIAN_POINT('Ctrl Pts',(2.54357687927141,-6.27352420825878,8.31978818962111));
#10742=CARTESIAN_POINT('Ctrl Pts',(2.71397317790192,-6.198922373254,8.3285379082266));
#10743=CARTESIAN_POINT('Ctrl Pts',(2.88436790207417,-6.12432122756862,8.33728754598486));
#10744=CARTESIAN_POINT('Ctrl Pts',(3.05168482126466,-6.04269049717311,8.34603718374313));
#10745=CARTESIAN_POINT('Ctrl Pts',(3.21535561997593,-5.95430745234819,8.35478682150139));
#10746=CARTESIAN_POINT('Ctrl Pts',(3.37902496075477,-5.86592519481403,8.3635363813204));
#10747=CARTESIAN_POINT('Ctrl Pts',(3.53904799385064,-5.77079087940116,8.37228594113941));
#10748=CARTESIAN_POINT('Ctrl Pts',(3.69488118815166,-5.66922763746906,8.38103550095842));
#10749=CARTESIAN_POINT('Ctrl Pts',(3.85071304611015,-5.56766526648926,8.38978498574586));
#10750=CARTESIAN_POINT('Ctrl Pts',(4.00235489706149,-5.45967423580581,8.3985344705333));
#10751=CARTESIAN_POINT('Ctrl Pts',(4.14929168607834,-5.34562133936189,8.40728395532074));
#10752=CARTESIAN_POINT('Ctrl Pts',(4.29622726385922,-5.23156938308395,8.41603336798403));
#10753=CARTESIAN_POINT('Ctrl Pts',(4.43845763092217,-5.11145583677071,8.42478278064733));
#10754=CARTESIAN_POINT('Ctrl Pts',(4.57549970661098,-4.98568866204087,8.43353219331062));
#10755=CARTESIAN_POINT('Ctrl Pts',(4.71254069815435,-4.85992248226026,8.44228153675695));
#10756=CARTESIAN_POINT('Ctrl Pts',(4.84439326931456,-4.72850295733857,8.45103088020328));
#10757=CARTESIAN_POINT('Ctrl Pts',(4.97060959434843,-4.59187644221525,8.45978022364961));
#10758=CARTESIAN_POINT('Ctrl Pts',(5.09682496280651,-4.45525096256508,8.4685295007859));
#10759=CARTESIAN_POINT('Ctrl Pts',(5.21740397615967,-4.31341878218171,8.4772787779222));
#10760=CARTESIAN_POINT('Ctrl Pts',(5.33193710452054,-4.16686161438524,8.48602805505849));
#10761=CARTESIAN_POINT('Ctrl Pts',(5.44646940289505,-4.02030550864349,8.49477726879145));
#10762=CARTESIAN_POINT('Ctrl Pts',(5.55495572749788,-3.86902470979958,8.50352648252442));
#10763=CARTESIAN_POINT('Ctrl Pts',(5.65702762491579,-3.71353301465594,8.51227569625739));
#10764=CARTESIAN_POINT('Ctrl Pts',(5.75909881655262,-3.55804239466717,8.5210248494935));
#10765=CARTESIAN_POINT('Ctrl Pts',(5.85475551250876,-3.3983411761939,8.5297740027296));
#10766=CARTESIAN_POINT('Ctrl Pts',(5.94367283728176,-3.2349717469182,8.53852315596571));
#10767=CARTESIAN_POINT('Ctrl Pts',(6.03258957676395,-3.07160339300803,8.54727225161125));
#10768=CARTESIAN_POINT('Ctrl Pts',(6.11476689685369,-2.90456712829327,8.55602134725679));
#10769=CARTESIAN_POINT('Ctrl Pts',(6.18992570525345,-2.73443024475713,8.56477044290233));
#10770=CARTESIAN_POINT('Ctrl Pts',(6.26508404388786,-2.56429442462816,8.57351948386337));
#10771=CARTESIAN_POINT('Ctrl Pts',(6.33322384283405,-2.39105828655755,8.5822685248244));
#10772=CARTESIAN_POINT('Ctrl Pts',(6.39411368720123,-2.2153101713182,8.59101756578544));
#10773=CARTESIAN_POINT('Ctrl Pts',(6.4550031712098,-2.03956309619233,8.59976655496786));
#10774=CARTESIAN_POINT('Ctrl Pts',(6.50864269270161,-1.86130434438329,8.60851554415027));
#10775=CARTESIAN_POINT('Ctrl Pts',(6.55485008446417,-1.68113930719619,8.61726453333269));
#10776=CARTESIAN_POINT('Ctrl Pts',(6.60199664749477,-1.49731239211518,8.62619134686205));
#10777=CARTESIAN_POINT('Ctrl Pts',(6.64140563640969,-1.31150116499353,8.63511816039141));
#10778=CARTESIAN_POINT('Ctrl Pts',(6.67293772282225,-1.12436255155346,8.64404497392078));
#10779=CARTESIAN_POINT('Ctrl Pts',(6.70384494949915,-0.940932395048195,
8.65279488807631));
#10780=CARTESIAN_POINT('Ctrl Pts',(6.72718449348966,-0.756227260503556,
8.66154480223183));
#10781=CARTESIAN_POINT('Ctrl Pts',(6.74287707373959,-0.570874564538526,
8.67029471638736));
#10782=CARTESIAN_POINT('Ctrl Pts',(6.75856934538688,-0.385525513629339,
8.67904445847133));
#10783=CARTESIAN_POINT('Ctrl Pts',(6.76661493004112,-0.199529212415126,
8.68779420055531));
#10784=CARTESIAN_POINT('Ctrl Pts',(6.76698649908907,-0.0135174385973606,
8.69654394263929));
#10785=CARTESIAN_POINT('Ctrl Pts',(6.76735806132382,0.172490924448839,8.70529352428518));
#10786=CARTESIAN_POINT('Ctrl Pts',(6.76005588896273,0.358514472904459,8.71404310593108));
#10787=CARTESIAN_POINT('Ctrl Pts',(6.7451047845456,0.543921359665251,8.72279268757698));
#10788=CARTESIAN_POINT('Ctrl Pts',(6.73015393440655,0.729325093153482,8.73154212041602));
#10789=CARTESIAN_POINT('Ctrl Pts',(6.70755443556856,0.914111900259384,8.74029155325507));
#10790=CARTESIAN_POINT('Ctrl Pts',(6.67738304682269,1.0976541559184,8.74904098609411));
#10791=CARTESIAN_POINT('Ctrl Pts',(6.64721213111802,1.28119353391578,8.75779028175544));
#10792=CARTESIAN_POINT('Ctrl Pts',(6.60946960955426,1.46348811672961,8.76653957741676));
#10793=CARTESIAN_POINT('Ctrl Pts',(6.56428366991105,1.64391876348532,8.77528887307809));
#10794=CARTESIAN_POINT('Ctrl Pts',(6.51909837867631,1.82434682110027,8.78403804318892));
#10795=CARTESIAN_POINT('Ctrl Pts',(6.46646995271825,2.00291071820757,8.79278721329975));
#10796=CARTESIAN_POINT('Ctrl Pts',(6.40657713281443,2.17900400213016,8.80153638341057));
#10797=CARTESIAN_POINT('Ctrl Pts',(6.34668509278943,2.35509499309974,8.81028543959635));
#10798=CARTESIAN_POINT('Ctrl Pts',(6.27952894037398,2.52871516398441,8.81903449578213));
#10799=CARTESIAN_POINT('Ctrl Pts',(6.20533675061307,2.69927486771741,8.82778355196791));
#10800=CARTESIAN_POINT('Ctrl Pts',(6.12832117907775,2.87632521636224,8.83686555325017));
#10801=CARTESIAN_POINT('Ctrl Pts',(6.04372366625938,3.05007728920277,8.84594755453243));
#10802=CARTESIAN_POINT('Ctrl Pts',(5.95185378007727,3.21989527478455,8.8550295558147));
#10803=CARTESIAN_POINT('Ctrl Pts',(5.86334450817224,3.38350129287006,8.86377933612182));
#10804=CARTESIAN_POINT('Ctrl Pts',(5.76808562057103,3.5434556712521,8.87252911642894));
#10805=CARTESIAN_POINT('Ctrl Pts',(5.66640068804326,3.69921508465552,8.88127889673606));
#10806=CARTESIAN_POINT('Ctrl Pts',(5.56471941107758,3.85496889852522,8.89002836248954));
#10807=CARTESIAN_POINT('Ctrl Pts',(5.45661270814941,4.00652780919872,8.89877782824303));
#10808=CARTESIAN_POINT('Ctrl Pts',(5.34244776448935,4.1533770456946,8.90752729399651));
#10809=CARTESIAN_POINT('Ctrl Pts',(5.22828631819409,4.30022178356475,8.91627649171611));
#10810=CARTESIAN_POINT('Ctrl Pts',(5.10806717843877,4.442356909729,8.92502568943571));
#10811=CARTESIAN_POINT('Ctrl Pts',(4.98219864544521,4.5792996907086,8.9337748871553));
#10812=CARTESIAN_POINT('Ctrl Pts',(4.85633329943815,4.71623900430217,8.94252386334555));
#10813=CARTESIAN_POINT('Ctrl Pts',(4.72481904033426,4.84798602483834,8.95127283953579));
#10814=CARTESIAN_POINT('Ctrl Pts',(4.58810250736964,4.97409332259342,8.96002181572603));
#10815=CARTESIAN_POINT('Ctrl Pts',(4.451377086854,5.10020881822347,8.9687713606622));
#10816=CARTESIAN_POINT('Ctrl Pts',(4.30944892635802,5.22068366308139,8.97752090559838));
#10817=CARTESIAN_POINT('Ctrl Pts',(4.16280009466404,5.33510865605051,8.98627045053456));
#10818=CARTESIAN_POINT('Ctrl Pts',(4.01615988348527,5.44952692273084,8.99501948114284));
#10819=CARTESIAN_POINT('Ctrl Pts',(3.86479978231965,5.55789587288811,9.00376851175112));
#10820=CARTESIAN_POINT('Ctrl Pts',(3.70923383580798,5.65984746714055,9.0125175423594));
#10821=CARTESIAN_POINT('Ctrl Pts',(3.55366577799268,5.76180044505551,9.02126669170742));
#10822=CARTESIAN_POINT('Ctrl Pts',(3.39389200026565,5.85733573571219,9.03001584105543));
#10823=CARTESIAN_POINT('Ctrl Pts',(3.23045513625763,5.94612887622079,9.03876499040345));
#10824=CARTESIAN_POINT('Ctrl Pts',(3.18695122151392,5.96976399206787,9.04109385451637));
#10825=CARTESIAN_POINT('Ctrl Pts',(3.1431879126257,5.99292165435381,9.04342271862929));
#10826=CARTESIAN_POINT('Ctrl Pts',(3.09917575053258,6.01559628526639,9.04575158274221));
#10827=CARTESIAN_POINT('Ctrl Pts',(3.09917575053257,6.0155962852664,7.04594397030302));
#10828=CARTESIAN_POINT('Ctrl Pts',(2.94415309791935,6.09546242371369,7.05414709647275));
#10829=CARTESIAN_POINT('Ctrl Pts',(2.78591898524294,6.16939525231196,7.06235022264247));
#10830=CARTESIAN_POINT('Ctrl Pts',(2.62496877406909,6.23713299001731,7.0705533488122));
#10831=CARTESIAN_POINT('Ctrl Pts',(2.46410949560556,6.30483245765121,7.07875184042761));
#10832=CARTESIAN_POINT('Ctrl Pts',(2.30053750533951,6.36634366800712,7.08695033204302));
#10833=CARTESIAN_POINT('Ctrl Pts',(2.13477077043363,6.42145176402519,7.09514882365843));
#10834=CARTESIAN_POINT('Ctrl Pts',(1.96615218344512,6.47750794011788,7.10348836218172));
#10835=CARTESIAN_POINT('Ctrl Pts',(1.79526298420467,6.52693850177259,7.11182790070501));
#10836=CARTESIAN_POINT('Ctrl Pts',(1.6226680115254,6.56956905164808,7.12016743922831));
#10837=CARTESIAN_POINT('Ctrl Pts',(1.45305240438134,6.61146370528584,7.12836301913409));
#10838=CARTESIAN_POINT('Ctrl Pts',(1.28178980116446,6.64679113915501,7.13655859903987));
#10839=CARTESIAN_POINT('Ctrl Pts',(1.10942978191014,6.67543665680462,7.14475417894565));
#10840=CARTESIAN_POINT('Ctrl Pts',(0.937056999630132,6.70408429561597,7.15295036572302));
#10841=CARTESIAN_POINT('Ctrl Pts',(0.763586993430932,6.72604897339413,7.16114655250038));
#10842=CARTESIAN_POINT('Ctrl Pts',(0.589577551380603,6.74126748548877,7.16934273927774));
#10843=CARTESIAN_POINT('Ctrl Pts',(0.415523565114005,6.75648989333002,7.17754102417525));
#10844=CARTESIAN_POINT('Ctrl Pts',(0.240930225363941,6.76496266437051,7.18573930907276));
#10845=CARTESIAN_POINT('Ctrl Pts',(0.0663584836826785,6.76667463024811,
7.19393759397027));
#10846=CARTESIAN_POINT('Ctrl Pts',(-0.113502496237864,6.76843846589167,
7.20238427349086));
#10847=CARTESIAN_POINT('Ctrl Pts',(-0.293340137794372,6.76302535317051,
7.21083095301146));
#10848=CARTESIAN_POINT('Ctrl Pts',(-0.472543928585516,6.7504808151388,7.21927763253206));
#10849=CARTESIAN_POINT('Ctrl Pts',(-0.646748104996574,6.7382862577211,7.22748865777208));
#10850=CARTESIAN_POINT('Ctrl Pts',(-0.820352974813139,6.71935296395488,
7.2356996830121));
#10851=CARTESIAN_POINT('Ctrl Pts',(-0.992805957653864,6.6937751180068,7.24391070825212));
#10852=CARTESIAN_POINT('Ctrl Pts',(-1.17268297386735,6.66709615580783,7.252475214913));
#10853=CARTESIAN_POINT('Ctrl Pts',(-1.3513062867024,6.63318795858461,7.26103972157388));
#10854=CARTESIAN_POINT('Ctrl Pts',(-1.52806445370092,6.59221571441164,7.26960422823477));
#10855=CARTESIAN_POINT('Ctrl Pts',(-1.70482262069945,6.55124347023866,7.27816873489565));
#10856=CARTESIAN_POINT('Ctrl Pts',(-1.87971523837467,6.50320735711522,7.28673324155653));
#10857=CARTESIAN_POINT('Ctrl Pts',(-2.05215294173931,6.44832980729977,7.29529774821742));
#10858=CARTESIAN_POINT('Ctrl Pts',(-2.21626474669054,6.3961019384765,7.30344873039364));
#10859=CARTESIAN_POINT('Ctrl Pts',(-2.378639230899,6.3375228963036,7.31159971256987));
#10860=CARTESIAN_POINT('Ctrl Pts',(-2.53874301684855,6.27272451925021,7.31975069474609));
#10861=CARTESIAN_POINT('Ctrl Pts',(-2.69866082741191,6.20800141151743,7.32789220880107));
#10862=CARTESIAN_POINT('Ctrl Pts',(-2.85631285459867,6.13707348528331,7.33603372285604));
#10863=CARTESIAN_POINT('Ctrl Pts',(-3.01117945953484,6.06012271018298,7.34417523691102));
#10864=CARTESIAN_POINT('Ctrl Pts',(-3.16589876216972,5.98324512727449,7.35230900711601));
#10865=CARTESIAN_POINT('Ctrl Pts',(-3.31783759181699,5.90035626204422,7.360442777321));
#10866=CARTESIAN_POINT('Ctrl Pts',(-3.466494937956,5.81168666095527,7.36857654752598));
#10867=CARTESIAN_POINT('Ctrl Pts',(-3.61504215346738,5.72308274944759,7.3767042919459));
#10868=CARTESIAN_POINT('Ctrl Pts',(-3.76031241329552,5.62870681590016,7.38483203636581));
#10869=CARTESIAN_POINT('Ctrl Pts',(-3.90182804519759,5.52883594490825,7.39295978078573));
#10870=CARTESIAN_POINT('Ctrl Pts',(-4.04326858990214,5.42901806469706,7.4010832126817));
#10871=CARTESIAN_POINT('Ctrl Pts',(-4.18095817601844,5.32371126386678,7.40920664457768));
#10872=CARTESIAN_POINT('Ctrl Pts',(-4.31444695146456,5.213236662861,7.41733007647365));
#10873=CARTESIAN_POINT('Ctrl Pts',(-4.44878252714567,5.10206125448188,7.42550504022326));
#10874=CARTESIAN_POINT('Ctrl Pts',(-4.57886349229339,4.98565245184027,7.43368000397286));
#10875=CARTESIAN_POINT('Ctrl Pts',(-4.70426372759376,4.86437989688775,7.44185496772247));
#10876=CARTESIAN_POINT('Ctrl Pts',(-4.82884522113193,4.74389913395309,7.44997655689738));
#10877=CARTESIAN_POINT('Ctrl Pts',(-4.94880667653275,4.61861821717317,7.45809814607229));
#10878=CARTESIAN_POINT('Ctrl Pts',(-5.06376621136556,4.48893759776548,7.4662197352472));
#10879=CARTESIAN_POINT('Ctrl Pts',(-5.17874092321446,4.35923985785665,7.47434239663843));
#10880=CARTESIAN_POINT('Ctrl Pts',(-5.28871215637903,4.22514153226331,7.48246505802966));
#10881=CARTESIAN_POINT('Ctrl Pts',(-5.39333750674595,4.08707713877869,7.49058771942089));
#10882=CARTESIAN_POINT('Ctrl Pts',(-5.49799659356594,3.94896822641872,7.49871299996498));
#10883=CARTESIAN_POINT('Ctrl Pts',(-5.59730614408126,3.80689099110871,7.50683828050906));
#10884=CARTESIAN_POINT('Ctrl Pts',(-5.69096640168317,3.66130993155637,7.51496356105314));
#10885=CARTESIAN_POINT('Ctrl Pts',(-5.78564706829542,3.51414279666423,7.5231773648374));
#10886=CARTESIAN_POINT('Ctrl Pts',(-5.8745544172481,3.36339536639403,7.53139116862166));
#10887=CARTESIAN_POINT('Ctrl Pts',(-5.9574263274126,3.20957326656539,7.53960497240592));
#10888=CARTESIAN_POINT('Ctrl Pts',(-6.03954695532302,3.05714565388755,7.54774431326288));
#10889=CARTESIAN_POINT('Ctrl Pts',(-6.11574102122482,2.90169924571963,7.55588365411985));
#10890=CARTESIAN_POINT('Ctrl Pts',(-6.18580201378812,2.74374606081081,7.56402299497681));
#10891=CARTESIAN_POINT('Ctrl Pts',(-6.25682443799939,2.58362531895894,7.57227403022472));
#10892=CARTESIAN_POINT('Ctrl Pts',(-6.32154409751292,2.42092886630554,7.58052506547263));
#10893=CARTESIAN_POINT('Ctrl Pts',(-6.37979827012356,2.25620544998198,7.58877610072053));
#10894=CARTESIAN_POINT('Ctrl Pts',(-6.43805244273421,2.09148203365842,7.59702713596844));
#10895=CARTESIAN_POINT('Ctrl Pts',(-6.48984107863011,1.9247320401606,7.60527817121635));
#10896=CARTESIAN_POINT('Ctrl Pts',(-6.53505529828139,1.75651394768285,7.61352920646426));
#10897=CARTESIAN_POINT('Ctrl Pts',(-6.59561712467624,1.53119556351781,7.62458098991017));
#10898=CARTESIAN_POINT('Ctrl Pts',(-6.64454081796998,1.30267368207627,7.63563277335607));
#10899=CARTESIAN_POINT('Ctrl Pts',(-6.68155380170293,1.07197378463705,7.64668455680198));
#10900=CARTESIAN_POINT('Ctrl Pts',(-6.71759850281841,0.847309139642104,
7.65744721873637));
#10901=CARTESIAN_POINT('Ctrl Pts',(-6.74234764100618,0.620578598254374,
7.66820988067075));
#10902=CARTESIAN_POINT('Ctrl Pts',(-6.75559287276856,0.392751750344489,
7.67897254260514));
#10903=CARTESIAN_POINT('Ctrl Pts',(-6.76306187783386,0.264279866154085,
7.68504162300676));
#10904=CARTESIAN_POINT('Ctrl Pts',(-6.76687359068,0.135459811375129,7.69111070340839));
#10905=CARTESIAN_POINT('Ctrl Pts',(-6.76699690759725,0.00646935617321545,
7.69717978381002));
#10906=CARTESIAN_POINT('',(-6.76699976915238,-0.00176756656877366,7.30282021615314));
#10907=CARTESIAN_POINT('Ctrl Pts',(3.0991757505326,6.01559628526638,6.65133473543275));
#10908=CARTESIAN_POINT('Ctrl Pts',(2.9577462882066,6.08845934642711,6.65884513280887));
#10909=CARTESIAN_POINT('Ctrl Pts',(2.81385032318343,6.15627895275546,6.66635553018499));
#10910=CARTESIAN_POINT('Ctrl Pts',(2.66786098159252,6.21890720166302,6.67386592756111));
#10911=CARTESIAN_POINT('Ctrl Pts',(2.50796169101893,6.28750270638314,6.68209191994713));
#10912=CARTESIAN_POINT('Ctrl Pts',(2.34520526418079,6.35001733527718,6.69031791233315));
#10913=CARTESIAN_POINT('Ctrl Pts',(2.18009410799565,6.40620626270203,6.69854390471918));
#10914=CARTESIAN_POINT('Ctrl Pts',(2.01515604956891,6.46233628328128,6.70676127321281));
#10915=CARTESIAN_POINT('Ctrl Pts',(1.84786851415233,6.51215369404529,6.71497864170645));
#10916=CARTESIAN_POINT('Ctrl Pts',(1.67875537281941,6.55546103628341,6.72319601020009));
#10917=CARTESIAN_POINT('Ctrl Pts',(1.50978568599895,6.59873164196979,6.73140640810243));
#10918=CARTESIAN_POINT('Ctrl Pts',(1.33899382267921,6.63550308920923,6.73961680600477));
#10919=CARTESIAN_POINT('Ctrl Pts',(1.1669204561316,6.66562717597239,6.74782720390712));
#10920=CARTESIAN_POINT('Ctrl Pts',(0.994958633739034,6.6957317352173,6.75603227953376));
#10921=CARTESIAN_POINT('Ctrl Pts',(0.821717314504548,6.71919745575553,6.76423735516041));
#10922=CARTESIAN_POINT('Ctrl Pts',(0.647749147972829,6.73592681383197,6.77244243078706));
#10923=CARTESIAN_POINT('Ctrl Pts',(0.47385896046791,6.75264867318558,6.7806438285925));
#10924=CARTESIAN_POINT('Ctrl Pts',(0.299242930652763,6.76264015156045,6.78884522639794));
#10925=CARTESIAN_POINT('Ctrl Pts',(0.124460741667302,6.76585534310213,6.79704662420338));
#10926=CARTESIAN_POINT('Ctrl Pts',(-0.0503077568719296,6.76907028280232,
6.80524737960472));
#10927=CARTESIAN_POINT('Ctrl Pts',(-0.225242030875551,6.76550997761102,
6.81344813500605));
#10928=CARTESIAN_POINT('Ctrl Pts',(-0.399780088322315,6.75518059573399,
6.82164889040739));
#10929=CARTESIAN_POINT('Ctrl Pts',(-0.57431725916889,6.74485126632707,6.82984960415138));
#10930=CARTESIAN_POINT('Ctrl Pts',(-0.748457859656909,6.72775294883227,
6.83805031789538));
#10931=CARTESIAN_POINT('Ctrl Pts',(-0.921642836535204,6.70394387520237,
6.84625103163937));
#10932=CARTESIAN_POINT('Ctrl Pts',(-1.09485831912054,6.6801306077178,6.85445318989995));
#10933=CARTESIAN_POINT('Ctrl Pts',(-1.2671174876918,6.64960427784065,6.86265534816053));
#10934=CARTESIAN_POINT('Ctrl Pts',(-1.43786926684679,6.61247464807673,6.87085750642111));
#10935=CARTESIAN_POINT('Ctrl Pts',(-1.60868206791768,6.57533174922036,6.87906259590392));
#10936=CARTESIAN_POINT('Ctrl Pts',(-1.77798605648574,6.53158092564861,6.88726768538673));
#10937=CARTESIAN_POINT('Ctrl Pts',(-1.94524309557896,6.48138243734332,6.89547277486954));
#10938=CARTESIAN_POINT('Ctrl Pts',(-2.1126912060525,6.43112660320373,6.90368723769641));
#10939=CARTESIAN_POINT('Ctrl Pts',(-2.27808735174958,6.37440849209118,6.91190170052328));
#10940=CARTESIAN_POINT('Ctrl Pts',(-2.44091022994374,6.31143773235196,6.92011616335015));
#10941=CARTESIAN_POINT('Ctrl Pts',(-2.60382957553541,6.24842966443234,6.92833549298602));
#10942=CARTESIAN_POINT('Ctrl Pts',(-2.7641722861174,6.1791617052847,6.9365548226219));
#10943=CARTESIAN_POINT('Ctrl Pts',(-2.92143973013384,6.10389047273913,6.94477415225778));
#10944=CARTESIAN_POINT('Ctrl Pts',(-3.07895085053445,6.02850261197535,6.95300621724736));
#10945=CARTESIAN_POINT('Ctrl Pts',(-3.23337686536588,5.9470930563785,6.96123828223694));
#10946=CARTESIAN_POINT('Ctrl Pts',(-3.38424514690154,5.85996363347704,6.96947034722653));
#10947=CARTESIAN_POINT('Ctrl Pts',(-3.519856430504,5.78164542928634,6.97686992047395));
#10948=CARTESIAN_POINT('Ctrl Pts',(-3.65259340203968,5.69870643024907,6.98426949372138));
#10949=CARTESIAN_POINT('Ctrl Pts',(-3.7821351902108,5.61139398037325,6.9916690669688));
#10950=CARTESIAN_POINT('Ctrl Pts',(-3.92441161092521,5.51549826187561,6.99979605680985));
#10951=CARTESIAN_POINT('Ctrl Pts',(-4.06327781887667,5.41402657110997,7.0079230466509));
#10952=CARTESIAN_POINT('Ctrl Pts',(-4.19825979227066,5.30725010872896,7.01605003649194));
#10953=CARTESIAN_POINT('Ctrl Pts',(-4.33307753009959,5.20060356364129,7.02416713804395));
#10954=CARTESIAN_POINT('Ctrl Pts',(-4.46402015411438,5.08866531908903,7.03228423959595));
#10955=CARTESIAN_POINT('Ctrl Pts',(-4.59064053134282,4.97175105088666,7.04040134114795));
#10956=CARTESIAN_POINT('Ctrl Pts',(-4.71713389446909,4.85495406049637,7.04851030035834));
#10957=CARTESIAN_POINT('Ctrl Pts',(-4.83931337293362,4.73319123036887,7.05661925956874));
#10958=CARTESIAN_POINT('Ctrl Pts',(-4.95676303128499,4.60681986316879,7.06472821877914));
#10959=CARTESIAN_POINT('Ctrl Pts',(-5.07411994308032,4.48054828773697,7.07283077458189));
#10960=CARTESIAN_POINT('Ctrl Pts',(-5.18675422130604,4.34967568903663,7.08093333038464));
#10961=CARTESIAN_POINT('Ctrl Pts',(-5.29428512757639,4.21459772551586,7.08903588618739));
#10962=CARTESIAN_POINT('Ctrl Pts',(-5.40175405835308,4.07959761424951,7.0971337720779));
#10963=CARTESIAN_POINT('Ctrl Pts',(-5.50412524544081,3.94039725193013,7.10523165796841));
#10964=CARTESIAN_POINT('Ctrl Pts',(-5.60105679618804,3.79742699283025,7.11332954385892));
#10965=CARTESIAN_POINT('Ctrl Pts',(-5.69796499854406,3.65449117169732,7.12142547917084));
#10966=CARTESIAN_POINT('Ctrl Pts',(-5.78943596202585,3.50778756300871,7.12952141448275));
#10967=CARTESIAN_POINT('Ctrl Pts',(-5.87516979223443,3.35777737683964,7.13761734979467));
#10968=CARTESIAN_POINT('Ctrl Pts',(-5.96089526601023,3.20778181208704,7.14571249599989));
#10969=CARTESIAN_POINT('Ctrl Pts',(-6.04088453607234,3.05448063083582,7.15380764220512));
#10970=CARTESIAN_POINT('Ctrl Pts',(-6.1148826341711,2.89836149752109,7.16190278841034));
#10971=CARTESIAN_POINT('Ctrl Pts',(-6.18888781242569,2.74222742669011,7.16999870916111));
#10972=CARTESIAN_POINT('Ctrl Pts',(-6.25690051941951,2.58327519992421,7.17809462991187));
#10973=CARTESIAN_POINT('Ctrl Pts',(-6.31871312917002,2.42201432515468,7.18619055066263));
#10974=CARTESIAN_POINT('Ctrl Pts',(-6.38054359334956,2.26070687055528,7.19428880990133));
#10975=CARTESIAN_POINT('Ctrl Pts',(-6.43617026313767,2.09708978429863,7.20238706914003));
#10976=CARTESIAN_POINT('Ctrl Pts',(-6.48543478515187,1.93168958363971,7.21048532837874));
#10977=CARTESIAN_POINT('Ctrl Pts',(-6.53475099061234,1.76611586150863,7.21859208350716));
#10978=CARTESIAN_POINT('Ctrl Pts',(-6.57769161173451,1.59875564208336,7.2266988386356));
#10979=CARTESIAN_POINT('Ctrl Pts',(-6.61414882311636,1.43014836491482,7.23480559376402));
#10980=CARTESIAN_POINT('Ctrl Pts',(-6.65062624168162,1.26144763358326,7.24291684223359));
#10981=CARTESIAN_POINT('Ctrl Pts',(-6.68061302708018,1.09149882952185,7.25102809070316));
#10982=CARTESIAN_POINT('Ctrl Pts',(-6.70405308758127,0.920848086761328,
7.25913933917273));
#10983=CARTESIAN_POINT('Ctrl Pts',(-6.72752745630857,0.749947569718673,
7.26726245973398));
#10984=CARTESIAN_POINT('Ctrl Pts',(-6.74443592206768,0.578343427576287,
7.27538558029523));
#10985=CARTESIAN_POINT('Ctrl Pts',(-6.75477446505585,0.406584463831959,
7.28350870085649));
#10986=CARTESIAN_POINT('Ctrl Pts',(-6.76296724965365,0.270473969895757,
7.28994587262204));
#10987=CARTESIAN_POINT('Ctrl Pts',(-6.76703530173109,0.134266321004993,
7.29638304438759));
#10988=CARTESIAN_POINT('Ctrl Pts',(-6.76699976915239,-0.00176756656875029,
7.30282021615314));
#10989=CARTESIAN_POINT('Ctrl Pts',(-6.76699976915218,-0.00176756734519897,
7.30282021618988));
#10990=CARTESIAN_POINT('Ctrl Pts',(-6.76698752969479,-0.0486254172486542,
7.30503754625208));
#10991=CARTESIAN_POINT('Ctrl Pts',(-6.76648859969451,-0.0954783083698461,
7.30725487631427));
#10992=CARTESIAN_POINT('Ctrl Pts',(-6.76550324311227,-0.142319596111774,
7.30947220637647));
#10993=CARTESIAN_POINT('Ctrl Pts',(-6.76184760804056,-0.316098974419329,
7.3176984157376));
#10994=CARTESIAN_POINT('Ctrl Pts',(-6.75148698982309,-0.489980337408581,
7.32592462509874));
#10995=CARTESIAN_POINT('Ctrl Pts',(-6.73440283697741,-0.663405931018561,
7.33415083445988));
#10996=CARTESIAN_POINT('Ctrl Pts',(-6.71733787744475,-0.836636688412039,
7.34236780202761));
#10997=CARTESIAN_POINT('Ctrl Pts',(-6.69356445939919,-1.00941234236451,
7.35058476959534));
#10998=CARTESIAN_POINT('Ctrl Pts',(-6.66311601983172,-1.1811747991986,7.35880173716306));
#10999=CARTESIAN_POINT('Ctrl Pts',(-6.63269567653462,-1.35277876237934,
7.36701112253132));
#11000=CARTESIAN_POINT('Ctrl Pts',(-6.59561264053686,-1.52337103947165,
7.37522050789958));
#11001=CARTESIAN_POINT('Ctrl Pts',(-6.55195216944722,-1.69239823010894,
7.38342989326784));
#11002=CARTESIAN_POINT('Ctrl Pts',(-6.50832322582457,-1.8613033652796,7.39163335059364));
#11003=CARTESIAN_POINT('Ctrl Pts',(-6.45812639683201,-2.02864531924276,
7.39983680791945));
#11004=CARTESIAN_POINT('Ctrl Pts',(-6.40149809730226,-2.19388037737602,
7.40804026524525));
#11005=CARTESIAN_POINT('Ctrl Pts',(-6.34489932988242,-2.35902926410844,
7.41623944440262));
#11006=CARTESIAN_POINT('Ctrl Pts',(-6.2818758898107,-2.52207310548398,7.42443862356));
#11007=CARTESIAN_POINT('Ctrl Pts',(-6.21261419681645,-2.68248277562312,
7.43263780271737));
#11008=CARTESIAN_POINT('Ctrl Pts',(-6.14336555421465,-2.84286222113075,
7.44083543697307));
#11009=CARTESIAN_POINT('Ctrl Pts',(-6.06788113631693,-3.00060815266827,
7.44903307122876));
#11010=CARTESIAN_POINT('Ctrl Pts',(-5.98639583441627,-3.15521059735853,
7.45723070548445));
#11011=CARTESIAN_POINT('Ctrl Pts',(-5.90491641421171,-3.30980188267925,
7.46542774802615));
#11012=CARTESIAN_POINT('Ctrl Pts',(-5.81743713910388,-3.46124981532172,
7.47362479056785));
#11013=CARTESIAN_POINT('Ctrl Pts',(-5.72423925008868,-3.60906830189513,
7.48182183310955));
#11014=CARTESIAN_POINT('Ctrl Pts',(-5.6310311496367,-3.75690298453421,7.4900197737787));
#11015=CARTESIAN_POINT('Ctrl Pts',(-5.53210337829873,-3.90110712536116,
7.49821771444784));
#11016=CARTESIAN_POINT('Ctrl Pts',(-5.42778098858982,-4.04122290153649,
7.50641565511699));
#11017=CARTESIAN_POINT('Ctrl Pts',(-5.32342820807334,-4.18137949571457,
7.51461598397948));
#11018=CARTESIAN_POINT('Ctrl Pts',(-5.21367789301692,-4.31744506527575,
7.52281631284197));
#11019=CARTESIAN_POINT('Ctrl Pts',(-5.09889594358894,-4.44899417356916,
7.53101664170447));
#11020=CARTESIAN_POINT('Ctrl Pts',(-4.9839943883899,-4.58068035944843,7.53922551552252));
#11021=CARTESIAN_POINT('Ctrl Pts',(-4.8640509600376,-4.70784041102398,7.54743438934057));
#11022=CARTESIAN_POINT('Ctrl Pts',(-4.73946974533751,-4.83008442297134,
7.55564326315862));
#11023=CARTESIAN_POINT('Ctrl Pts',(-4.6148216692723,-4.95239404193286,7.56385654258879));
#11024=CARTESIAN_POINT('Ctrl Pts',(-4.4855311101498,-5.0697821206818,7.57206982201896));
#11025=CARTESIAN_POINT('Ctrl Pts',(-4.35203583918027,-5.181898595543,7.58028310144913));
#11026=CARTESIAN_POINT('Ctrl Pts',(-4.21834531039661,-5.29417905836909,
7.58850839409128));
#11027=CARTESIAN_POINT('Ctrl Pts',(-4.08043806266068,-5.40117228842603,
7.59673368673343));
#11028=CARTESIAN_POINT('Ctrl Pts',(-3.9387825246479,-5.50257041967919,7.60495897937558));
#11029=CARTESIAN_POINT('Ctrl Pts',(-3.8106721125475,-5.5942728448952,7.61239776817843));
#11030=CARTESIAN_POINT('Ctrl Pts',(-3.67949649292701,-5.68139948981056,
7.61983655698129));
#11031=CARTESIAN_POINT('Ctrl Pts',(-3.54561914823371,-5.76375518700079,
7.62727534578415));
#11032=CARTESIAN_POINT('Ctrl Pts',(-3.39757059137176,-5.85482841635341,
7.63550154678617));
#11033=CARTESIAN_POINT('Ctrl Pts',(-3.24580387325173,-5.94032108328819,
7.64372774778819));
#11034=CARTESIAN_POINT('Ctrl Pts',(-3.09077776091241,-6.01991543401145,
7.65195394879021));
#11035=CARTESIAN_POINT('Ctrl Pts',(-2.93592578774073,-6.09942037725506,
7.66017090938896));
#11036=CARTESIAN_POINT('Ctrl Pts',(-2.77782202702455,-6.17304003517207,
7.6683878699877));
#11037=CARTESIAN_POINT('Ctrl Pts',(-2.61695369561579,-6.24050016865658,
7.67660483058645));
#11038=CARTESIAN_POINT('Ctrl Pts',(-2.45623377832424,-6.30789806468224,
7.68481421037086));
#11039=CARTESIAN_POINT('Ctrl Pts',(-2.29275469849348,-6.36914761568798,
7.69302359015528));
#11040=CARTESIAN_POINT('Ctrl Pts',(-2.12702780144999,-6.4240206827079,7.70123296993969));
#11041=CARTESIAN_POINT('Ctrl Pts',(-1.96142054891306,-6.47885413478815,
7.70943642306276));
#11042=CARTESIAN_POINT('Ctrl Pts',(-1.79356905055117,-6.52732015984342,
7.71763987618583));
#11043=CARTESIAN_POINT('Ctrl Pts',(-1.62400422441038,-6.56923886604051,
7.7258433293089));
#11044=CARTESIAN_POINT('Ctrl Pts',(-1.45452779923989,-6.61113571832848,
7.7340425056416));
#11045=CARTESIAN_POINT('Ctrl Pts',(-1.28334017308492,-6.64649196595729,
7.7422416819743));
#11046=CARTESIAN_POINT('Ctrl Pts',(-1.11098709125494,-6.67517765179811,
7.750440858307));
#11047=CARTESIAN_POINT('Ctrl Pts',(-0.938666440261681,-6.70385793999367,
7.75863849184078));
#11048=CARTESIAN_POINT('Ctrl Pts',(-0.765181122795862,-6.72587010160438,
7.76683612537456));
#11049=CARTESIAN_POINT('Ctrl Pts',(-0.591087044441642,-6.74113529799642,
7.77503375890834));
#11050=CARTESIAN_POINT('Ctrl Pts',(-0.417005505135572,-6.75639939491951,
7.78323080201123));
#11051=CARTESIAN_POINT('Ctrl Pts',(-0.242315649492823,-6.76491746220367,
7.79142784511412));
#11052=CARTESIAN_POINT('Ctrl Pts',(-0.0675784208831055,-6.76666255675802,
7.79962488821701));
#11053=CARTESIAN_POINT('Ctrl Pts',(0.107177980555809,-6.76840784279074,
7.80782283073045));
#11054=CARTESIAN_POINT('Ctrl Pts',(0.281981406580633,-6.76337867192868,
7.81602077324388));
#11055=CARTESIAN_POINT('Ctrl Pts',(0.456270941966133,-6.75160024198096,
7.82421871575733));
#11056=CARTESIAN_POINT('Ctrl Pts',(0.630611278008756,-6.7398183789414,7.83241904774794));
#11057=CARTESIAN_POINT('Ctrl Pts',(0.804437067284309,-6.72128336251896,
7.84061937973855));
#11058=CARTESIAN_POINT('Ctrl Pts',(0.9771924877412,-6.69607226976398,7.84881971172917));
#11059=CARTESIAN_POINT('Ctrl Pts',(1.15012796603896,-6.67083490023624,7.85702859068213));
#11060=CARTESIAN_POINT('Ctrl Pts',(1.32199049130191,-6.63890760465673,7.86523746963509));
#11061=CARTESIAN_POINT('Ctrl Pts',(1.49223341972256,-6.60041880648972,7.87344634858804));
#11062=CARTESIAN_POINT('Ctrl Pts',(1.66256773849562,-6.56190934664318,7.88165963425761));
#11063=CARTESIAN_POINT('Ctrl Pts',(1.83128038098567,-6.51683145474681,7.88987291992717));
#11064=CARTESIAN_POINT('Ctrl Pts',(1.99783994387982,-6.46536345139531,7.89808620559674));
#11065=CARTESIAN_POINT('Ctrl Pts',(2.16464316288966,-6.41382015669721,7.90631150629113));
#11066=CARTESIAN_POINT('Ctrl Pts',(2.32928666954229,-6.3558681883647,7.91453680698553));
#11067=CARTESIAN_POINT('Ctrl Pts',(2.49125792102187,-6.29173449622168,7.92276210767992));
#11068=CARTESIAN_POINT('Ctrl Pts',(2.63774138419605,-6.23373330622382,7.93020090018388));
#11069=CARTESIAN_POINT('Ctrl Pts',(2.78203930985302,-6.17067676984828,7.93763969268784));
#11070=CARTESIAN_POINT('Ctrl Pts',(2.92379073791715,-6.10276467847728,7.94507848519181));
#11071=CARTESIAN_POINT('Ctrl Pts',(3.07914343599351,-6.02833631630432,7.95323104140731));
#11072=CARTESIAN_POINT('Ctrl Pts',(3.23189528432432,-5.94785565104467,7.96138359762281));
#11073=CARTESIAN_POINT('Ctrl Pts',(3.38153615325296,-5.86152729621241,7.96953615383832));
#11074=CARTESIAN_POINT('Ctrl Pts',(3.53100365962748,-5.77529895486039,7.97767926512091));
#11075=CARTESIAN_POINT('Ctrl Pts',(3.67736704758343,-5.68323659041015,7.9858223764035));
#11076=CARTESIAN_POINT('Ctrl Pts',(3.82013675003357,-5.58559255684149,7.99396548768609));
#11077=CARTESIAN_POINT('Ctrl Pts',(3.96277106589319,-5.48804111779786,8.00210087696567));
#11078=CARTESIAN_POINT('Ctrl Pts',(4.10181818116243,-5.38491875231458,8.01023626624525));
#11079=CARTESIAN_POINT('Ctrl Pts',(4.23681371614003,-5.27652333783598,8.01837165552482));
#11080=CARTESIAN_POINT('Ctrl Pts',(4.37170960248498,-5.16820793678033,8.02650103956565));
#11081=CARTESIAN_POINT('Ctrl Pts',(4.50255957975303,-5.05462746502777,8.03463042360648));
#11082=CARTESIAN_POINT('Ctrl Pts',(4.62892883536721,-4.93612265215381,8.0427598076473));
#11083=CARTESIAN_POINT('Ctrl Pts',(4.75523135353173,-4.81768042340244,8.05088489844168));
#11084=CARTESIAN_POINT('Ctrl Pts',(4.87705759663659,-4.69431928226894,8.05900998923605));
#11085=CARTESIAN_POINT('Ctrl Pts',(4.99400640904814,-4.56641971202672,8.06713508003043));
#11086=CARTESIAN_POINT('Ctrl Pts',(5.11140164037723,-4.43803192145523,8.07529118605414));
#11087=CARTESIAN_POINT('Ctrl Pts',(5.22388184578451,-4.30507122419482,8.08344729207785));
#11088=CARTESIAN_POINT('Ctrl Pts',(5.3310788343176,-4.16795962819831,8.09160339810156));
#11089=CARTESIAN_POINT('Ctrl Pts',(5.4378443744059,-4.0313998815183,8.09972667727717));
#11090=CARTESIAN_POINT('Ctrl Pts',(5.53936893675134,-3.89072289073989,8.10784995645278));
#11091=CARTESIAN_POINT('Ctrl Pts',(5.63532956659387,-3.74637820779923,8.11597323562839));
#11092=CARTESIAN_POINT('Ctrl Pts',(5.73130297440501,-3.6020143041445,8.12409759648726));
#11093=CARTESIAN_POINT('Ctrl Pts',(5.82171077145809,-3.45398204023489,8.13222195734612));
#11094=CARTESIAN_POINT('Ctrl Pts',(5.90627381256288,-3.30275924811875,8.14034631820498));
#11095=CARTESIAN_POINT('Ctrl Pts',(5.99086420250468,-3.15148754849598,8.14847330659259));
#11096=CARTESIAN_POINT('Ctrl Pts',(6.06960589391021,-2.99702358503507,8.1566002949802));
#11097=CARTESIAN_POINT('Ctrl Pts',(6.1422661238186,-2.83986898715247,8.1647272833678));
#11098=CARTESIAN_POINT('Ctrl Pts',(6.21539609378466,-2.68169840280844,8.17290681180378));
#11099=CARTESIAN_POINT('Ctrl Pts',(6.28236554001722,-2.52080261527084,8.18108634023975));
#11100=CARTESIAN_POINT('Ctrl Pts',(6.34298702717897,-2.35771172390504,8.18926586867573));
#11101=CARTESIAN_POINT('Ctrl Pts',(6.40332302826017,-2.19538888000113,8.19740687708154));
#11102=CARTESIAN_POINT('Ctrl Pts',(6.45737067781465,-2.03089192985121,8.20554788548735));
#11103=CARTESIAN_POINT('Ctrl Pts',(6.50499590511038,-1.86475662607675,8.21368889389316));
#11104=CARTESIAN_POINT('Ctrl Pts',(6.55295914799961,-1.69744219253233,8.22188768234421));
#11105=CARTESIAN_POINT('Ctrl Pts',(6.59440837850788,-1.52846643040878,8.23008647079526));
#11106=CARTESIAN_POINT('Ctrl Pts',(6.62925944593312,-1.35838440748798,8.23828525924632));
#11107=CARTESIAN_POINT('Ctrl Pts',(6.66411051335837,-1.18830238456717,8.24648404769737));
#11108=CARTESIAN_POINT('Ctrl Pts',(6.69236342114684,-1.01711447780827,8.25468283614843));
#11109=CARTESIAN_POINT('Ctrl Pts',(6.7139872728954,-0.845377962451505,8.26288162459949));
#11110=CARTESIAN_POINT('Ctrl Pts',(6.73570148794889,-0.672923782208495,
8.27111467473664));
#11111=CARTESIAN_POINT('Ctrl Pts',(6.75079874565138,-0.499380333445228,
8.27934772487379));
#11112=CARTESIAN_POINT('Ctrl Pts',(6.75917681953755,-0.325296360610221,
8.28758077501095));
#11113=CARTESIAN_POINT('Ctrl Pts',(6.76754491642563,-0.151419695026239,
8.295804020851));
#11114=CARTESIAN_POINT('Ctrl Pts',(6.76920974544321,0.0229958586427361,
8.30402726669104));
#11115=CARTESIAN_POINT('Ctrl Pts',(6.76412040581053,0.197393352718985,8.31225051253109));
#11116=CARTESIAN_POINT('Ctrl Pts',(6.7590361081567,0.371618072223139,8.32046561164983));
#11117=CARTESIAN_POINT('Ctrl Pts',(6.74721097806552,0.545824412197253,8.32868071076857));
#11118=CARTESIAN_POINT('Ctrl Pts',(6.72864603823996,0.719452216674408,8.3368958098873));
#11119=CARTESIAN_POINT('Ctrl Pts',(6.71009577612072,0.892942748531908,8.34510441403146));
#11120=CARTESIAN_POINT('Ctrl Pts',(6.68481635566108,1.06585530138931,8.35331301817561));
#11121=CARTESIAN_POINT('Ctrl Pts',(6.65286082587563,1.23763154110155,8.36152162231977));
#11122=CARTESIAN_POINT('Ctrl Pts',(6.62092416859118,1.40930633210439,8.36972537857403));
#11123=CARTESIAN_POINT('Ctrl Pts',(6.58231932194603,1.57984579567035,8.3779291348283));
#11124=CARTESIAN_POINT('Ctrl Pts',(6.53715096824298,1.74869843552281,8.38613289108256));
#11125=CARTESIAN_POINT('Ctrl Pts',(6.49199597871709,1.91750111613588,8.39433422005217));
#11126=CARTESIAN_POINT('Ctrl Pts',(6.44028143919269,2.08461762062783,8.40253554902176));
#11127=CARTESIAN_POINT('Ctrl Pts',(6.38216282693135,2.24950809079134,8.41073687799137));
#11128=CARTESIAN_POINT('Ctrl Pts',(6.32405222978137,2.41437582098516,8.41893707591942));
#11129=CARTESIAN_POINT('Ctrl Pts',(6.25953943719118,2.57701779021335,8.42713727384749));
#11130=CARTESIAN_POINT('Ctrl Pts',(6.18882935908951,2.73691069713129,8.43533747177554));
#11131=CARTESIAN_POINT('Ctrl Pts',(6.11811621847773,2.89681052913908,8.44353802486074));
#11132=CARTESIAN_POINT('Ctrl Pts',(6.04120540247875,3.05396073391649,8.45173857794594));
#11133=CARTESIAN_POINT('Ctrl Pts',(5.95834941791655,3.20785928837497,8.45993913103113));
#11134=CARTESIAN_POINT('Ctrl Pts',(5.87547482966789,3.36179239773577,8.4681415253897));
#11135=CARTESIAN_POINT('Ctrl Pts',(5.78665258397753,3.51247208723095,8.47634391974827));
#11136=CARTESIAN_POINT('Ctrl Pts',(5.69218048709079,3.65942212683681,8.48454631410685));
#11137=CARTESIAN_POINT('Ctrl Pts',(5.59762004218647,3.80650959056166,8.49275637914602));
#11138=CARTESIAN_POINT('Ctrl Pts',(5.49739938388745,3.94986013414001,8.50096644418519));
#11139=CARTESIAN_POINT('Ctrl Pts',(5.39185943326424,4.08902688324734,8.50917650922437));
#11140=CARTESIAN_POINT('Ctrl Pts',(5.28626897309297,4.22826023509192,8.51739050345502));
#11141=CARTESIAN_POINT('Ctrl Pts',(5.17535437212263,4.36330552350885,8.52560449768567));
#11142=CARTESIAN_POINT('Ctrl Pts',(5.05949592397364,4.49375010378795,8.53381849191632));
#11143=CARTESIAN_POINT('Ctrl Pts',(4.94347952217289,4.62437252347483,8.5420436845568));
#11144=CARTESIAN_POINT('Ctrl Pts',(4.82250605119118,4.7503814412255,8.55026887719728));
#11145=CARTESIAN_POINT('Ctrl Pts',(4.69699250535623,4.87140127731513,8.55849406983776));
#11146=CARTESIAN_POINT('Ctrl Pts',(4.58411844345555,4.98023415570383,8.56589096789422));
#11147=CARTESIAN_POINT('Ctrl Pts',(4.46757326273479,5.08503258278129,8.57328786595068));
#11148=CARTESIAN_POINT('Ctrl Pts',(4.34768164610651,5.18555236248836,8.58068476400715));
#11149=CARTESIAN_POINT('Ctrl Pts',(4.20753111020087,5.3030576676236,8.58933156731006));
#11150=CARTESIAN_POINT('Ctrl Pts',(4.06248921193366,5.41498253421157,8.59797837061297));
#11151=CARTESIAN_POINT('Ctrl Pts',(3.91301657326871,5.52092295701764,8.60662517391588));
#11152=CARTESIAN_POINT('Ctrl Pts',(3.76378560526331,5.62669209301107,8.61525799687647));
#11153=CARTESIAN_POINT('Ctrl Pts',(3.61013843570947,5.72649591228951,8.62389081983705));
#11154=CARTESIAN_POINT('Ctrl Pts',(3.45256820668289,5.81997094307201,8.63252364279763));
#11155=CARTESIAN_POINT('Ctrl Pts',(3.33681818514436,5.88863706669974,8.63886525599322));
#11156=CARTESIAN_POINT('Ctrl Pts',(3.21895191095766,5.95388879123284,8.6452068691888));
#11157=CARTESIAN_POINT('Ctrl Pts',(3.09917575053261,6.01559628526638,8.65154848238438));
#11158=CARTESIAN_POINT('Origin',(0.,0.,-3.69717978381041));
#11159=CARTESIAN_POINT('',(3.0991757505326,6.01559628526639,11.0455440641533));
#11160=CARTESIAN_POINT('',(3.09917575053259,6.01559628526639,10.6513920151221));
#11161=CARTESIAN_POINT('',(3.09917575053259,6.01559628526639,-3.69717978381041));
#11162=CARTESIAN_POINT('',(-6.767,1.72459919609014E-12,9.69717978381002));
#11163=CARTESIAN_POINT('Ctrl Pts',(-6.76699931536137,-0.00304399388113017,
9.69717978381003));
#11164=CARTESIAN_POINT('Ctrl Pts',(-6.76691563275954,-0.189075941186378,
9.70587829366268));
#11165=CARTESIAN_POINT('Ctrl Pts',(-6.75915646223125,-0.374883524766316,
9.71457680351534));
#11166=CARTESIAN_POINT('Ctrl Pts',(-6.74380218515861,-0.559840233861357,
9.72327531336799));
#11167=CARTESIAN_POINT('Ctrl Pts',(-6.72841643646549,-0.74517604822634,
9.73199165253293));
#11168=CARTESIAN_POINT('Ctrl Pts',(-6.70540450111108,-0.929657222362386,
9.74070799169786));
#11169=CARTESIAN_POINT('Ctrl Pts',(-6.67489790911547,-1.11266657309634,
9.7494243308628));
#11170=CARTESIAN_POINT('Ctrl Pts',(-6.64429394823896,-1.29626004072139,
9.75816849025067));
#11171=CARTESIAN_POINT('Ctrl Pts',(-6.60614751276337,-1.47837200472053,
9.76691264963853));
#11172=CARTESIAN_POINT('Ctrl Pts',(-6.5606409249368,-1.6583967119011,9.7756568090264));
#11173=CARTESIAN_POINT('Ctrl Pts',(-6.51505618434852,-1.83873059251602,
9.78441598558513));
#11174=CARTESIAN_POINT('Ctrl Pts',(-6.46208612285544,-2.01696978566612,
9.79317516214386));
#11175=CARTESIAN_POINT('Ctrl Pts',(-6.4019618448933,-2.19252674705018,9.8019343387026));
#11176=CARTESIAN_POINT('Ctrl Pts',(-6.34167561950224,-2.36855657895322,
9.81071710849473));
#11177=CARTESIAN_POINT('Ctrl Pts',(-6.27419673216841,-2.54188946277467,
9.81949987828687));
#11178=CARTESIAN_POINT('Ctrl Pts',(-6.19980411841009,-2.71195831334946,
9.828282648079));
#11179=CARTESIAN_POINT('Ctrl Pts',(-6.16347570173305,-2.79500865605606,
9.83257157011666));
#11180=CARTESIAN_POINT('Ctrl Pts',(-6.12549925121098,-2.87728103007024,
9.83686049215433));
#11181=CARTESIAN_POINT('Ctrl Pts',(-6.08591104570938,-2.9587118385731,9.84114941419199));
#11182=CARTESIAN_POINT('Ctrl Pts',(-6.00992899708752,-3.11500282404684,
9.84938118622287));
#11183=CARTESIAN_POINT('Ctrl Pts',(-5.9278110264455,-3.26859445189463,9.85761295825376));
#11184=CARTESIAN_POINT('Ctrl Pts',(-5.83977091139031,-3.41897129301777,
9.86584473028464));
#11185=CARTESIAN_POINT('Ctrl Pts',(-5.75183592503064,-3.56916856916496,
9.87406667275709));
#11186=CARTESIAN_POINT('Ctrl Pts',(-5.6579930547608,-3.71615839630879,9.88228861522954));
#11187=CARTESIAN_POINT('Ctrl Pts',(-5.55850356303743,-3.85944648099961,
9.89051055770199));
#11188=CARTESIAN_POINT('Ctrl Pts',(-5.4591129381152,-4.00259217442547,9.89872432969194));
#11189=CARTESIAN_POINT('Ctrl Pts',(-5.35408706952809,-4.14204315897073,
9.90693810168188));
#11190=CARTESIAN_POINT('Ctrl Pts',(-5.24373247890332,-4.27733079030538,
9.91515187367183));
#11191=CARTESIAN_POINT('Ctrl Pts',(-5.13346544969492,-4.41251107697453,
9.92335912840223));
#11192=CARTESIAN_POINT('Ctrl Pts',(-5.01787834537423,-4.54353431375377,
9.93156638313264));
#11193=CARTESIAN_POINT('Ctrl Pts',(-4.89732028676702,-4.66996177808986,
9.93977363786304));
#11194=CARTESIAN_POINT('Ctrl Pts',(-4.77683374576919,-4.79631424296002,
9.94797602387504));
#11195=CARTESIAN_POINT('Ctrl Pts',(-4.65138237160784,-4.91807610790113,
9.95617840988704));
#11196=CARTESIAN_POINT('Ctrl Pts',(-4.52135481620011,-5.03484256218842,
9.96438079589904));
#11197=CARTESIAN_POINT('Ctrl Pts',(-4.39136607086359,-5.15157416452151,
9.97258073369779));
#11198=CARTESIAN_POINT('Ctrl Pts',(-4.25680412872402,-5.26331308423868,
9.98078067149653));
#11199=CARTESIAN_POINT('Ctrl Pts',(-4.11809384882402,-5.36969198858536,
9.98898060929528));
#11200=CARTESIAN_POINT('Ctrl Pts',(-3.97940296420127,-5.47605601841556,
9.99717940053108));
#11201=CARTESIAN_POINT('Ctrl Pts',(-3.83656518087139,-5.57706130684962,
10.0053781917669));
#11202=CARTESIAN_POINT('Ctrl Pts',(-3.69003773789161,-5.67238137759934,
10.0135769830027));
#11203=CARTESIAN_POINT('Ctrl Pts',(-3.54350420239129,-5.7677054116987,10.0217761151391));
#11204=CARTESIAN_POINT('Ctrl Pts',(-3.39328100202644,-5.85734356164554,
10.0299752472756));
#11205=CARTESIAN_POINT('Ctrl Pts',(-3.23985363895098,-5.94101316259913,
10.0381743794121));
#11206=CARTESIAN_POINT('Ctrl Pts',(-3.0863920640432,-6.02470142052694,10.0463753398231));
#11207=CARTESIAN_POINT('Ctrl Pts',(-2.92972521800756,-6.10241830714088,
10.054576300234));
#11208=CARTESIAN_POINT('Ctrl Pts',(-2.77036247488132,-6.17392749858382,
10.062777260645));
#11209=CARTESIAN_POINT('Ctrl Pts',(-2.61085037050137,-6.24550371135356,
10.0709859073301));
#11210=CARTESIAN_POINT('Ctrl Pts',(-2.44863764827458,-6.31086045780384,
10.0791945540152));
#11211=CARTESIAN_POINT('Ctrl Pts',(-2.28425378236797,-6.36980954642583,
10.0874032007002));
#11212=CARTESIAN_POINT('Ctrl Pts',(-2.11979143498689,-6.42878677899837,
10.0956157664238));
#11213=CARTESIAN_POINT('Ctrl Pts',(-1.9531562188367,-6.48135014645744,10.1038283321474));
#11214=CARTESIAN_POINT('Ctrl Pts',(-1.7848919051021,-6.52736163293417,10.1120408978709));
#11215=CARTESIAN_POINT('Ctrl Pts',(-1.61639670844841,-6.57343625380983,
10.1202647324197));
#11216=CARTESIAN_POINT('Ctrl Pts',(-1.44626829600009,-6.6129409453816,10.1284885669685));
#11217=CARTESIAN_POINT('Ctrl Pts',(-1.27506096342839,-6.64578878234488,
10.1367124015174));
#11218=CARTESIAN_POINT('Ctrl Pts',(-1.11775363041975,-6.67596976554333,
10.1442685584912));
#11219=CARTESIAN_POINT('Ctrl Pts',(-0.959535757706112,-6.70053149720022,
10.151824715465));
#11220=CARTESIAN_POINT('Ctrl Pts',(-0.800839558192604,-6.71944528975673,
10.1593808724388));
#11221=CARTESIAN_POINT('Ctrl Pts',(-0.619260138690586,-6.7410863591933,
10.1680265904911));
#11222=CARTESIAN_POINT('Ctrl Pts',(-0.436640606077396,-6.75538226963625,
10.1766723085434));
#11223=CARTESIAN_POINT('Ctrl Pts',(-0.253587320618503,-6.76224685077538,
10.1853180265958));
#11224=CARTESIAN_POINT('Ctrl Pts',(-0.0707690382729579,-6.76910261919128,
10.1939526453081));
#11225=CARTESIAN_POINT('Ctrl Pts',(0.112481583221877,-6.76854607080577,
10.2025872640203));
#11226=CARTESIAN_POINT('Ctrl Pts',(0.295552513121757,-6.76054270839164,
10.2112218827326));
#11227=CARTESIAN_POINT('Ctrl Pts',(0.485088797093329,-6.75225669830757,
10.2201614426351));
#11228=CARTESIAN_POINT('Ctrl Pts',(0.674432150438052,-6.73598822265197,
10.2291010025376));
#11229=CARTESIAN_POINT('Ctrl Pts',(0.862899522178615,-6.71175784833034,
10.23804056244));
#11230=CARTESIAN_POINT('Ctrl Pts',(1.04443275295916,-6.68841896429431,10.2466512157105));
#11231=CARTESIAN_POINT('Ctrl Pts',(1.2251529601535,-6.65769360214627,10.2552618689809));
#11232=CARTESIAN_POINT('Ctrl Pts',(1.40445101194971,-6.61965303887095,10.2638725222514));
#11233=CARTESIAN_POINT('Ctrl Pts',(1.58357934614409,-6.58164848353386,10.2724750249624));
#11234=CARTESIAN_POINT('Ctrl Pts',(1.76128791146506,-6.53634259540759,10.2810775276734));
#11235=CARTESIAN_POINT('Ctrl Pts',(1.93697516794393,-6.48385812605185,10.2896800303845));
#11236=CARTESIAN_POINT('Ctrl Pts',(2.11246469195233,-6.43143272690982,10.2982728511519));
#11237=CARTESIAN_POINT('Ctrl Pts',(2.2859371539519,-6.3718449517129,10.3068656719193));
#11238=CARTESIAN_POINT('Ctrl Pts',(2.45680342999803,-6.30526810741224,10.3154584926867));
#11239=CARTESIAN_POINT('Ctrl Pts',(2.47694079675369,-6.29742172390029,10.3164711956452));
#11240=CARTESIAN_POINT('Ctrl Pts',(2.49704197929952,-6.28947832197825,10.3174838986037));
#11241=CARTESIAN_POINT('Ctrl Pts',(2.51710602579774,-6.28143823139993,10.3184966015622));
#11242=CARTESIAN_POINT('Ctrl Pts',(2.68739845944339,-6.21319842785709,10.3270918593223));
#11243=CARTESIAN_POINT('Ctrl Pts',(2.85481392433213,-6.13806977349865,10.3356871170823));
#11244=CARTESIAN_POINT('Ctrl Pts',(3.01880316740535,-6.05632862685501,10.3442823748424));
#11245=CARTESIAN_POINT('Ctrl Pts',(3.18294597945007,-5.9745109330941,10.3528856816969));
#11246=CARTESIAN_POINT('Ctrl Pts',(3.34365589208657,-5.88606852315955,10.3614889885513));
#11247=CARTESIAN_POINT('Ctrl Pts',(3.50040945379159,-5.79132304882109,10.3700922954058));
#11248=CARTESIAN_POINT('Ctrl Pts',(3.66366207252199,-5.69264939426189,10.3790522983458));
#11249=CARTESIAN_POINT('Ctrl Pts',(3.82262296714999,-5.58713909241298,10.3880123012858));
#11250=CARTESIAN_POINT('Ctrl Pts',(3.97673666788187,-5.47520360117537,10.3969723042257));
#11251=CARTESIAN_POINT('Ctrl Pts',(4.12511995980998,-5.3674302066326,10.4055991474305));
#11252=CARTESIAN_POINT('Ctrl Pts',(4.26900982086606,-5.25370104216551,10.4142259906353));
#11253=CARTESIAN_POINT('Ctrl Pts',(4.40794602725427,-5.13442312444283,10.4228528338401));
#11254=CARTESIAN_POINT('Ctrl Pts',(4.54701502153511,-5.01503120718222,10.4314879221262));
#11255=CARTESIAN_POINT('Ctrl Pts',(4.68112068568571,-4.89008015654943,10.4401230104124));
#11256=CARTESIAN_POINT('Ctrl Pts',(4.80983962513759,-4.76001384246477,10.4487580986985));
#11257=CARTESIAN_POINT('Ctrl Pts',(4.9387497380463,-4.62975435380156,10.4574060118237));
#11258=CARTESIAN_POINT('Ctrl Pts',(5.06225693002524,-4.49436464221067,10.4660539249489));
#11259=CARTESIAN_POINT('Ctrl Pts',(5.17997706645217,-4.35432274768759,10.4747018380741));
#11260=CARTESIAN_POINT('Ctrl Pts',(5.19318347368377,-4.33861217900587,10.4756720022779));
#11261=CARTESIAN_POINT('Ctrl Pts',(5.20631709256602,-4.32284309161049,10.4766421664818));
#11262=CARTESIAN_POINT('Ctrl Pts',(5.21937741450869,-4.30701618349833,10.4776123306856));
#11263=CARTESIAN_POINT('Ctrl Pts',(5.33009780798819,-4.17284173500972,10.4858370102044));
#11264=CARTESIAN_POINT('Ctrl Pts',(5.43578695861546,-4.03421829462914,10.4940616897232));
#11265=CARTESIAN_POINT('Ctrl Pts',(5.53606876448858,-3.89155902368882,10.502286369242));
#11266=CARTESIAN_POINT('Ctrl Pts',(5.63624516283858,-3.74904970378168,10.5105024036921));
#11267=CARTESIAN_POINT('Ctrl Pts',(5.73102533033411,-3.60251329167313,10.5187184381423));
#11268=CARTESIAN_POINT('Ctrl Pts',(5.82007258227959,-3.45239686840858,10.5269344725924));
#11269=CARTESIAN_POINT('Ctrl Pts',(5.90904407181046,-3.30240816590409,10.535143516747));
#11270=CARTESIAN_POINT('Ctrl Pts',(5.99229217833759,-3.14884582507148,10.5433525609016));
#11271=CARTESIAN_POINT('Ctrl Pts',(6.06952276025712,-2.99218690303945,10.5515616050562));
#11272=CARTESIAN_POINT('Ctrl Pts',(6.14670309857145,-2.835629898005,10.5597653086843));
#11273=CARTESIAN_POINT('Ctrl Pts',(6.21787355229081,-2.67598064486513,10.5679690123123));
#11274=CARTESIAN_POINT('Ctrl Pts',(6.28278524535251,-2.51374194395146,10.5761727159403));
#11275=CARTESIAN_POINT('Ctrl Pts',(6.34766770467248,-2.35157630913816,10.5843727249343));
#11276=CARTESIAN_POINT('Ctrl Pts',(6.40629688610756,-2.18682388199999,10.5925727339283));
#11277=CARTESIAN_POINT('Ctrl Pts',(6.45847147158352,-2.02000872541228,10.6007727429222));
#11278=CARTESIAN_POINT('Ctrl Pts',(6.51064188506953,-1.85320690771652,10.6089720962262));
#11279=CARTESIAN_POINT('Ctrl Pts',(6.55635861538592,-1.68434302830992,10.6171714495301));
#11280=CARTESIAN_POINT('Ctrl Pts',(6.59546966923875,-1.51395800541219,10.6253708028341));
#11281=CARTESIAN_POINT('Ctrl Pts',(6.63458046809908,-1.34357409337446,10.6335701026807));
#11282=CARTESIAN_POINT('Ctrl Pts',(6.66708559501083,-1.17166940678454,10.6417694025272));
#11283=CARTESIAN_POINT('Ctrl Pts',(6.69288384741036,-0.998796678545469,
10.6499687023738));
#11284=CARTESIAN_POINT('Ctrl Pts',(6.71868661166906,-0.825893716576185,
10.6581694361968));
#11285=CARTESIAN_POINT('Ctrl Pts',(6.73778011155967,-0.652022730249603,
10.6663701700199));
#11286=CARTESIAN_POINT('Ctrl Pts',(6.75011484042284,-0.477743279495723,
10.6745709038429));
#11287=CARTESIAN_POINT('Ctrl Pts',(6.76245396417321,-0.303401732644257,
10.6827745596029));
#11288=CARTESIAN_POINT('Ctrl Pts',(6.76802949441791,-0.128651788846136,
10.6909782153628));
#11289=CARTESIAN_POINT('Ctrl Pts',(6.7668440233951,0.0459452178362025,10.6991818711228));
#11290=CARTESIAN_POINT('Ctrl Pts',(6.76565719433903,0.220742236613633,10.7073949246978));
#11291=CARTESIAN_POINT('Ctrl Pts',(6.7576938928307,0.395385609373892,10.7156079782729));
#11292=CARTESIAN_POINT('Ctrl Pts',(6.74300882202752,0.569316279460716,10.7238210318479));
#11293=CARTESIAN_POINT('Ctrl Pts',(6.72831506173848,0.743349868227267,10.732038945271));
#11294=CARTESIAN_POINT('Ctrl Pts',(6.70689164757387,0.916669558450377,10.7402568586941));
#11295=CARTESIAN_POINT('Ctrl Pts',(6.67884475052505,1.08872484971362,10.7484747721172));
#11296=CARTESIAN_POINT('Ctrl Pts',(6.65075410977755,1.261048489194,10.7567055027131));
#11297=CARTESIAN_POINT('Ctrl Pts',(6.61601941289762,1.43210343761496,10.7649362333091));
#11298=CARTESIAN_POINT('Ctrl Pts',(6.57479753177616,1.60135143430484,10.7731669639051));
#11299=CARTESIAN_POINT('Ctrl Pts',(6.53694016400921,1.75678547758949,10.7807259055809));
#11300=CARTESIAN_POINT('Ctrl Pts',(6.49361200355109,1.91069547167616,10.7882848472566));
#11301=CARTESIAN_POINT('Ctrl Pts',(6.44497042446897,2.06267913833449,10.7958437889324));
#11302=CARTESIAN_POINT('Ctrl Pts',(6.39249147917856,2.2266528965493,10.8039990604952));
#11303=CARTESIAN_POINT('Ctrl Pts',(6.33366470589249,2.38889122907565,10.8121543320579));
#11304=CARTESIAN_POINT('Ctrl Pts',(6.26862024425497,2.5488603793297,10.8203096036207));
#11305=CARTESIAN_POINT('Ctrl Pts',(6.20365726218112,2.70862914024645,10.8284546592796));
#11306=CARTESIAN_POINT('Ctrl Pts',(6.13249223341637,2.86613404240104,10.8365997149385));
#11307=CARTESIAN_POINT('Ctrl Pts',(6.05530549016273,3.02085491555042,10.8447447705973));
#11308=CARTESIAN_POINT('Ctrl Pts',(5.97601892578176,3.17978488140902,10.8531114078288));
#11309=CARTESIAN_POINT('Ctrl Pts',(5.89037843145591,3.33577681303247,10.8614780450603));
#11310=CARTESIAN_POINT('Ctrl Pts',(5.79863370633216,3.48828555880802,10.8698446822918));
#11311=CARTESIAN_POINT('Ctrl Pts',(5.70949954984256,3.63645471396822,10.8779732493705));
#11312=CARTESIAN_POINT('Ctrl Pts',(5.61460399167447,3.78133584760525,10.8861018164492));
#11313=CARTESIAN_POINT('Ctrl Pts',(5.51422380440614,3.92245138082305,10.8942303835279));
#11314=CARTESIAN_POINT('Ctrl Pts',(5.41389742076104,4.06349127633597,10.9023545937074));
#11315=CARTESIAN_POINT('Ctrl Pts',(5.30809247157963,4.20076929221523,10.9104788038868));
#11316=CARTESIAN_POINT('Ctrl Pts',(5.19712983400608,4.3338355400827,10.9186030140663));
#11317=CARTESIAN_POINT('Ctrl Pts',(5.08620554266485,4.46685580319922,10.9267244166985));
#11318=CARTESIAN_POINT('Ctrl Pts',(4.97012734613717,4.59566691608216,10.9348458193306));
#11319=CARTESIAN_POINT('Ctrl Pts',(4.84925728527732,4.71985092785618,10.9429672219628));
#11320=CARTESIAN_POINT('Ctrl Pts',(4.72840597956668,4.84401567026232,10.9510873644143));
#11321=CARTESIAN_POINT('Ctrl Pts',(4.60276454632192,4.96355448040034,10.9592075068658));
#11322=CARTESIAN_POINT('Ctrl Pts',(4.47273283158707,5.07808527077314,10.9673276493173));
#11323=CARTESIAN_POINT('Ctrl Pts',(4.34266559527193,5.19264734824135,10.9754500099991));
#11324=CARTESIAN_POINT('Ctrl Pts',(4.20820595494758,5.30219842961339,10.9835723706809));
#11325=CARTESIAN_POINT('Ctrl Pts',(4.06978813473268,5.40639561430618,10.9916947313627));
#11326=CARTESIAN_POINT('Ctrl Pts',(3.93134630479885,5.51061087286485,10.9998185009353));
#11327=CARTESIAN_POINT('Ctrl Pts',(3.78894522419705,5.60947017119006,11.0079422705079));
#11328=CARTESIAN_POINT('Ctrl Pts',(3.64304905248789,5.70267328550103,11.0160660400805));
#11329=CARTESIAN_POINT('Ctrl Pts',(3.49706115350793,5.79593499810972,11.0241949171978));
#11330=CARTESIAN_POINT('Ctrl Pts',(3.34757408948374,5.88353323843629,11.0323237943151));
#11331=CARTESIAN_POINT('Ctrl Pts',(3.19507795083086,5.9652129792753,11.0404526714324));
#11332=CARTESIAN_POINT('Ctrl Pts',(3.16324010823984,5.98226591421962,11.0421498023394));
#11333=CARTESIAN_POINT('Ctrl Pts',(3.13127118247908,5.99906103594538,11.0438469332463));
#11334=CARTESIAN_POINT('Ctrl Pts',(3.0991757505326,6.01559628526638,11.0455440641533));
#11335=CARTESIAN_POINT('Ctrl Pts',(3.09917575053258,6.01559628526639,9.04575158274221));
#11336=CARTESIAN_POINT('Ctrl Pts',(2.9338238445926,6.10078395293762,9.05450103065462));
#11337=CARTESIAN_POINT('Ctrl Pts',(2.76495772122974,6.17915010267054,9.06325047856703));
#11338=CARTESIAN_POINT('Ctrl Pts',(2.59315093316697,6.25042856433183,9.07199992647944));
#11339=CARTESIAN_POINT('Ctrl Pts',(2.42134553245612,6.32170645041453,9.08074930373944));
#11340=CARTESIAN_POINT('Ctrl Pts',(2.24659977927594,6.38589665313456,9.08949868099944));
#11341=CARTESIAN_POINT('Ctrl Pts',(2.06950718689932,6.44278115439071,9.09824805825945));
#11342=CARTESIAN_POINT('Ctrl Pts',(1.89241596572878,6.49966521519719,9.1069973677741));
#11343=CARTESIAN_POINT('Ctrl Pts',(1.71297821457217,6.54924360009541,9.11574667728875));
#11344=CARTESIAN_POINT('Ctrl Pts',(1.53180337335867,6.59134792173551,9.12449598680341));
#11345=CARTESIAN_POINT('Ctrl Pts',(1.35062987477799,6.63345193135302,9.13324523147953));
#11346=CARTESIAN_POINT('Ctrl Pts',(1.16771959102961,6.66808192368236,9.14199447615566));
#11347=CARTESIAN_POINT('Ctrl Pts',(0.983693746906862,6.69512028363168,9.15074372083179));
#11348=CARTESIAN_POINT('Ctrl Pts',(0.799669205419905,6.72215845218867,9.15949290357596));
#11349=CARTESIAN_POINT('Ctrl Pts',(0.614529402873525,6.74160505424579,9.16824208632014));
#11350=CARTESIAN_POINT('Ctrl Pts',(0.428903127363314,6.75339404354122,9.17699126906432));
#11351=CARTESIAN_POINT('Ctrl Pts',(0.243278104163857,6.7651829533033,9.18574039278293));
#11352=CARTESIAN_POINT('Ctrl Pts',(0.0571669005390063,6.76931433552276,
9.19448951650154));
#11353=CARTESIAN_POINT('Ctrl Pts',(-0.128798404777712,6.76577415902473,
9.20323864022015));
#11354=CARTESIAN_POINT('Ctrl Pts',(-0.314762517259244,6.76223400523441,
9.21198770781936));
#11355=CARTESIAN_POINT('Ctrl Pts',(-0.500580446819601,6.75102239665088,
9.22073677541857));
#11356=CARTESIAN_POINT('Ctrl Pts',(-0.685621118842648,6.73217741012497,
9.22948584301777));
#11357=CARTESIAN_POINT('Ctrl Pts',(-0.8706606654147,6.71333253821769,9.23823485740356));
#11358=CARTESIAN_POINT('Ctrl Pts',(-1.05492267885525,6.68685441030606,9.24698387178934));
#11359=CARTESIAN_POINT('Ctrl Pts',(-1.23778137635307,6.65283295028167,9.25573288617513));
#11360=CARTESIAN_POINT('Ctrl Pts',(-1.42999922978902,6.61707018861853,9.26492969654252));
#11361=CARTESIAN_POINT('Ctrl Pts',(-1.62066601233751,6.57297172934399,9.27412650690992));
#11362=CARTESIAN_POINT('Ctrl Pts',(-1.80906628500441,6.52070304311279,9.28332331727731));
#11363=CARTESIAN_POINT('Ctrl Pts',(-1.98831342545581,6.47097374915014,9.29207331501507));
#11364=CARTESIAN_POINT('Ctrl Pts',(-2.16550875896753,6.41384933989511,9.30082331275284));
#11365=CARTESIAN_POINT('Ctrl Pts',(-2.3400503671406,6.34952386240458,9.3095733104906));
#11366=CARTESIAN_POINT('Ctrl Pts',(-2.51458843547144,6.28519968948574,9.31832313077147));
#11367=CARTESIAN_POINT('Ctrl Pts',(-2.68647261718115,6.21367483971073,9.32707295105234));
#11368=CARTESIAN_POINT('Ctrl Pts',(-2.85511905908796,6.13519226743814,9.33582277133321));
#11369=CARTESIAN_POINT('Ctrl Pts',(-3.02376230488947,6.05671118252905,9.34457242579174));
#11370=CARTESIAN_POINT('Ctrl Pts',(-3.18916767379966,5.971272759926,9.35332208025027));
#11371=CARTESIAN_POINT('Ctrl Pts',(-3.35077334102847,5.87916720437963,9.3620717347088));
#11372=CARTESIAN_POINT('Ctrl Pts',(-3.51237616037431,5.78706327195605,9.37082123497725));
#11373=CARTESIAN_POINT('Ctrl Pts',(-3.67017916302367,5.68829258362255,9.37957073524569));
#11374=CARTESIAN_POINT('Ctrl Pts',(-3.82364636566533,5.58319061740994,9.38832023551414));
#11375=CARTESIAN_POINT('Ctrl Pts',(-3.97711106778862,5.47809036367655,9.39706959322257));
#11376=CARTESIAN_POINT('Ctrl Pts',(-4.12623987481985,5.3666592004318,9.40581895093101));
#11377=CARTESIAN_POINT('Ctrl Pts',(-4.27052628213981,5.24927559512293,9.41456830863944));
#11378=CARTESIAN_POINT('Ctrl Pts',(-4.41481053025038,5.13189374642985,9.42331753541596));
#11379=CARTESIAN_POINT('Ctrl Pts',(-4.55425230136597,5.00855981477292,9.43206676219249));
#11380=CARTESIAN_POINT('Ctrl Pts',(-4.68837800630622,4.87969268192005,9.44081598896901));
#11381=CARTESIAN_POINT('Ctrl Pts',(-4.82250188228976,4.75082730631727,9.44956509643986));
#11382=CARTESIAN_POINT('Ctrl Pts',(-4.95130963053055,4.61642907903431,9.45831420391071));
#11383=CARTESIAN_POINT('Ctrl Pts',(-5.07436379033463,4.47695444731581,9.46706331138156));
#11384=CARTESIAN_POINT('Ctrl Pts',(-5.19741643562904,4.33748153220469,9.47581231117131));
#11385=CARTESIAN_POINT('Ctrl Pts',(-5.31471544462873,4.19293255254462,9.48456131096106));
#11386=CARTESIAN_POINT('Ctrl Pts',(-5.42586245275729,4.04379841779467,9.49331031075081));
#11387=CARTESIAN_POINT('Ctrl Pts',(-5.53702160019251,3.89464799484203,9.50206026609297));
#11388=CARTESIAN_POINT('Ctrl Pts',(-5.64202723081347,3.74091164443706,9.51081022143512));
#11389=CARTESIAN_POINT('Ctrl Pts',(-5.74052265233059,3.58311159163086,9.51956017677728));
#11390=CARTESIAN_POINT('Ctrl Pts',(-5.83901427067006,3.42531763191634,9.52830979425973));
#11391=CARTESIAN_POINT('Ctrl Pts',(-5.93099603115823,3.26346052695461,9.53705941174218));
#11392=CARTESIAN_POINT('Ctrl Pts',(-6.01615550622833,3.09809004466923,9.54580902922462));
#11393=CARTESIAN_POINT('Ctrl Pts',(-6.1013121457888,2.93272506863661,9.55455835537572));
#11394=CARTESIAN_POINT('Ctrl Pts',(-6.17964682328829,2.76384720416714,9.56330768152682));
#11395=CARTESIAN_POINT('Ctrl Pts',(-6.25089348288644,2.59203002791399,9.57205700767793));
#11396=CARTESIAN_POINT('Ctrl Pts',(-6.32213814889404,2.42021765936835,9.58080608900949));
#11397=CARTESIAN_POINT('Ctrl Pts',(-6.38629508412653,2.24546640831724,9.58955517034106));
#11398=CARTESIAN_POINT('Ctrl Pts',(-6.44314639819874,2.06836976659848,9.59830425167263));
#11399=CARTESIAN_POINT('Ctrl Pts',(-6.50000285283759,1.89125711158074,9.60705412410703));
#11400=CARTESIAN_POINT('Ctrl Pts',(-6.54955227673304,1.71179891440046,9.61580399654143));
#11401=CARTESIAN_POINT('Ctrl Pts',(-6.59162635926435,1.53060476278214,9.62455386897583));
#11402=CARTESIAN_POINT('Ctrl Pts',(-6.63369752055242,1.34942319164472,9.63330313389833));
#11403=CARTESIAN_POINT('Ctrl Pts',(-6.66829431424295,1.16650618642473,9.64205239882083));
#11404=CARTESIAN_POINT('Ctrl Pts',(-6.69529923745452,0.982474997616181,
9.65080166374333));
#11405=CARTESIAN_POINT('Ctrl Pts',(-6.72230554731472,0.798434359175324,
9.65955137792304));
#11406=CARTESIAN_POINT('Ctrl Pts',(-6.74171916496725,0.61327970623788,9.66830109210274));
#11407=CARTESIAN_POINT('Ctrl Pts',(-6.75347414817291,0.427639953652885,
9.67705080628244));
#11408=CARTESIAN_POINT('Ctrl Pts',(-6.76248837758749,0.285283364196959,
9.6837604654583));
#11409=CARTESIAN_POINT('Ctrl Pts',(-6.76699999999996,0.142641701104389,
9.69047012463416));
#11410=CARTESIAN_POINT('Ctrl Pts',(-6.767,1.7245986591618E-12,9.69717978381002));
#11411=CARTESIAN_POINT('',(-6.76699881632875,0.00201345172301315,9.30282021618989));
#11412=CARTESIAN_POINT('Ctrl Pts',(3.09917575053261,6.01559628526638,8.65154848238438));
#11413=CARTESIAN_POINT('Ctrl Pts',(2.93648754800763,6.09941163926513,8.66016209671495));
#11414=CARTESIAN_POINT('Ctrl Pts',(2.77027489456604,6.17668648178732,8.66877571104552));
#11415=CARTESIAN_POINT('Ctrl Pts',(2.60107937308078,6.2471333501802,8.67738932537608));
#11416=CARTESIAN_POINT('Ctrl Pts',(2.43204707156897,6.31751225970581,8.6859946303029));
#11417=CARTESIAN_POINT('Ctrl Pts',(2.2600379194756,6.38107621066294,8.6945999352297));
#11418=CARTESIAN_POINT('Ctrl Pts',(2.08561650640442,6.4375843907644,8.70320524015651));
#11419=CARTESIAN_POINT('Ctrl Pts',(1.91140403447069,6.49402487915749,8.71180023670336));
#11420=CARTESIAN_POINT('Ctrl Pts',(1.73478535613973,6.54342636604349,8.72039523325021));
#11421=CARTESIAN_POINT('Ctrl Pts',(1.5563434826823,6.58559670522819,8.72899022979705));
#11422=CARTESIAN_POINT('Ctrl Pts',(1.4830144389203,6.60292621756527,8.73252226443504));
#11423=CARTESIAN_POINT('Ctrl Pts',(1.40937772352134,6.61903515919354,8.73605429907302));
#11424=CARTESIAN_POINT('Ctrl Pts',(1.3354746271782,6.6339126102296,8.739586333711));
#11425=CARTESIAN_POINT('Ctrl Pts',(1.15561990778682,6.67011920932695,8.74818209126553));
#11426=CARTESIAN_POINT('Ctrl Pts',(0.974397471948755,6.69898614923061,8.75677784882006));
#11427=CARTESIAN_POINT('Ctrl Pts',(0.792418247089899,6.72044361048279,8.76537360637459));
#11428=CARTESIAN_POINT('Ctrl Pts',(0.610269229423072,6.74192109227634,8.77397738406336));
#11429=CARTESIAN_POINT('Ctrl Pts',(0.4273623165183,6.75597526047728,8.78258116175212));
#11430=CARTESIAN_POINT('Ctrl Pts',(0.244311675476918,6.76258832143623,8.79118493944089));
#11431=CARTESIAN_POINT('Ctrl Pts',(0.0540669844083164,6.76946128146519,
8.80012685310539));
#11432=CARTESIAN_POINT('Ctrl Pts',(-0.136332583699432,6.76829642190302,
8.80906876676989));
#11433=CARTESIAN_POINT('Ctrl Pts',(-0.326201127095777,6.75913321548566,
8.81801068043438));
#11434=CARTESIAN_POINT('Ctrl Pts',(-0.509387232777708,6.75029250880971,
8.8266378827726));
#11435=CARTESIAN_POINT('Ctrl Pts',(-0.692078764494619,6.73400693969177,
8.83526508511082));
#11436=CARTESIAN_POINT('Ctrl Pts',(-0.873667647935661,6.7103646578223,8.84389228744904));
#11437=CARTESIAN_POINT('Ctrl Pts',(-1.0554294669953,6.68669986029789,8.85252770587705));
#11438=CARTESIAN_POINT('Ctrl Pts',(-1.23608624078694,6.65566441370846,8.86116312430507));
#11439=CARTESIAN_POINT('Ctrl Pts',(-1.41504049283352,6.61739747964723,8.86979854273309));
#11440=CARTESIAN_POINT('Ctrl Pts',(-1.59425912429878,6.57907401164133,8.87844671876188));
#11441=CARTESIAN_POINT('Ctrl Pts',(-1.77176991134944,6.53349777857669,8.88709489479067));
#11442=CARTESIAN_POINT('Ctrl Pts',(-1.94698948617415,6.48085804047021,8.89574307081946));
#11443=CARTESIAN_POINT('Ctrl Pts',(-1.96552705211969,6.47528895598018,8.89665801501792));
#11444=CARTESIAN_POINT('Ctrl Pts',(-1.98403899069124,6.4696408554876,8.89757295921638));
#11445=CARTESIAN_POINT('Ctrl Pts',(-2.00252462408755,6.46391399462609,8.89848790341484));
#11446=CARTESIAN_POINT('Ctrl Pts',(-2.1687234837376,6.4124254832967,8.90671389595549));
#11447=CARTESIAN_POINT('Ctrl Pts',(-2.33315341001072,6.35445537053403,8.91493988849615));
#11448=CARTESIAN_POINT('Ctrl Pts',(-2.49527320211393,6.29014313404807,8.9231658810368));
#11449=CARTESIAN_POINT('Ctrl Pts',(-2.65722303256971,6.22589832062947,8.93138324968752));
#11450=CARTESIAN_POINT('Ctrl Pts',(-2.81686722140321,6.15532475493372,8.93960061833823));
#11451=CARTESIAN_POINT('Ctrl Pts',(-2.97367894937343,6.07861188973711,8.94781798698894));
#11452=CARTESIAN_POINT('Ctrl Pts',(-3.13035765786271,6.00196409815229,8.95602838505062));
#11453=CARTESIAN_POINT('Ctrl Pts',(-3.28420837076711,5.91918753569112,8.96423878311229));
#11454=CARTESIAN_POINT('Ctrl Pts',(-3.43472342455742,5.83052004514147,8.97244918117397));
#11455=CARTESIAN_POINT('Ctrl Pts',(-3.58514090910781,5.74191003202974,8.98065425696203));
#11456=CARTESIAN_POINT('Ctrl Pts',(-3.73222673407548,5.64741687862983,8.9888593327501));
#11457=CARTESIAN_POINT('Ctrl Pts',(-3.87549698699058,5.54732476999742,8.99706440853817));
#11458=CARTESIAN_POINT('Ctrl Pts',(-4.01870302086423,5.44727752636066,9.00526580650692));
#11459=CARTESIAN_POINT('Ctrl Pts',(-4.15809659696912,5.34163653223326,9.01346720447568));
#11460=CARTESIAN_POINT('Ctrl Pts',(-4.29322192553541,5.23072982461358,9.02166860244444));
#11461=CARTESIAN_POINT('Ctrl Pts',(-4.42833666996081,5.11983180413074,9.02986935801142));
#11462=CARTESIAN_POINT('Ctrl Pts',(-4.55918355052281,5.00366911210476,9.0380701135784));
#11463=CARTESIAN_POINT('Ctrl Pts',(-4.68533879233318,4.88261092050738,9.04627086914538));
#11464=CARTESIAN_POINT('Ctrl Pts',(-4.81149339333496,4.76155334382798,9.05447158305643));
#11465=CARTESIAN_POINT('Ctrl Pts',(-4.93295614373756,4.63560056447028,9.06267229696747));
#11466=CARTESIAN_POINT('Ctrl Pts',(-5.0493392712357,4.50515947819352,9.07087301087851));
#11467=CARTESIAN_POINT('Ctrl Pts',(-5.16574289908355,4.37469541532263,9.07907516930739));
#11468=CARTESIAN_POINT('Ctrl Pts',(-5.27706488279496,4.23974173781979,9.08727732773627));
#11469=CARTESIAN_POINT('Ctrl Pts',(-5.38295694247679,4.10073939130993,9.09547948616514));
#11470=CARTESIAN_POINT('Ctrl Pts',(-5.48888684503592,3.96168736922706,9.10368457581734));
#11471=CARTESIAN_POINT('Ctrl Pts',(-5.58938274093627,3.81858408075926,9.11188966546954));
#11472=CARTESIAN_POINT('Ctrl Pts',(-5.6841389485791,3.67190051788526,9.12009475512174));
#11473=CARTESIAN_POINT('Ctrl Pts',(-5.77900340398618,3.52504938638302,9.12830921811878));
#11474=CARTESIAN_POINT('Ctrl Pts',(-5.8681148769155,3.37461011062403,9.13652368111582));
#11475=CARTESIAN_POINT('Ctrl Pts',(-5.9512125171873,3.22108034287772,9.14473814411286));
#11476=CARTESIAN_POINT('Ctrl Pts',(-6.03435939018455,3.06745961359652,9.1529574739196));
#11477=CARTESIAN_POINT('Ctrl Pts',(-6.11148517010585,2.91074506340614,9.16117680372633));
#11478=CARTESIAN_POINT('Ctrl Pts',(-6.18237673831163,2.75145540861254,9.16939613353307));
#11479=CARTESIAN_POINT('Ctrl Pts',(-6.25337814870437,2.59191894415619,9.17762819869303));
#11480=CARTESIAN_POINT('Ctrl Pts',(-6.31812591104038,2.42979973416161,9.18586026385298));
#11481=CARTESIAN_POINT('Ctrl Pts',(-6.37645602069225,2.26563404286252,9.19409232901294));
#11482=CARTESIAN_POINT('Ctrl Pts',(-6.42888731164545,2.11807013159255,9.20149190028279));
#11483=CARTESIAN_POINT('Ctrl Pts',(-6.47613395471416,1.96885309922747,9.20889147155265));
#11484=CARTESIAN_POINT('Ctrl Pts',(-6.51811212380928,1.81837931726316,9.2162910428225));
#11485=CARTESIAN_POINT('Ctrl Pts',(-6.57652369905974,1.60899880286983,9.22658736167982));
#11486=CARTESIAN_POINT('Ctrl Pts',(-6.62488316915981,1.39665633020682,9.23688368053714));
#11487=CARTESIAN_POINT('Ctrl Pts',(-6.66293320233366,1.18220562561667,9.24717999939447));
#11488=CARTESIAN_POINT('Ctrl Pts',(-6.7003504764938,0.971321162761626,9.25730509399726));
#11489=CARTESIAN_POINT('Ctrl Pts',(-6.72779836156197,0.758397917147425,
9.26743018860006));
#11490=CARTESIAN_POINT('Ctrl Pts',(-6.74507664073389,0.544270255136271,
9.27755528320285));
#11491=CARTESIAN_POINT('Ctrl Pts',(-6.7594480147814,0.366167523141684,9.28597692753186));
#11492=CARTESIAN_POINT('Ctrl Pts',(-6.7667845369513,0.187231905133603,9.29439857186088));
#11493=CARTESIAN_POINT('Ctrl Pts',(-6.76699532258635,0.00795638702641748,
9.30282021618989));
#11494=CARTESIAN_POINT('Ctrl Pts',(-6.767,1.50055999763773E-12,9.30282021618989));
#11495=CARTESIAN_POINT('Ctrl Pts',(-6.76700000000004,-0.186007249414152,
9.31156972799584));
#11496=CARTESIAN_POINT('Ctrl Pts',(-6.75932637295447,-0.372014355525981,
9.32031923980179));
#11497=CARTESIAN_POINT('Ctrl Pts',(-6.74400518266941,-0.557389537153473,
9.32906875160774));
#11498=CARTESIAN_POINT('Ctrl Pts',(-6.72868405709661,-0.742763935810001,
9.33781822645829));
#11499=CARTESIAN_POINT('Ctrl Pts',(-6.70571545653009,-0.927506129693821,
9.34656770130884));
#11500=CARTESIAN_POINT('Ctrl Pts',(-6.67517739415667,-1.11098863924872,
9.35531717615939));
#11501=CARTESIAN_POINT('Ctrl Pts',(-6.64463945823084,-1.29447038906588,
9.36406661478138));
#11502=CARTESIAN_POINT('Ctrl Pts',(-6.60653217027133,-1.47669218228329,
9.37281605340338));
#11503=CARTESIAN_POINT('Ctrl Pts',(-6.56098496116677,-1.65703510504258,
9.38156549202537));
#11504=CARTESIAN_POINT('Ctrl Pts',(-6.5154379368747,-1.83737729604189,9.39031489514562));
#11505=CARTESIAN_POINT('Ctrl Pts',(-6.46245112202578,-2.01584035397252,
9.39906429826587));
#11506=CARTESIAN_POINT('Ctrl Pts',(-6.40220448416164,-2.19181813638371,
9.40781370138612));
#11507=CARTESIAN_POINT('Ctrl Pts',(-6.34195808575096,-2.36779521936189,
9.4165630697314));
#11508=CARTESIAN_POINT('Ctrl Pts',(-6.27445201489129,-2.54128677545089,
9.42531243807668));
#11509=CARTESIAN_POINT('Ctrl Pts',(-6.19991555136063,-2.71170355238117,
9.43406180642196));
#11510=CARTESIAN_POINT('Ctrl Pts',(-6.1253793778891,-2.88211966613345,9.44281114071902));
#11511=CARTESIAN_POINT('Ctrl Pts',(-6.04381298133482,-3.04946076210713,
9.45156047501607));
#11512=CARTESIAN_POINT('Ctrl Pts',(-5.95549339426164,-3.21315848207118,
9.46030980931313));
#11513=CARTESIAN_POINT('Ctrl Pts',(-5.86717414355014,-3.37685557859891,
9.46905911028869));
#11514=CARTESIAN_POINT('Ctrl Pts',(-5.77210188986087,-3.53690907467557,
9.47780841126425));
#11515=CARTESIAN_POINT('Ctrl Pts',(-5.67059953466914,-3.69277536785142,
9.48655771223981));
#11516=CARTESIAN_POINT('Ctrl Pts',(-5.56909755761611,-3.84864108036016,
9.49530698062057));
#11517=CARTESIAN_POINT('Ctrl Pts',(-5.46116568337916,-4.00031938104489,
9.50405624900132));
#11518=CARTESIAN_POINT('Ctrl Pts',(-5.34717048685962,-4.14729511663415,
9.51280551738208));
#11519=CARTESIAN_POINT('Ctrl Pts',(-5.23317570555364,-4.29427031688228,
9.5215547538947));
#11520=CARTESIAN_POINT('Ctrl Pts',(-5.1131178217865,-4.43654275987308,9.53030399040731));
#11521=CARTESIAN_POINT('Ctrl Pts',(-4.98740459171859,-4.57362924147819,
9.53905322691993));
#11522=CARTESIAN_POINT('Ctrl Pts',(-4.86169180910671,-4.710715235146,9.54780243229105));
#11523=CARTESIAN_POINT('Ctrl Pts',(-4.73032391415269,-4.84261509316682,
9.55655163766216));
#11524=CARTESIAN_POINT('Ctrl Pts',(-4.59374707237128,-4.96888084331676,
9.56530084303328));
#11525=CARTESIAN_POINT('Ctrl Pts',(-4.45717070537247,-5.09514615452859,
9.5740500179895));
#11526=CARTESIAN_POINT('Ctrl Pts',(-4.31538563819366,-5.2157772025375,9.58279919294572));
#11527=CARTESIAN_POINT('Ctrl Pts',(-4.16887341290518,-5.33036429028752,
9.59154836790194));
#11528=CARTESIAN_POINT('Ctrl Pts',(-4.0223616847722,-5.44495098921263,9.60029751316984));
#11529=CARTESIAN_POINT('Ctrl Pts',(-3.87112305634334,-5.55349359238831,
9.60904665843776));
#11530=CARTESIAN_POINT('Ctrl Pts',(-3.71567117316642,-5.65562346102533,
9.61779580370566));
#11531=CARTESIAN_POINT('Ctrl Pts',(-3.56021980457225,-5.75775299158815,
9.62654492001182));
#11532=CARTESIAN_POINT('Ctrl Pts',(-3.40055544862328,-5.85346967275388,
9.63529403631797));
#11533=CARTESIAN_POINT('Ctrl Pts',(-3.23722036323359,-5.94244842803585,
9.64404315262413));
#11534=CARTESIAN_POINT('Ctrl Pts',(-3.07388580495981,-6.03142689616509,
9.65279224069508));
#11535=CARTESIAN_POINT('Ctrl Pts',(-2.90688079257619,-6.11366734484865,
9.66154132876604));
#11536=CARTESIAN_POINT('Ctrl Pts',(-2.73677251094504,-6.18889046787351,
9.670290416837));
#11537=CARTESIAN_POINT('Ctrl Pts',(-2.56666476416553,-6.26411335438307,
9.67903947739921));
#11538=CARTESIAN_POINT('Ctrl Pts',(-2.39345402972021,-6.33231884350317,
9.68778853796143));
#11539=CARTESIAN_POINT('Ctrl Pts',(-2.21772856473987,-6.39327529621061,
9.69653759852365));
#11540=CARTESIAN_POINT('Ctrl Pts',(-2.04200363768245,-6.45423156232089,
9.70528663230364));
#11541=CARTESIAN_POINT('Ctrl Pts',(-1.86376426620097,-6.50793874252054,
9.71403566608363));
#11542=CARTESIAN_POINT('Ctrl Pts',(-1.68361578194719,-6.55421443796115,
9.72278469986361));
#11543=CARTESIAN_POINT('Ctrl Pts',(-1.50346783419942,-6.60048999558662,
9.73153370758782));
#11544=CARTESIAN_POINT('Ctrl Pts',(-1.32141106257363,-6.63933404145471,
9.74028271531203));
#11545=CARTESIAN_POINT('Ctrl Pts',(-1.13806375959204,-6.67061465527003,
9.74903172303624));
#11546=CARTESIAN_POINT('Ctrl Pts',(-0.954716987420288,-6.70189517852466,
9.75778070543114));
#11547=CARTESIAN_POINT('Ctrl Pts',(-0.770079973810545,-6.72561226535821,
9.76652968782605));
#11548=CARTESIAN_POINT('Ctrl Pts',(-0.584779770552651,-6.7416853693978,
9.77527867022096));
#11549=CARTESIAN_POINT('Ctrl Pts',(-0.391490647554111,-6.75845143942393,
9.78440485089701));
#11550=CARTESIAN_POINT('Ctrl Pts',(-0.197480213104537,-6.76689975924026,
9.79353103157306));
#11551=CARTESIAN_POINT('Ctrl Pts',(-0.00346532629800411,-6.76699911271707,
9.80265721224912));
#11552=CARTESIAN_POINT('Ctrl Pts',(0.184486595295824,-6.76709536139774,
9.81149819977905));
#11553=CARTESIAN_POINT('Ctrl Pts',(0.372442378184971,-6.75935659726771,
9.82033918730897));
#11554=CARTESIAN_POINT('Ctrl Pts',(0.559750217721805,-6.74380965729019,
9.8291801748389));
#11555=CARTESIAN_POINT('Ctrl Pts',(0.745129914457424,-6.72842275717257,
9.83793015343666));
#11556=CARTESIAN_POINT('Ctrl Pts',(0.929874656313808,-6.70538772273478,
9.84668013203443));
#11557=CARTESIAN_POINT('Ctrl Pts',(1.11335688289735,-6.67478280180749,9.8554301106322));
#11558=CARTESIAN_POINT('Ctrl Pts',(1.29683723118809,-6.64417819418033,9.86417999965714));
#11559=CARTESIAN_POINT('Ctrl Pts',(1.47905480730182,-6.60600390230087,9.87292988868207));
#11560=CARTESIAN_POINT('Ctrl Pts',(1.6593906480475,-6.56038959797149,9.88167977770701));
#11561=CARTESIAN_POINT('Ctrl Pts',(1.83972470264205,-6.51477574543273,9.89042958006796));
#11562=CARTESIAN_POINT('Ctrl Pts',(2.01817678125786,-6.46172209820119,9.89917938242891));
#11563=CARTESIAN_POINT('Ctrl Pts',(2.19414072347616,-6.40140886724036,9.90792918478985));
#11564=CARTESIAN_POINT('Ctrl Pts',(2.37010298132039,-6.34109621361396,9.91667890339534));
#11565=CARTESIAN_POINT('Ctrl Pts',(2.54357687926861,-6.27352420825992,9.92542862200083));
#11566=CARTESIAN_POINT('Ctrl Pts',(2.71397317789925,-6.19892237325517,9.93417834060632));
#11567=CARTESIAN_POINT('Ctrl Pts',(2.88436790207162,-6.12432122756982,9.94292797836459));
#11568=CARTESIAN_POINT('Ctrl Pts',(3.05168482126224,-6.04269049717434,9.95167761612286));
#11569=CARTESIAN_POINT('Ctrl Pts',(3.21535561997362,-5.95430745234944,9.96042725388113));
#11570=CARTESIAN_POINT('Ctrl Pts',(3.37902496075256,-5.86592519481531,9.96917681370014));
#11571=CARTESIAN_POINT('Ctrl Pts',(3.53904799384852,-5.77079087940246,9.97792637351916));
#11572=CARTESIAN_POINT('Ctrl Pts',(3.69488118814964,-5.66922763747038,9.98667593333817));
#11573=CARTESIAN_POINT('Ctrl Pts',(3.85071304610807,-5.5676652664907,9.99542541812561));
#11574=CARTESIAN_POINT('Ctrl Pts',(4.00235489705936,-5.45967423580737,10.004174902913));
#11575=CARTESIAN_POINT('Ctrl Pts',(4.14929168607617,-5.34562133936357,10.0129243877005));
#11576=CARTESIAN_POINT('Ctrl Pts',(4.29622726385719,-5.23156938308562,10.0216738003638));
#11577=CARTESIAN_POINT('Ctrl Pts',(4.43845763092027,-5.11145583677237,10.0304232130271));
#11578=CARTESIAN_POINT('Ctrl Pts',(4.57549970660921,-4.98568866204249,10.0391726256904));
#11579=CARTESIAN_POINT('Ctrl Pts',(4.71254069815249,-4.85992248226205,10.0479219691367));
#11580=CARTESIAN_POINT('Ctrl Pts',(4.84439326931264,-4.72850295734053,10.056671312583));
#11581=CARTESIAN_POINT('Ctrl Pts',(4.97060959434645,-4.59187644221739,10.0654206560293));
#11582=CARTESIAN_POINT('Ctrl Pts',(5.09682496280464,-4.45525096256723,10.0741699331656));
#11583=CARTESIAN_POINT('Ctrl Pts',(5.21740397615789,-4.31341878218386,10.0829192103019));
#11584=CARTESIAN_POINT('Ctrl Pts',(5.33193710451886,-4.16686161438738,10.0916684874382));
#11585=CARTESIAN_POINT('Ctrl Pts',(5.44646940289332,-4.02030550864583,10.1004177011712));
#11586=CARTESIAN_POINT('Ctrl Pts',(5.5549557274961,-3.86902470980211,10.1091669149041));
#11587=CARTESIAN_POINT('Ctrl Pts',(5.65702762491399,-3.71353301465869,10.1179161286371));
#11588=CARTESIAN_POINT('Ctrl Pts',(5.75909881655102,-3.55804239466978,10.1266652818732));
#11589=CARTESIAN_POINT('Ctrl Pts',(5.85475551250734,-3.39834117619635,10.1354144351093));
#11590=CARTESIAN_POINT('Ctrl Pts',(5.94367283728051,-3.23497174692049,10.1441635883455));
#11591=CARTESIAN_POINT('Ctrl Pts',(6.03258957676271,-3.07160339301045,10.152912683991));
#11592=CARTESIAN_POINT('Ctrl Pts',(6.11476689685247,-2.90456712829582,10.1616617796365));
#11593=CARTESIAN_POINT('Ctrl Pts',(6.18992570525227,-2.73443024475981,10.1704108752821));
#11594=CARTESIAN_POINT('Ctrl Pts',(6.26508404388674,-2.56429442463088,10.1791599162431));
#11595=CARTESIAN_POINT('Ctrl Pts',(6.33322384283301,-2.39105828656032,10.1879089572041));
#11596=CARTESIAN_POINT('Ctrl Pts',(6.39411368720026,-2.21531017132101,10.1966579981652));
#11597=CARTESIAN_POINT('Ctrl Pts',(6.45500317120884,-2.03956309619534,10.2054069873476));
#11598=CARTESIAN_POINT('Ctrl Pts',(6.50864269270068,-1.86130434438651,10.21415597653));
#11599=CARTESIAN_POINT('Ctrl Pts',(6.55485008446329,-1.68113930719961,10.2229049657124));
#11600=CARTESIAN_POINT('Ctrl Pts',(6.60199664749401,-1.49731239211854,10.2318317792418));
#11601=CARTESIAN_POINT('Ctrl Pts',(6.64140563640904,-1.31150116499684,10.2407585927711));
#11602=CARTESIAN_POINT('Ctrl Pts',(6.6729377228217,-1.1243625515567,10.2496854063005));
#11603=CARTESIAN_POINT('Ctrl Pts',(6.7038449494987,-0.94093239505143,10.258435320456));
#11604=CARTESIAN_POINT('Ctrl Pts',(6.7271844934893,-0.756227260506783,10.2671852346115));
#11605=CARTESIAN_POINT('Ctrl Pts',(6.74287707373932,-0.570874564541741,
10.2759351487671));
#11606=CARTESIAN_POINT('Ctrl Pts',(6.7585693453867,-0.385525513632511,10.2846848908511));
#11607=CARTESIAN_POINT('Ctrl Pts',(6.76661493004103,-0.199529212418251,
10.293434632935));
#11608=CARTESIAN_POINT('Ctrl Pts',(6.76698649908907,-0.0135174386004342,
10.302184375019));
#11609=CARTESIAN_POINT('Ctrl Pts',(6.76735806132389,0.172490924445833,10.3109339566649));
#11610=CARTESIAN_POINT('Ctrl Pts',(6.76005588896289,0.358514472901523,10.3196835383108));
#11611=CARTESIAN_POINT('Ctrl Pts',(6.74510478454583,0.543921359662389,10.3284331199567));
#11612=CARTESIAN_POINT('Ctrl Pts',(6.73015393440686,0.729325093150645,10.3371825527958));
#11613=CARTESIAN_POINT('Ctrl Pts',(6.70755443556894,0.914111900256575,10.3459319856348));
#11614=CARTESIAN_POINT('Ctrl Pts',(6.67738304682315,1.09765415591563,10.3546814184738));
#11615=CARTESIAN_POINT('Ctrl Pts',(6.64721213111854,1.28119353391307,10.3634307141352));
#11616=CARTESIAN_POINT('Ctrl Pts',(6.60946960955485,1.46348811672696,10.3721800097965));
#11617=CARTESIAN_POINT('Ctrl Pts',(6.5642836699117,1.64391876348274,10.3809293054578));
#11618=CARTESIAN_POINT('Ctrl Pts',(6.51909837867704,1.82434682109763,10.3896784755687));
#11619=CARTESIAN_POINT('Ctrl Pts',(6.46646995271908,2.00291071820488,10.3984276456795));
#11620=CARTESIAN_POINT('Ctrl Pts',(6.40657713281536,2.17900400212742,10.4071768157903));
#11621=CARTESIAN_POINT('Ctrl Pts',(6.34668509279043,2.35509499309703,10.4159258719761));
#11622=CARTESIAN_POINT('Ctrl Pts',(6.27952894037506,2.52871516398173,10.4246749281619));
#11623=CARTESIAN_POINT('Ctrl Pts',(6.20533675061422,2.69927486771476,10.4334239843476));
#11624=CARTESIAN_POINT('Ctrl Pts',(6.12832117907892,2.87632521635975,10.4425059856299));
#11625=CARTESIAN_POINT('Ctrl Pts',(6.04372366626056,3.05007728920043,10.4515879869122));
#11626=CARTESIAN_POINT('Ctrl Pts',(5.95185378007846,3.21989527478237,10.4606699881944));
#11627=CARTESIAN_POINT('Ctrl Pts',(5.86334450817348,3.38350129286792,10.4694197685016));
#11628=CARTESIAN_POINT('Ctrl Pts',(5.76808562057231,3.54345567125002,10.4781695488087));
#11629=CARTESIAN_POINT('Ctrl Pts',(5.66640068804458,3.69921508465348,10.4869193291158));
#11630=CARTESIAN_POINT('Ctrl Pts',(5.56471941107895,3.85496889852324,10.4956687948693));
#11631=CARTESIAN_POINT('Ctrl Pts',(5.45661270815083,4.00652780919679,10.5044182606228));
#11632=CARTESIAN_POINT('Ctrl Pts',(5.3424477644908,4.15337704569273,10.5131677263763));
#11633=CARTESIAN_POINT('Ctrl Pts',(5.22828631819558,4.30022178356295,10.5219169240959));
#11634=CARTESIAN_POINT('Ctrl Pts',(5.10806717844028,4.44235690972726,10.5306661218155));
#11635=CARTESIAN_POINT('Ctrl Pts',(4.98219864544675,4.57929969070693,10.5394153195351));
#11636=CARTESIAN_POINT('Ctrl Pts',(4.8563332994399,4.71623900430036,10.5481642957253));
#11637=CARTESIAN_POINT('Ctrl Pts',(4.72481904033624,4.84798602483639,10.5569132719155));
#11638=CARTESIAN_POINT('Ctrl Pts',(4.58810250737186,4.97409332259137,10.5656622481058));
#11639=CARTESIAN_POINT('Ctrl Pts',(4.45137708685627,5.10020881822149,10.5744117930419));
#11640=CARTESIAN_POINT('Ctrl Pts',(4.30944892636032,5.22068366307949,10.5831613379781));
#11641=CARTESIAN_POINT('Ctrl Pts',(4.16280009466638,5.33510865604868,10.5919108829143));
#11642=CARTESIAN_POINT('Ctrl Pts',(4.01615988348775,5.44952692272901,10.6006599135226));
#11643=CARTESIAN_POINT('Ctrl Pts',(3.86479978232227,5.55789587288629,10.6094089441308));
#11644=CARTESIAN_POINT('Ctrl Pts',(3.70923383581073,5.65984746713874,10.6181579747391));
#11645=CARTESIAN_POINT('Ctrl Pts',(3.55366577799543,5.76180044505382,10.6269071240871));
#11646=CARTESIAN_POINT('Ctrl Pts',(3.39389200026838,5.8573357357106,10.6356562734352));
#11647=CARTESIAN_POINT('Ctrl Pts',(3.23045513626035,5.94612887621931,10.6444054227832));
#11648=CARTESIAN_POINT('Ctrl Pts',(3.18695122151575,5.9697639920669,10.6467342868961));
#11649=CARTESIAN_POINT('Ctrl Pts',(3.14318791262663,5.99292165435333,10.6490631510091));
#11650=CARTESIAN_POINT('Ctrl Pts',(3.09917575053259,6.01559628526639,10.6513920151221));
#11651=CARTESIAN_POINT('Origin',(0.,0.,-3.69717978381041));
#11652=CARTESIAN_POINT('',(3.09917575053261,6.01559628526638,13.045945719425));
#11653=CARTESIAN_POINT('',(3.09917575053257,6.0155962852664,12.6511155556306));
#11654=CARTESIAN_POINT('',(3.09917575053259,6.01559628526639,-3.69717978381041));
#11655=CARTESIAN_POINT('',(-6.76699833437543,-0.00474790060590539,11.6971797837751));
#11656=CARTESIAN_POINT('Ctrl Pts',(-6.76699833437491,-0.00474790134657525,
11.69717978381));
#11657=CARTESIAN_POINT('Ctrl Pts',(-6.76679660725303,-0.292261688620453,
11.7107429284341));
#11658=CARTESIAN_POINT('Ctrl Pts',(-6.74826864779524,-0.579070480480221,
11.7243060730581));
#11659=CARTESIAN_POINT('Ctrl Pts',(-6.71169741404573,-0.863369458743955,
11.7378692176821));
#11660=CARTESIAN_POINT('Ctrl Pts',(-6.70031069909056,-0.951887977143168,
11.7420921996791));
#11661=CARTESIAN_POINT('Ctrl Pts',(-6.6871750701465,-1.04016349819088,11.746315181676));
#11662=CARTESIAN_POINT('Ctrl Pts',(-6.67229977123769,-1.12814217310653,
11.7505381636729));
#11663=CARTESIAN_POINT('Ctrl Pts',(-6.64358823604027,-1.29795407651414,
11.7586891458472));
#11664=CARTESIAN_POINT('Ctrl Pts',(-6.60834472339372,-1.46693594567893,
11.7668401280215));
#11665=CARTESIAN_POINT('Ctrl Pts',(-6.5666250158011,-1.63454119001485,11.7749911101958));
#11666=CARTESIAN_POINT('Ctrl Pts',(-6.52495376951554,-1.80195174532542,
11.7831326242488));
#11667=CARTESIAN_POINT('Ctrl Pts',(-6.47682139022109,-1.96798850765806,
11.7912741383018));
#11668=CARTESIAN_POINT('Ctrl Pts',(-6.42233522229994,-2.13211146341031,
11.7994156523549));
#11669=CARTESIAN_POINT('Ctrl Pts',(-6.36790087922451,-2.29607831262788,
11.8075494225579));
#11670=CARTESIAN_POINT('Ctrl Pts',(-6.30712489355887,-2.45813463458681,
11.815683192761));
#11671=CARTESIAN_POINT('Ctrl Pts',(-6.24016531787777,-2.61775205196281,
11.8238169629641));
#11672=CARTESIAN_POINT('Ctrl Pts',(-6.17325534822217,-2.77725121910204,
11.831944707382));
#11673=CARTESIAN_POINT('Ctrl Pts',(-6.10017105095313,-2.93431474352113,
11.8400724518));
#11674=CARTESIAN_POINT('Ctrl Pts',(-6.02111982837664,-3.08843083334072,
11.848200196218));
#11675=CARTESIAN_POINT('Ctrl Pts',(-5.94211054982195,-3.24246515024876,
11.8563236281121));
#11676=CARTESIAN_POINT('Ctrl Pts',(-5.85714081766822,-3.39355482239924,
11.8644470600061));
#11677=CARTESIAN_POINT('Ctrl Pts',(-5.76646553451817,-3.54120943170749,
11.8725704919002));
#11678=CARTESIAN_POINT('Ctrl Pts',(-5.67521504303697,-3.68980070378044,
11.880745455651));
#11679=CARTESIAN_POINT('Ctrl Pts',(-5.57818651365921,-3.8349128373978,11.8889204194018));
#11680=CARTESIAN_POINT('Ctrl Pts',(-5.47568621780785,-3.97607211253885,
11.8970953831526));
#11681=CARTESIAN_POINT('Ctrl Pts',(-5.37385514939057,-4.11630975463763,
11.9052169723256));
#11682=CARTESIAN_POINT('Ctrl Pts',(-5.26662379139155,-4.25264571738984,
11.9133385614987));
#11683=CARTESIAN_POINT('Ctrl Pts',(-5.15433512035698,-4.38464576300693,
11.9214601506717));
#11684=CARTESIAN_POINT('Ctrl Pts',(-5.04203162491482,-4.51666323533733,
11.929582812061));
#11685=CARTESIAN_POINT('Ctrl Pts',(-4.92466972372092,-4.64434337155865,
11.9377054734504));
#11686=CARTESIAN_POINT('Ctrl Pts',(-4.8026316566751,-4.7672862479929,11.9458281348398));
#11687=CARTESIAN_POINT('Ctrl Pts',(-4.6805542384438,-4.8902687673685,11.953953415382));
#11688=CARTESIAN_POINT('Ctrl Pts',(-4.5537979095081,-5.00851072556508,11.9620786959243));
#11689=CARTESIAN_POINT('Ctrl Pts',(-4.42278057195902,-5.12165022354142,
11.9702039764665));
#11690=CARTESIAN_POINT('Ctrl Pts',(-4.29033582770329,-5.2360223528719,11.9784177802543));
#11691=CARTESIAN_POINT('Ctrl Pts',(-4.15353697598372,-5.34517993907141,
11.986631584042));
#11692=CARTESIAN_POINT('Ctrl Pts',(-4.01284791481315,-5.4487925830022,11.9948453878298));
#11693=CARTESIAN_POINT('Ctrl Pts',(-3.87343428221996,-5.5514659177504,12.002984728685));
#11694=CARTESIAN_POINT('Ctrl Pts',(-3.73020102221582,-5.64869428143773,
12.0111240695401));
#11695=CARTESIAN_POINT('Ctrl Pts',(-3.58362615654727,-5.74020143985473,
12.0192634103953));
#11696=CARTESIAN_POINT('Ctrl Pts',(-3.43503987597343,-5.83296433104378,
12.0275144456494));
#11697=CARTESIAN_POINT('Ctrl Pts',(-3.28301995323354,-5.91984766182591,
12.0357654809034));
#11698=CARTESIAN_POINT('Ctrl Pts',(-3.12808691313762,-6.00061340729906,
12.0440165161575));
#11699=CARTESIAN_POINT('Ctrl Pts',(-2.97315387304169,-6.08137915277221,
12.0522675514116));
#11700=CARTESIAN_POINT('Ctrl Pts',(-2.81530809128953,-6.15602720944744,
12.0605185866656));
#11701=CARTESIAN_POINT('Ctrl Pts',(-2.65508727394273,-6.22437149981807,
12.0687696219197));
#11702=CARTESIAN_POINT('Ctrl Pts',(-2.49524051503537,-6.29255623065688,
12.0770013939505));
#11703=CARTESIAN_POINT('Ctrl Pts',(-2.33253085409738,-6.35467961984619,
12.0852331659814));
#11704=CARTESIAN_POINT('Ctrl Pts',(-2.16745765985384,-6.41049267160808,
12.0934649380122));
#11705=CARTESIAN_POINT('Ctrl Pts',(-2.00258157950071,-6.46623907700853,
12.1016868804846));
#11706=CARTESIAN_POINT('Ctrl Pts',(-1.83534792177387,-6.51569003561539,
12.109908822957));
#11707=CARTESIAN_POINT('Ctrl Pts',(-1.66627804975084,-6.55864364491002,
12.1181307654294));
#11708=CARTESIAN_POINT('Ctrl Pts',(-1.49737618941545,-6.60155456943591,
12.1263445374193));
#11709=CARTESIAN_POINT('Ctrl Pts',(-1.32664209359358,-6.63798091548698,
12.1345583094092));
#11710=CARTESIAN_POINT('Ctrl Pts',(-1.15461447983466,-6.66776982228362,
12.1427720813991));
#11711=CARTESIAN_POINT('Ctrl Pts',(-0.982723362268644,-6.6975350929193,
12.1509793361294));
#11712=CARTESIAN_POINT('Ctrl Pts',(-0.809541122495328,-6.72067335318585,
12.1591865908598));
#11713=CARTESIAN_POINT('Ctrl Pts',(-0.635619022647368,-6.73708226594041,
12.1673938455901));
#11714=CARTESIAN_POINT('Ctrl Pts',(-0.461800097095261,-6.75348144457826,
12.1755962316021));
#11715=CARTESIAN_POINT('Ctrl Pts',(-0.287242541584296,-6.76315919466014,
12.183798617614));
#11716=CARTESIAN_POINT('Ctrl Pts',(-0.112505230085923,-6.76606470359273,
12.192001003626));
#11717=CARTESIAN_POINT('Ctrl Pts',(0.0621799265634823,-6.76896934530137,
12.2002009414247));
#11718=CARTESIAN_POINT('Ctrl Pts',(0.23704437457786,-6.76510576247856,12.2084008792234));
#11719=CARTESIAN_POINT('Ctrl Pts',(0.411526476122003,-6.75447518016393,
12.2166008170221));
#11720=CARTESIAN_POINT('Ctrl Pts',(0.585984180564948,-6.74384608427909,
12.2247996082578));
#11721=CARTESIAN_POINT('Ctrl Pts',(0.760059287329435,-6.72645189436287,
12.2329983994936));
#11722=CARTESIAN_POINT('Ctrl Pts',(0.933192499546701,-6.70234591458765,
12.2411971907293));
#11723=CARTESIAN_POINT('Ctrl Pts',(1.10633291053602,-6.67823893250068,12.2493963228658));
#11724=CARTESIAN_POINT('Ctrl Pts',(1.27853099392193,-6.64741965392924,12.2575954550022));
#11725=CARTESIAN_POINT('Ctrl Pts',(1.44923483975395,-6.60999299388762,12.2657945871386));
#11726=CARTESIAN_POINT('Ctrl Pts',(1.61997674979563,-6.57255798830329,12.2739955475495));
#11727=CARTESIAN_POINT('Ctrl Pts',(1.78922340862214,-6.5285127435271,12.2821965079604));
#11728=CARTESIAN_POINT('Ctrl Pts',(1.95643526729759,-6.47801281604739,12.2903974683713));
#11729=CARTESIAN_POINT('Ctrl Pts',(2.12380384373775,-6.42746555797872,12.2986061150564));
#11730=CARTESIAN_POINT('Ctrl Pts',(2.28913346618986,-6.37045163425554,12.3068147617414));
#11731=CARTESIAN_POINT('Ctrl Pts',(2.45190096910737,-6.30717612229834,12.3150234084265));
#11732=CARTESIAN_POINT('Ctrl Pts',(2.61474618180225,-6.24387040083458,12.32323597415));
#11733=CARTESIAN_POINT('Ctrl Pts',(2.77502650743805,-6.17429727330813,12.3314485398735));
#11734=CARTESIAN_POINT('Ctrl Pts',(2.93224088516228,-6.09870907581127,12.339661105597));
#11735=CARTESIAN_POINT('Ctrl Pts',(3.08967098369889,-6.02301716040001,12.3478849401458));
#11736=CARTESIAN_POINT('Ctrl Pts',(3.24402640969365,-5.9412938476673,12.3561087746945));
#11737=CARTESIAN_POINT('Ctrl Pts',(3.39483165528085,-5.85383694958299,12.3643326092433));
#11738=CARTESIAN_POINT('Ctrl Pts',(3.53339330817677,-5.77348051165853,12.3718887662177));
#11739=CARTESIAN_POINT('Ctrl Pts',(3.66895798881336,-5.68828431880963,12.3794449231921));
#11740=CARTESIAN_POINT('Ctrl Pts',(3.80118055163148,-5.59851010661753,12.3870010801665));
#11741=CARTESIAN_POINT('Ctrl Pts',(3.95246896479744,-5.4957908897434,12.3956467982189));
#11742=CARTESIAN_POINT('Ctrl Pts',(4.09972658582958,-5.38684383932133,12.4042925162713));
#11743=CARTESIAN_POINT('Ctrl Pts',(4.24243909134905,-5.27200147535957,12.4129382343236));
#11744=CARTESIAN_POINT('Ctrl Pts',(4.38496838309539,-5.15730654558895,12.421572853036));
#11745=CARTESIAN_POINT('Ctrl Pts',(4.52296395815918,-5.0367315843092,12.4302074717483));
#11746=CARTESIAN_POINT('Ctrl Pts',(4.6559410930395,-4.91065184452596,12.4388420904607));
#11747=CARTESIAN_POINT('Ctrl Pts',(4.79361446374846,-4.78011945811464,12.4477816503631));
#11748=CARTESIAN_POINT('Ctrl Pts',(4.92590817948129,-4.6436865385779,12.4567212102656));
#11749=CARTESIAN_POINT('Ctrl Pts',(5.05231999877382,-4.50181648115404,12.465660770168));
#11750=CARTESIAN_POINT('Ctrl Pts',(5.17408084126512,-4.36516614408195,12.4742714234385));
#11751=CARTESIAN_POINT('Ctrl Pts',(5.2903846176042,-4.22347185069932,12.482882076709));
#11752=CARTESIAN_POINT('Ctrl Pts',(5.40081814768467,-4.07718681637719,12.4914927299795));
#11753=CARTESIAN_POINT('Ctrl Pts',(5.51114714504044,-3.93104025062714,12.5000952326906));
#11754=CARTESIAN_POINT('Ctrl Pts',(5.61561679131165,-3.78031185019857,12.5086977354017));
#11755=CARTESIAN_POINT('Ctrl Pts',(5.71385338961835,-3.62548871766923,12.5173002381128));
#11756=CARTESIAN_POINT('Ctrl Pts',(5.81197942461125,-3.47083983545883,12.5258930588803));
#11757=CARTESIAN_POINT('Ctrl Pts',(5.90388624363981,-3.31210567202316,12.5344858796478));
#11758=CARTESIAN_POINT('Ctrl Pts',(5.98924267277715,-3.14980335998697,12.5430787004152));
#11759=CARTESIAN_POINT('Ctrl Pts',(5.99930231566164,-3.13067529529504,12.5440914033734));
#11760=CARTESIAN_POINT('Ctrl Pts',(6.00927102467809,-3.11149770383693,12.5451041063317));
#11761=CARTESIAN_POINT('Ctrl Pts',(6.01914829737112,-3.09227145869413,12.5461168092899));
#11762=CARTESIAN_POINT('Ctrl Pts',(6.10298107782584,-2.92908981553044,12.55471206705));
#11763=CARTESIAN_POINT('Ctrl Pts',(6.18012472976184,-2.76259324032409,12.56330732481));
#11764=CARTESIAN_POINT('Ctrl Pts',(6.25034575254777,-2.59335053041583,12.5719025825701));
#11765=CARTESIAN_POINT('Ctrl Pts',(6.32063253434351,-2.42394933188722,12.5805058894245));
#11766=CARTESIAN_POINT('Ctrl Pts',(6.38398363015338,-2.25179714760198,12.5891091962789));
#11767=CARTESIAN_POINT('Ctrl Pts',(6.44021471850249,-2.07748005515912,12.5977125031334));
#11768=CARTESIAN_POINT('Ctrl Pts',(6.49877716727391,-1.89593571561534,12.6066725060734));
#11769=CARTESIAN_POINT('Ctrl Pts',(6.54961652787162,-1.71204349383505,12.6156325090134));
#11770=CARTESIAN_POINT('Ctrl Pts',(6.59258318849465,-1.52647826803324,12.6245925119534));
#11771=CARTESIAN_POINT('Ctrl Pts',(6.63395222003498,-1.34781291290278,12.6332193551581));
#11772=CARTESIAN_POINT('Ctrl Pts',(6.66802344626706,-1.16759702429153,12.6418461983628));
#11773=CARTESIAN_POINT('Ctrl Pts',(6.69471625732958,-0.986439675726336,
12.6504730415676));
#11774=CARTESIAN_POINT('Ctrl Pts',(6.72143457997201,-0.805109186529252,
12.6591081298537));
#11775=CARTESIAN_POINT('Ctrl Pts',(6.74076037604901,-0.622835744093636,
12.6677432181398));
#11776=CARTESIAN_POINT('Ctrl Pts',(6.75266500716457,-0.440232099028653,
12.676378306426));
#11777=CARTESIAN_POINT('Ctrl Pts',(6.76458731904638,-0.257357250905425,
12.6850262195511));
#11778=CARTESIAN_POINT('Ctrl Pts',(6.76906642854844,-0.0741515248676813,
12.6936741326763));
#11779=CARTESIAN_POINT('Ctrl Pts',(6.76612574469661,0.10877227106996,12.7023220458014));
#11780=CARTESIAN_POINT('Ctrl Pts',(6.76579584473498,0.12929353629372,12.7032922100054));
#11781=CARTESIAN_POINT('Ctrl Pts',(6.76537261721316,0.149811258896166,12.7042623742094));
#11782=CARTESIAN_POINT('Ctrl Pts',(6.76485613579447,0.17032457839058,12.7052325384133));
#11783=CARTESIAN_POINT('Ctrl Pts',(6.76047760468728,0.344228622693202,12.7134572179321));
#11784=CARTESIAN_POINT('Ctrl Pts',(6.74938317409022,0.518192896016715,12.7216818974509));
#11785=CARTESIAN_POINT('Ctrl Pts',(6.731559778019,0.691658842896419,12.7299065769697));
#11786=CARTESIAN_POINT('Ctrl Pts',(6.71375511635345,0.864942457441293,12.7381226114198));
#11787=CARTESIAN_POINT('Ctrl Pts',(6.68923561020222,1.03772843500376,12.74633864587));
#11788=CARTESIAN_POINT('Ctrl Pts',(6.65804019558089,1.20945845485869,12.7545546803201));
#11789=CARTESIAN_POINT('Ctrl Pts',(6.62687132237308,1.38104236485982,12.7627637244747));
#11790=CARTESIAN_POINT('Ctrl Pts',(6.58903791666403,1.55157175580109,12.7709727686293));
#11791=CARTESIAN_POINT('Ctrl Pts',(6.54463069083944,1.72049356886983,12.7791818127839));
#11792=CARTESIAN_POINT('Ctrl Pts',(6.50025235485443,1.88930548711878,12.787385516412));
#11793=CARTESIAN_POINT('Ctrl Pts',(6.44930880837135,2.05651156530519,12.79558922004));
#11794=CARTESIAN_POINT('Ctrl Pts',(6.39194182025092,2.22156898756877,12.803792923668));
#11795=CARTESIAN_POINT('Ctrl Pts',(6.33460066802595,2.38655207428771,12.811992932662));
#11796=CARTESIAN_POINT('Ctrl Pts',(6.27084195498384,2.54938809510271,12.820192941656));
#11797=CARTESIAN_POINT('Ctrl Pts',(6.20085729943392,2.70954936328111,12.8283929506499));
#11798=CARTESIAN_POINT('Ctrl Pts',(6.13087824000474,2.86969782462654,12.8365923039539));
#11799=CARTESIAN_POINT('Ctrl Pts',(6.05467436508159,3.02717162767248,12.8447916572578));
#11800=CARTESIAN_POINT('Ctrl Pts',(5.97248558667473,3.18146270085988,12.8529910105618));
#11801=CARTESIAN_POINT('Ctrl Pts',(5.89029734411442,3.33575276811507,12.8611903104083));
#11802=CARTESIAN_POINT('Ctrl Pts',(5.80212444338723,3.48685982991059,12.8693896102549));
#11803=CARTESIAN_POINT('Ctrl Pts',(5.70825289195924,3.63430019693462,12.8775889101015));
#11804=CARTESIAN_POINT('Ctrl Pts',(5.6143649233254,3.78176634982049,12.8857896439245));
#11805=CARTESIAN_POINT('Ctrl Pts',(5.51477651090571,3.92556422788545,12.8939903777476));
#11806=CARTESIAN_POINT('Ctrl Pts',(5.40981717072618,4.0652388834257,12.9021911115706));
#11807=CARTESIAN_POINT('Ctrl Pts',(5.30482043333558,4.20496330530943,12.9103947673306));
#11808=CARTESIAN_POINT('Ctrl Pts',(5.19444917129497,4.34056129168992,12.9185984230905));
#11809=CARTESIAN_POINT('Ctrl Pts',(5.07907340035507,4.47161071581657,12.9268020788505));
#11810=CARTESIAN_POINT('Ctrl Pts',(4.9635654590525,4.60281026548321,12.9350151324255));
#11811=CARTESIAN_POINT('Ctrl Pts',(4.84304179239248,4.72945057342195,12.9432281860005));
#11812=CARTESIAN_POINT('Ctrl Pts',(4.7179102683927,4.85114540076823,12.9514412395756));
#11813=CARTESIAN_POINT('Ctrl Pts',(4.59270470126281,4.9729122376741,12.9596591529986));
#11814=CARTESIAN_POINT('Ctrl Pts',(4.46288610777912,5.08972752126063,12.9678770664217));
#11815=CARTESIAN_POINT('Ctrl Pts',(4.32889560573564,5.20124521962219,12.9760949798448));
#11816=CARTESIAN_POINT('Ctrl Pts',(4.19469612370625,5.31293684797637,12.9843257104408));
#11817=CARTESIAN_POINT('Ctrl Pts',(4.05631201387683,5.41931416084593,12.9925564410368));
#11818=CARTESIAN_POINT('Ctrl Pts',(3.91421464953569,5.52007361158891,13.0007871716328));
#11819=CARTESIAN_POINT('Ctrl Pts',(3.78371521490937,5.61260911649559,13.0083461133085));
#11820=CARTESIAN_POINT('Ctrl Pts',(3.65008444115707,5.70040679342884,13.0159050549843));
#11821=CARTESIAN_POINT('Ctrl Pts',(3.5137049190326,5.78326609641698,13.0234639966601));
#11822=CARTESIAN_POINT('Ctrl Pts',(3.37849875134788,5.86541251135917,13.0309579042484));
#11823=CARTESIAN_POINT('Ctrl Pts',(3.24020677386849,5.94293849593535,13.0384518118367));
#11824=CARTESIAN_POINT('Ctrl Pts',(3.09917575053261,6.01559628526638,13.045945719425));
#11825=CARTESIAN_POINT('Ctrl Pts',(3.0991757505326,6.01559628526638,11.0455440641533));
#11826=CARTESIAN_POINT('Ctrl Pts',(2.94526730765652,6.09488839386949,11.0536823803998));
#11827=CARTESIAN_POINT('Ctrl Pts',(2.78844847615828,6.16820072942692,11.0618206966463));
#11828=CARTESIAN_POINT('Ctrl Pts',(2.62923474293037,6.23533589043669,11.0699590128928));
#11829=CARTESIAN_POINT('Ctrl Pts',(2.46978442865988,6.30257080984081,11.0781094221373));
#11830=CARTESIAN_POINT('Ctrl Pts',(2.30793244489111,6.36361008803655,11.0862598313817));
#11831=CARTESIAN_POINT('Ctrl Pts',(2.14421045009698,6.41830589374602,11.0944102406261));
#11832=CARTESIAN_POINT('Ctrl Pts',(2.01253632167944,6.46229523405394,11.1009652428105));
#11833=CARTESIAN_POINT('Ctrl Pts',(1.8796529631955,6.50218241470288,11.1075202449948));
#11834=CARTESIAN_POINT('Ctrl Pts',(1.74584106724889,6.5379146497876,11.1140752471792));
#11835=CARTESIAN_POINT('Ctrl Pts',(1.57794102589216,6.58274955557868,11.1223001148568));
#11836=CARTESIAN_POINT('Ctrl Pts',(1.40807705294203,6.62117549259409,11.1305249825344));
#11837=CARTESIAN_POINT('Ctrl Pts',(1.23677946429998,6.65301928125012,11.138749850212));
#11838=CARTESIAN_POINT('Ctrl Pts',(1.06567486156505,6.68482719431392,11.1469654516555));
#11839=CARTESIAN_POINT('Ctrl Pts',(0.893140208782343,6.71006766024843,11.1551810530991));
#11840=CARTESIAN_POINT('Ctrl Pts',(0.719720638582738,6.72861733214173,11.1633966545426));
#11841=CARTESIAN_POINT('Ctrl Pts',(0.546461601468275,6.74714983275468,11.1716046508707));
#11842=CARTESIAN_POINT('Ctrl Pts',(0.372319632799995,6.75900383611599,11.1798126471989));
#11843=CARTESIAN_POINT('Ctrl Pts',(0.197849799874018,6.76410707016749,11.188020643527));
#11844=CARTESIAN_POINT('Ctrl Pts',(0.0235064290797352,6.76920660520784,
11.1962226903985));
#11845=CARTESIAN_POINT('Ctrl Pts',(-0.151163975458657,6.76756510683125,
11.2044247372699));
#11846=CARTESIAN_POINT('Ctrl Pts',(-0.325601393170112,6.75916213245146,
11.2126267841414));
#11847=CARTESIAN_POINT('Ctrl Pts',(-0.499947400840036,6.75076356146313,
11.2208245329129));
#11848=CARTESIAN_POINT('Ctrl Pts',(-0.674060307402147,6.73561059031559,
11.2290222816845));
#11849=CARTESIAN_POINT('Ctrl Pts',(-0.847380170823765,6.71373486563885,
11.237220030456));
#11850=CARTESIAN_POINT('Ctrl Pts',(-1.02066697696245,6.69186331331723,11.2454162156717));
#11851=CARTESIAN_POINT('Ctrl Pts',(-1.19316068488015,6.66327160021774,11.2536124008873));
#11852=CARTESIAN_POINT('Ctrl Pts',(-1.36430624382287,6.62804326125486,11.2618085861029));
#11853=CARTESIAN_POINT('Ctrl Pts',(-1.53543914180346,6.59281752840498,11.2700041649833));
#11854=CARTESIAN_POINT('Ctrl Pts',(-1.70522373779388,6.55095621892385,11.2781997438636));
#11855=CARTESIAN_POINT('Ctrl Pts',(-1.87311500420352,6.5025940347701,11.286395322744));
#11856=CARTESIAN_POINT('Ctrl Pts',(-2.04102439622373,6.45422662941494,11.2945917864224));
#11857=CARTESIAN_POINT('Ctrl Pts',(-2.20703970654683,6.39935705045834,11.3027882501009));
#11858=CARTESIAN_POINT('Ctrl Pts',(-2.3706308569867,6.33816995195794,11.3109847137793));
#11859=CARTESIAN_POINT('Ctrl Pts',(-2.53426943239221,6.27696511535841,11.3191835536071));
#11860=CARTESIAN_POINT('Ctrl Pts',(-2.69548211209535,6.20943923688715,11.3273823934349));
#11861=CARTESIAN_POINT('Ctrl Pts',(-2.85375854749797,6.13582522180858,11.3355812332627));
#11862=CARTESIAN_POINT('Ctrl Pts',(-3.01220030714001,6.06213431479708,11.343788637012));
#11863=CARTESIAN_POINT('Ctrl Pts',(-3.16769936923715,5.98234271779002,11.3519960407612));
#11864=CARTESIAN_POINT('Ctrl Pts',(-3.31976887326136,5.89672990971479,11.3602034445105));
#11865=CARTESIAN_POINT('Ctrl Pts',(-3.4719198337594,5.81107124288895,11.3684152445795));
#11866=CARTESIAN_POINT('Ctrl Pts',(-3.62063726863101,5.71958533672074,11.3766270446485));
#11867=CARTESIAN_POINT('Ctrl Pts',(-3.76546320619158,5.62259511638687,11.3848388447175));
#11868=CARTESIAN_POINT('Ctrl Pts',(-3.91050234776854,5.52546211289637,11.3930627337037));
#11869=CARTESIAN_POINT('Ctrl Pts',(-4.05163825293761,5.42280881245052,11.4012866226898));
#11870=CARTESIAN_POINT('Ctrl Pts',(-4.18844493344157,5.31499934520482,11.409510511676));
#11871=CARTESIAN_POINT('Ctrl Pts',(-4.31485194113688,5.21538526126131,11.417109242926));
#11872=CARTESIAN_POINT('Ctrl Pts',(-4.43756311217769,5.11136971193684,11.424707974176));
#11873=CARTESIAN_POINT('Ctrl Pts',(-4.55627102392818,5.00326726814714,11.432306705426));
#11874=CARTESIAN_POINT('Ctrl Pts',(-4.68269534251505,4.88813780801127,11.4403993793367));
#11875=CARTESIAN_POINT('Ctrl Pts',(-4.80495912097062,4.76802573065788,11.4484920532473));
#11876=CARTESIAN_POINT('Ctrl Pts',(-4.92263669390666,4.64326792031256,11.4565847271579));
#11877=CARTESIAN_POINT('Ctrl Pts',(-5.04018015380373,4.51865229210666,11.4646681781294));
#11878=CARTESIAN_POINT('Ctrl Pts',(-5.15314755820498,4.38940173596641,11.472751629101));
#11879=CARTESIAN_POINT('Ctrl Pts',(-5.26114657768875,4.25589305411614,11.4808350800725));
#11880=CARTESIAN_POINT('Ctrl Pts',(-5.36904598642814,4.1225075113392,11.488911075434));
#11881=CARTESIAN_POINT('Ctrl Pts',(-5.47198589985088,3.98487194762242,11.4969870707955));
#11882=CARTESIAN_POINT('Ctrl Pts',(-5.56961117993759,3.84339957645757,11.505063066157));
#11883=CARTESIAN_POINT('Ctrl Pts',(-5.66716307474747,3.70203355058679,11.5131329907636));
#11884=CARTESIAN_POINT('Ctrl Pts',(-5.75940808218336,3.55683676572979,11.5212029153701));
#11885=CARTESIAN_POINT('Ctrl Pts',(-5.84603177669574,3.40825490036524,11.5292728399766));
#11886=CARTESIAN_POINT('Ctrl Pts',(-5.93261980712226,3.25973420806001,11.5373394420917));
#11887=CARTESIAN_POINT('Ctrl Pts',(-6.01359094311208,3.10783152885777,11.5454060442068));
#11888=CARTESIAN_POINT('Ctrl Pts',(-6.08867442380893,2.95302095503147,11.5534726463219));
#11889=CARTESIAN_POINT('Ctrl Pts',(-6.16374173956836,2.79824371081665,11.5615375117552));
#11890=CARTESIAN_POINT('Ctrl Pts',(-6.2329237609722,2.64056015226075,11.5696023771884));
#11891=CARTESIAN_POINT('Ctrl Pts',(-6.29599604673013,2.48046825812358,11.5776672426217));
#11892=CARTESIAN_POINT('Ctrl Pts',(-6.35906714163235,2.3203793866507,11.5857319557837));
#11893=CARTESIAN_POINT('Ctrl Pts',(-6.41602859524056,2.15788261623926,11.5937966689458));
#11894=CARTESIAN_POINT('Ctrl Pts',(-6.46670445829191,1.99349503363001,11.6018613821078));
#11895=CARTESIAN_POINT('Ctrl Pts',(-6.51741120481266,1.8290072680427,11.6099310101605));
#11896=CARTESIAN_POINT('Ctrl Pts',(-6.56182459634185,1.66262674320034,11.6180006382131));
#11897=CARTESIAN_POINT('Ctrl Pts',(-6.59981868985138,1.49488536720662,11.6260702662658));
#11898=CARTESIAN_POINT('Ctrl Pts',(-6.63782396935663,1.3270946057916,11.6341422701305));
#11899=CARTESIAN_POINT('Ctrl Pts',(-6.66940611446372,1.15794255987394,11.6422142739952));
#11900=CARTESIAN_POINT('Ctrl Pts',(-6.6944905870027,0.987970030179167,11.6502862778599));
#11901=CARTESIAN_POINT('Ctrl Pts',(-6.71960330689822,0.817806096234619,
11.6583673715219));
#11902=CARTESIAN_POINT('Ctrl Pts',(-6.73820369187974,0.646820201885291,
11.6664484651839));
#11903=CARTESIAN_POINT('Ctrl Pts',(-6.75026915953388,0.475557855413853,
11.6745295588459));
#11904=CARTESIAN_POINT('Ctrl Pts',(-6.7615417903465,0.315549370105564,11.6820796338223));
#11905=CARTESIAN_POINT('Ctrl Pts',(-6.76711062799904,0.15529983985892,11.6896297087987));
#11906=CARTESIAN_POINT('Ctrl Pts',(-6.76699833437543,-0.0047479006059271,
11.6971797837751));
#11907=CARTESIAN_POINT('',(-6.76751319450492,-0.0015787245738949,11.3037082475646));
#11908=CARTESIAN_POINT('Ctrl Pts',(3.09917575053259,6.01559628526639,10.6513920151221));
#11909=CARTESIAN_POINT('Ctrl Pts',(2.93382384459261,6.10078395293761,10.6601414630345));
#11910=CARTESIAN_POINT('Ctrl Pts',(2.76495772122975,6.17915010267053,10.6688909109469));
#11911=CARTESIAN_POINT('Ctrl Pts',(2.59315093316697,6.25042856433183,10.6776403588593));
#11912=CARTESIAN_POINT('Ctrl Pts',(2.42134553245603,6.32170645041457,10.6863897361193));
#11913=CARTESIAN_POINT('Ctrl Pts',(2.24659977927576,6.38589665313462,10.6951391133793));
#11914=CARTESIAN_POINT('Ctrl Pts',(2.06950718689904,6.4427811543908,10.7038884906393));
#11915=CARTESIAN_POINT('Ctrl Pts',(1.89241596572852,6.49966521519726,10.712637800154));
#11916=CARTESIAN_POINT('Ctrl Pts',(1.71297821457194,6.54924360009547,10.7213871096686));
#11917=CARTESIAN_POINT('Ctrl Pts',(1.53180337335847,6.59134792173556,10.7301364191833));
#11918=CARTESIAN_POINT('Ctrl Pts',(1.35062987477783,6.63345193135305,10.7388856638594));
#11919=CARTESIAN_POINT('Ctrl Pts',(1.16771959102949,6.66808192368238,10.7476349085355));
#11920=CARTESIAN_POINT('Ctrl Pts',(0.983693746906791,6.69512028363169,10.7563841532117));
#11921=CARTESIAN_POINT('Ctrl Pts',(0.799669205419814,6.72215845218868,10.7651333359558));
#11922=CARTESIAN_POINT('Ctrl Pts',(0.614529402873416,6.7416050542458,10.7738825187));
#11923=CARTESIAN_POINT('Ctrl Pts',(0.428903127363185,6.75339404354122,10.7826317014442));
#11924=CARTESIAN_POINT('Ctrl Pts',(0.243278104163724,6.76518295330331,10.7913808251628));
#11925=CARTESIAN_POINT('Ctrl Pts',(0.0571669005388728,6.76931433552276,
10.8001299488814));
#11926=CARTESIAN_POINT('Ctrl Pts',(-0.128798404777849,6.76577415902472,
10.8088790726));
#11927=CARTESIAN_POINT('Ctrl Pts',(-0.314762517259335,6.7622340052344,10.8176281401992));
#11928=CARTESIAN_POINT('Ctrl Pts',(-0.500580446819649,6.75102239665088,
10.8263772077984));
#11929=CARTESIAN_POINT('Ctrl Pts',(-0.685621118842651,6.73217741012497,
10.8351262753976));
#11930=CARTESIAN_POINT('Ctrl Pts',(-0.870660665414531,6.71333253821771,
10.8438752897834));
#11931=CARTESIAN_POINT('Ctrl Pts',(-1.05492267885491,6.68685441030611,10.8526243041692));
#11932=CARTESIAN_POINT('Ctrl Pts',(-1.23778137635257,6.65283295028176,10.861373318555));
#11933=CARTESIAN_POINT('Ctrl Pts',(-1.42999922978852,6.61707018861864,10.8705701289224));
#11934=CARTESIAN_POINT('Ctrl Pts',(-1.62066601233702,6.57297172934411,10.8797669392898));
#11935=CARTESIAN_POINT('Ctrl Pts',(-1.80906628500392,6.52070304311292,10.8889637496572));
#11936=CARTESIAN_POINT('Ctrl Pts',(-1.98831342545534,6.47097374915028,10.8977137473949));
#11937=CARTESIAN_POINT('Ctrl Pts',(-2.16550875896709,6.41384933989526,10.9064637451327));
#11938=CARTESIAN_POINT('Ctrl Pts',(-2.34005036714018,6.34952386240473,10.9152137428704));
#11939=CARTESIAN_POINT('Ctrl Pts',(-2.51458843547101,6.28519968948591,10.9239635631513));
#11940=CARTESIAN_POINT('Ctrl Pts',(-2.68647261718072,6.21367483971092,10.9327133834322));
#11941=CARTESIAN_POINT('Ctrl Pts',(-2.85511905908752,6.13519226743834,10.9414632037131));
#11942=CARTESIAN_POINT('Ctrl Pts',(-3.02376230488894,6.05671118252932,10.9502128581716));
#11943=CARTESIAN_POINT('Ctrl Pts',(-3.18916767379903,5.97127275992633,10.9589625126301));
#11944=CARTESIAN_POINT('Ctrl Pts',(-3.35077334102776,5.87916720438003,10.9677121670886));
#11945=CARTESIAN_POINT('Ctrl Pts',(-3.51237616037357,5.7870632719565,10.9764616673571));
#11946=CARTESIAN_POINT('Ctrl Pts',(-3.67017916302288,5.68829258362306,10.9852111676255));
#11947=CARTESIAN_POINT('Ctrl Pts',(-3.82364636566451,5.5831906174105,10.993960667894));
#11948=CARTESIAN_POINT('Ctrl Pts',(-3.9771110677879,5.47809036367708,11.0027100256024));
#11949=CARTESIAN_POINT('Ctrl Pts',(-4.12623987481921,5.36665920043229,11.0114593833108));
#11950=CARTESIAN_POINT('Ctrl Pts',(-4.27052628213927,5.24927559512337,11.0202087410193));
#11951=CARTESIAN_POINT('Ctrl Pts',(-4.41481053024971,5.13189374643042,11.0289579677958));
#11952=CARTESIAN_POINT('Ctrl Pts',(-4.5542523013652,5.00855981477362,11.0377071945723));
#11953=CARTESIAN_POINT('Ctrl Pts',(-4.68837800630534,4.8796926819209,11.0464564213488));
#11954=CARTESIAN_POINT('Ctrl Pts',(-4.82250188228878,4.75082730631826,11.0552055288197));
#11955=CARTESIAN_POINT('Ctrl Pts',(-4.95130963052948,4.61642907903545,11.0639546362905));
#11956=CARTESIAN_POINT('Ctrl Pts',(-5.07436379033348,4.47695444731711,11.0727037437614));
#11957=CARTESIAN_POINT('Ctrl Pts',(-5.19741643562762,4.33748153220637,11.0814527435511));
#11958=CARTESIAN_POINT('Ctrl Pts',(-5.31471544462707,4.19293255254671,11.0902017433408));
#11959=CARTESIAN_POINT('Ctrl Pts',(-5.42586245275542,4.04379841779717,11.0989507431305));
#11960=CARTESIAN_POINT('Ctrl Pts',(-5.53702160019068,3.89464799484463,11.1077006984727));
#11961=CARTESIAN_POINT('Ctrl Pts',(-5.64202723081167,3.74091164443977,11.1164506538148));
#11962=CARTESIAN_POINT('Ctrl Pts',(-5.74052265232884,3.58311159163366,11.125200609157));
#11963=CARTESIAN_POINT('Ctrl Pts',(-5.83901427066841,3.42531763191915,11.1339502266394));
#11964=CARTESIAN_POINT('Ctrl Pts',(-5.93099603115669,3.26346052695742,11.1426998441219));
#11965=CARTESIAN_POINT('Ctrl Pts',(-6.01615550622689,3.09809004467203,11.1514494616043));
#11966=CARTESIAN_POINT('Ctrl Pts',(-6.1013121457874,2.93272506863952,11.1601987877554));
#11967=CARTESIAN_POINT('Ctrl Pts',(-6.17964682328694,2.76384720417015,11.1689481139065));
#11968=CARTESIAN_POINT('Ctrl Pts',(-6.25089348288515,2.59203002791711,11.1776974400576));
#11969=CARTESIAN_POINT('Ctrl Pts',(-6.32213814889292,2.42021765937131,11.1864465213892));
#11970=CARTESIAN_POINT('Ctrl Pts',(-6.38629508412556,2.24546640832003,11.1951956027208));
#11971=CARTESIAN_POINT('Ctrl Pts',(-6.4431463981979,2.0683697666011,11.2039446840524));
#11972=CARTESIAN_POINT('Ctrl Pts',(-6.50000285283682,1.89125711158338,11.2126945564868));
#11973=CARTESIAN_POINT('Ctrl Pts',(-6.54955227673235,1.71179891440311,11.2214444289212));
#11974=CARTESIAN_POINT('Ctrl Pts',(-6.59162635926374,1.5306047627848,11.2301943013556));
#11975=CARTESIAN_POINT('Ctrl Pts',(-6.63369752055189,1.34942319164735,11.2389435662781));
#11976=CARTESIAN_POINT('Ctrl Pts',(-6.66829431424249,1.16650618642733,11.2476928312006));
#11977=CARTESIAN_POINT('Ctrl Pts',(-6.69529923745415,0.982474997618738,
11.2564420961231));
#11978=CARTESIAN_POINT('Ctrl Pts',(-6.72230554731441,0.79843435917792,11.2651918103028));
#11979=CARTESIAN_POINT('Ctrl Pts',(-6.74171916496701,0.613279706240516,
11.2739415244825));
#11980=CARTESIAN_POINT('Ctrl Pts',(-6.75347414817274,0.427639953655554,
11.2826912386622));
#11981=CARTESIAN_POINT('Ctrl Pts',(-6.76248837758744,0.285283364198654,
11.2894008978381));
#11982=CARTESIAN_POINT('Ctrl Pts',(-6.76699999999997,0.142641701105099,
11.296110557014));
#11983=CARTESIAN_POINT('Ctrl Pts',(-6.767,1.45413500768681E-12,11.3028202161899));
#11984=CARTESIAN_POINT('Ctrl Pts',(-6.76699905057905,-0.0035846146663836,
11.3028202161899));
#11985=CARTESIAN_POINT('Ctrl Pts',(-6.76689717948375,-0.195895830608512,
11.3118251661962));
#11986=CARTESIAN_POINT('Ctrl Pts',(-6.75859330496265,-0.387925714519049,
11.3208301162025));
#11987=CARTESIAN_POINT('Ctrl Pts',(-6.74218372926967,-0.579005665577984,
11.3298350662088));
#11988=CARTESIAN_POINT('Ctrl Pts',(-6.72531576528353,-0.775423281318799,
11.3390915622477));
#11989=CARTESIAN_POINT('Ctrl Pts',(-6.69988280524364,-0.970836849582827,
11.3483480582867));
#11990=CARTESIAN_POINT('Ctrl Pts',(-6.66604400647577,-1.1645369482024,11.3576045543256));
#11991=CARTESIAN_POINT('Ctrl Pts',(-6.63287135500348,-1.35442388555294,
11.3666788278854));
#11992=CARTESIAN_POINT('Ctrl Pts',(-6.59162085975679,-1.54266400819156,
11.3757531014452));
#11993=CARTESIAN_POINT('Ctrl Pts',(-6.5424921374319,-1.72860800404308,11.384827375005));
#11994=CARTESIAN_POINT('Ctrl Pts',(-6.4918835681219,-1.92015297318757,11.3941749822836));
#11995=CARTESIAN_POINT('Ctrl Pts',(-6.43291490559951,-2.10926107711814,
11.4035225895621));
#11996=CARTESIAN_POINT('Ctrl Pts',(-6.36585668772188,-2.29524674738613,
11.4128701968406));
#11997=CARTESIAN_POINT('Ctrl Pts',(-6.29879846984425,-2.48123241765411,
11.4222178041192));
#11998=CARTESIAN_POINT('Ctrl Pts',(-6.22365085991296,-2.66409544755373,
11.4315654113977));
#11999=CARTESIAN_POINT('Ctrl Pts',(-6.1407351238976,-2.84317799972677,11.4409130186762));
#12000=CARTESIAN_POINT('Ctrl Pts',(-6.06839406204169,-2.99942122455524,
11.449068477083));
#12001=CARTESIAN_POINT('Ctrl Pts',(-5.98996799741044,-3.15315655311691,
11.4572239354898));
#12002=CARTESIAN_POINT('Ctrl Pts',(-5.90565223682026,-3.30387055704969,
11.4653793938966));
#12003=CARTESIAN_POINT('Ctrl Pts',(-5.82143909959385,-3.45440112222866,
11.4735249260385));
#12004=CARTESIAN_POINT('Ctrl Pts',(-5.7313507121931,-3.60191736723609,11.4816704581804));
#12005=CARTESIAN_POINT('Ctrl Pts',(-5.63563049261017,-3.74592551324269,
11.4898159903223));
#12006=CARTESIAN_POINT('Ctrl Pts',(-5.54000664907487,-3.88978866443002,
11.4979533211228));
#12007=CARTESIAN_POINT('Ctrl Pts',(-5.43876246296973,-4.03015044635292,
11.5060906519234));
#12008=CARTESIAN_POINT('Ctrl Pts',(-5.33218733651383,-4.16654139644881,
11.5142279827239));
#12009=CARTESIAN_POINT('Ctrl Pts',(-5.22569711829203,-4.30282368409123,
11.5223588305259));
#12010=CARTESIAN_POINT('Ctrl Pts',(-5.11388464032455,-4.43514115227457,
11.5304896783279));
#12011=CARTESIAN_POINT('Ctrl Pts',(-4.99708270305726,-4.56305308524961,
11.5386205261299));
#12012=CARTESIAN_POINT('Ctrl Pts',(-4.88034928543937,-4.69088998110619,
11.5467466041237));
#12013=CARTESIAN_POINT('Ctrl Pts',(-4.7586324833724,-4.81432621935578,11.5548726821175));
#12014=CARTESIAN_POINT('Ctrl Pts',(-4.63230547684412,-4.93295398004076,
11.5629987601113));
#12015=CARTESIAN_POINT('Ctrl Pts',(-4.50553053782335,-5.05200237309867,
11.5711536516935));
#12016=CARTESIAN_POINT('Ctrl Pts',(-4.37411287423625,-5.16620783683439,
11.5793085432757));
#12017=CARTESIAN_POINT('Ctrl Pts',(-4.23846754166975,-5.27519496305227,
11.5874634348579));
#12018=CARTESIAN_POINT('Ctrl Pts',(-4.10335117847325,-5.38375707758414,
11.5955865252142));
#12019=CARTESIAN_POINT('Ctrl Pts',(-3.96404035782896,-5.48714126357408,
11.6037096155705));
#12020=CARTESIAN_POINT('Ctrl Pts',(-3.82097874921737,-5.58501659782934,
11.6118327059268));
#12021=CARTESIAN_POINT('Ctrl Pts',(-3.67790590675518,-5.68289961770267,
11.6199564341452));
#12022=CARTESIAN_POINT('Ctrl Pts',(-3.53108199156581,-5.77527271758845,
11.6280801623636));
#12023=CARTESIAN_POINT('Ctrl Pts',(-3.38097978101672,-5.86184823416268,
11.6362038905821));
#12024=CARTESIAN_POINT('Ctrl Pts',(-3.23083722698936,-5.94844701993101,
11.6443298022424));
#12025=CARTESIAN_POINT('Ctrl Pts',(-3.07741493989091,-6.02924493694812,
11.6524557139027));
#12026=CARTESIAN_POINT('Ctrl Pts',(-2.9212103740452,-6.10400024169157,11.660581625563));
#12027=CARTESIAN_POINT('Ctrl Pts',(-2.76400686376333,-6.17923361437971,
11.6687595032731));
#12028=CARTESIAN_POINT('Ctrl Pts',(-2.60398570409236,-6.24834665812697,
11.6769373809832));
#12029=CARTESIAN_POINT('Ctrl Pts',(-2.4416736627962,-6.31114242624958,11.6851152586932));
#12030=CARTESIAN_POINT('Ctrl Pts',(-2.28013630166992,-6.37363848379047,
11.6932541051667));
#12031=CARTESIAN_POINT('Ctrl Pts',(-2.11633024476488,-6.42987737492793,
11.7013929516401));
#12032=CARTESIAN_POINT('Ctrl Pts',(-1.95078891128069,-6.47971539680751,
11.7095317981135));
#12033=CARTESIAN_POINT('Ctrl Pts',(-1.78405675493559,-6.52991192888239,
11.7177291914419));
#12034=CARTESIAN_POINT('Ctrl Pts',(-1.61556462809543,-6.57361506025311,
11.7259265847703));
#12035=CARTESIAN_POINT('Ctrl Pts',(-1.44586647194078,-6.61073060601607,
11.7341239780987));
#12036=CARTESIAN_POINT('Ctrl Pts',(-1.27616831578612,-6.64784615177903,
11.7423213714271));
#12037=CARTESIAN_POINT('Ctrl Pts',(-1.10526450749564,-6.67837410663854,
11.7505187647555));
#12038=CARTESIAN_POINT('Ctrl Pts',(-0.933712306061313,-6.70227351944918,
11.7587161580839));
#12039=CARTESIAN_POINT('Ctrl Pts',(-0.761557053204323,-6.72625694502547,
11.7669423674209));
#12040=CARTESIAN_POINT('Ctrl Pts',(-0.588236492379632,-6.74363664009532,
11.7751685767579));
#12041=CARTESIAN_POINT('Ctrl Pts',(-0.414298356368247,-6.75430572834178,
11.7833947860948));
#12042=CARTESIAN_POINT('Ctrl Pts',(-0.240555632401363,-6.76496283032465,
11.791611753638));
#12043=CARTESIAN_POINT('Ctrl Pts',(-0.0661970695429192,-6.76892431608196,
11.7998287211812));
#12044=CARTESIAN_POINT('Ctrl Pts',(0.108221009389168,-6.76613458431968,
11.8080456887244));
#12045=CARTESIAN_POINT('Ctrl Pts',(0.282478144187115,-6.76334742678001,
11.8162550740678));
#12046=CARTESIAN_POINT('Ctrl Pts',(0.456794329349758,-6.7538214640603,11.8244644594112));
#12047=CARTESIAN_POINT('Ctrl Pts',(0.63060964775381,-6.73755300329132,11.8326738447545));
#12048=CARTESIAN_POINT('Ctrl Pts',(0.804299453150475,-6.72129629006826,
11.8408773020551));
#12049=CARTESIAN_POINT('Ctrl Pts',(0.977488756561493,-6.69830680988572,
11.8490807593557));
#12050=CARTESIAN_POINT('Ctrl Pts',(1.1496190809913,-6.66863291601965,11.8572842166563));
#12051=CARTESIAN_POINT('Ctrl Pts',(1.32165963807766,-6.63897449732701,11.8654833957882));
#12052=CARTESIAN_POINT('Ctrl Pts',(1.49264196381272,-6.60263867041663,11.8736825749201));
#12053=CARTESIAN_POINT('Ctrl Pts',(1.66201404509435,-6.55972547549889,11.8818817540519));
#12054=CARTESIAN_POINT('Ctrl Pts',(1.83135421302534,-6.516820366352,11.8900793882817));
#12055=CARTESIAN_POINT('Ctrl Pts',(1.99908439203378,-6.46734043975449,11.8982770225116));
#12056=CARTESIAN_POINT('Ctrl Pts',(2.16466378273087,-6.41143663368307,11.9064746567414));
#12057=CARTESIAN_POINT('Ctrl Pts',(2.3302312217262,-6.35553686280959,11.914671699257));
#12058=CARTESIAN_POINT('Ctrl Pts',(2.49364784147683,-6.29321424981038,11.9228687417725));
#12059=CARTESIAN_POINT('Ctrl Pts',(2.65438905974009,-6.22466928595666,11.9310657842881));
#12060=CARTESIAN_POINT('Ctrl Pts',(2.81514788997328,-6.15611681182116,11.939263724931));
#12061=CARTESIAN_POINT('Ctrl Pts',(2.97323040470381,-6.08134076927961,11.9474616655738));
#12062=CARTESIAN_POINT('Ctrl Pts',(3.12813297720783,-6.00058939412662,11.9556596062166));
#12063=CARTESIAN_POINT('Ctrl Pts',(3.283080675345,-5.91981449478761,11.9638599350526));
#12064=CARTESIAN_POINT('Ctrl Pts',(3.43484626806414,-5.83306096131377,11.9720602638886));
#12065=CARTESIAN_POINT('Ctrl Pts',(3.58295161818903,-5.7406225012377,11.9802605927246));
#12066=CARTESIAN_POINT('Ctrl Pts',(3.73121129793195,-5.64808771788755,11.988469466516));
#12067=CARTESIAN_POINT('Ctrl Pts',(3.87580281047055,-5.54985636315848,11.9966783403074));
#12068=CARTESIAN_POINT('Ctrl Pts',(4.016277035931,-5.44626548844741,12.0048872140988));
#12069=CARTESIAN_POINT('Ctrl Pts',(4.15682665235861,-5.34261901765664,12.0131004935022));
#12070=CARTESIAN_POINT('Ctrl Pts',(4.29325429664768,-5.23360751637436,12.0213137729056));
#12071=CARTESIAN_POINT('Ctrl Pts',(4.42514483673317,-5.11960761913779,12.0295270523091));
#12072=CARTESIAN_POINT('Ctrl Pts',(4.557228287463,-5.00544097913396,12.0377523449245));
#12073=CARTESIAN_POINT('Ctrl Pts',(4.68476110986385,-4.88627160683936,12.04597763754));
#12074=CARTESIAN_POINT('Ctrl Pts',(4.80736496639999,-4.76251310547594,12.0542029301554));
#12075=CARTESIAN_POINT('Ctrl Pts',(4.91824542691824,-4.65058840741246,12.0616417192675));
#12076=CARTESIAN_POINT('Ctrl Pts',(5.02509484876144,-4.53491084447065,12.0690805083795));
#12077=CARTESIAN_POINT('Ctrl Pts',(5.12766282663466,-4.41580829932064,12.0765192974916));
#12078=CARTESIAN_POINT('Ctrl Pts',(5.24108784667101,-4.28409849232106,12.0847454985104));
#12079=CARTESIAN_POINT('Ctrl Pts',(5.34959346886797,-4.14783161111323,12.0929716995293));
#12080=CARTESIAN_POINT('Ctrl Pts',(5.45279312744014,-4.00741014987755,12.1011979005481));
#12081=CARTESIAN_POINT('Ctrl Pts',(5.55587686294633,-3.86714642255825,12.1094148611639));
#12082=CARTESIAN_POINT('Ctrl Pts',(5.65366629261492,-3.72273769443094,12.1176318217797));
#12083=CARTESIAN_POINT('Ctrl Pts',(5.74581329606023,-3.57462145783542,12.1258487823954));
#12084=CARTESIAN_POINT('Ctrl Pts',(5.83787528640367,-3.42664187050944,12.134058162197));
#12085=CARTESIAN_POINT('Ctrl Pts',(5.92430502940764,-3.27496188932745,12.1422675419986));
#12086=CARTESIAN_POINT('Ctrl Pts',(6.00479608888126,-3.12005014878869,12.1504769218002));
#12087=CARTESIAN_POINT('Ctrl Pts',(6.08522903882042,-2.96525024488351,12.1586803749406));
#12088=CARTESIAN_POINT('Ctrl Pts',(6.15973168022834,-2.80722354576659,12.166883828081));
#12089=CARTESIAN_POINT('Ctrl Pts',(6.22804210422755,-2.64646567103542,12.1750872812214));
#12090=CARTESIAN_POINT('Ctrl Pts',(6.29631691525374,-2.48579160585363,12.1832864575715));
#12091=CARTESIAN_POINT('Ctrl Pts',(6.35840580020133,-2.32238953095174,12.1914856339217));
#12092=CARTESIAN_POINT('Ctrl Pts',(6.41409379715271,-2.15677763372287,12.1996848102718));
#12093=CARTESIAN_POINT('Ctrl Pts',(6.46977131556704,-1.99119689887178,12.2078824438232));
#12094=CARTESIAN_POINT('Ctrl Pts',(6.51905022498551,-1.82340750754573,12.2160800773745));
#12095=CARTESIAN_POINT('Ctrl Pts',(6.56176442024781,-1.65394579511239,12.2242777109259));
#12096=CARTESIAN_POINT('Ctrl Pts',(6.60447553903973,-1.48449628808137,12.2324747540465));
#12097=CARTESIAN_POINT('Ctrl Pts',(6.64062279680041,-1.3133750474065,12.2406717971671));
#12098=CARTESIAN_POINT('Ctrl Pts',(6.6700905256658,-1.1411316223045,12.2488688402876));
#12099=CARTESIAN_POINT('Ctrl Pts',(6.69956148784204,-0.968869298001379,
12.2570667828188));
#12100=CARTESIAN_POINT('Ctrl Pts',(6.72235140047008,-0.795484897576925,
12.26526472535));
#12101=CARTESIAN_POINT('Ctrl Pts',(6.73839607959482,-0.621536221391113,
12.2734626678812));
#12102=CARTESIAN_POINT('Ctrl Pts',(6.75444543530706,-0.447536843898206,
12.2816629998897));
#12103=CARTESIAN_POINT('Ctrl Pts',(6.7637456084418,-0.272973220111627,12.2898633318981));
#12104=CARTESIAN_POINT('Ctrl Pts',(6.7662844448387,-0.0984063592142831,
12.2980636639065));
#12105=CARTESIAN_POINT('Ctrl Pts',(6.76882592738933,0.0763424475338137,
12.3062725428773));
#12106=CARTESIAN_POINT('Ctrl Pts',(6.76459198885875,0.251094139017972,12.314481421848));
#12107=CARTESIAN_POINT('Ctrl Pts',(6.7536226274409,0.425288615081848,12.3226903008188));
#12108=CARTESIAN_POINT('Ctrl Pts',(6.74264737741542,0.599576602780875,12.3309035865062));
#12109=CARTESIAN_POINT('Ctrl Pts',(6.72492953277396,0.773306422258561,12.3391168721936));
#12110=CARTESIAN_POINT('Ctrl Pts',(6.70056077573087,0.945925097847058,12.347330157881));
#12111=CARTESIAN_POINT('Ctrl Pts',(6.67615637019961,1.11879629328312,12.3555554585931));
#12112=CARTESIAN_POINT('Ctrl Pts',(6.64508167241789,1.29055274351432,12.3637807593051));
#12113=CARTESIAN_POINT('Ctrl Pts',(6.60747937158772,1.4606523727577,12.3720060600172));
#12114=CARTESIAN_POINT('Ctrl Pts',(6.57347262637041,1.61448696866093,12.3794448523112));
#12115=CARTESIAN_POINT('Ctrl Pts',(6.5341276476508,1.76696644063304,12.3868836446052));
#12116=CARTESIAN_POINT('Ctrl Pts',(6.4895843790117,1.91770268490382,12.3943224368992));
#12117=CARTESIAN_POINT('Ctrl Pts',(6.4407603161478,2.08292531204811,12.4024761282131));
#12118=CARTESIAN_POINT('Ctrl Pts',(6.38554598662076,2.24654062068834,12.4106298195269));
#12119=CARTESIAN_POINT('Ctrl Pts',(6.32406246397546,2.40801224077799,12.4187835108408));
#12120=CARTESIAN_POINT('Ctrl Pts',(6.26265194244936,2.56929214106243,12.4269275210471));
#12121=CARTESIAN_POINT('Ctrl Pts',(6.1949871753131,2.72843308152131,12.4350715312535));
#12122=CARTESIAN_POINT('Ctrl Pts',(6.12123964829143,2.88491146626461,12.4432155414599));
#12123=CARTESIAN_POINT('Ctrl Pts',(6.04756417639992,3.04123696357107,12.4513515945491));
#12124=CARTESIAN_POINT('Ctrl Pts',(5.96781793304699,3.194904756398,12.4594876476382));
#12125=CARTESIAN_POINT('Ctrl Pts',(5.8822213506837,3.34540894085623,12.4676237007274));
#12126=CARTESIAN_POINT('Ctrl Pts',(5.79669876936719,3.49578300952146,12.4757527199324));
#12127=CARTESIAN_POINT('Ctrl Pts',(5.70533610633201,3.64299860269472,12.4838817391374));
#12128=CARTESIAN_POINT('Ctrl Pts',(5.60840070748488,3.78657239522541,12.4920107583424));
#12129=CARTESIAN_POINT('Ctrl Pts',(5.51151178316446,3.93007735300498,12.5001358801856));
#12130=CARTESIAN_POINT('Ctrl Pts',(5.40905564570289,4.0699436835985,12.5082610020288));
#12131=CARTESIAN_POINT('Ctrl Pts',(5.30134427226658,4.20571491032218,12.516386123872));
#12132=CARTESIAN_POINT('Ctrl Pts',(5.19366404882027,4.34144687218257,12.5245088959405));
#12133=CARTESIAN_POINT('Ctrl Pts',(5.08073184271923,4.47308580225137,12.532631668009));
#12134=CARTESIAN_POINT('Ctrl Pts',(4.96290140266499,4.60020637226482,12.5407544400775));
#12135=CARTESIAN_POINT('Ctrl Pts',(4.84508262376716,4.72731436171888,12.5488764082712));
#12136=CARTESIAN_POINT('Ctrl Pts',(4.72236682569628,4.84990461439186,12.5569983764649));
#12137=CARTESIAN_POINT('Ctrl Pts',(4.5951462456726,4.96758693742556,12.5651203446587));
#12138=CARTESIAN_POINT('Ctrl Pts',(4.46787474726667,5.08531636127823,12.5732455635645));
#12139=CARTESIAN_POINT('Ctrl Pts',(4.33609513224914,5.19813368123317,12.5813707824703));
#12140=CARTESIAN_POINT('Ctrl Pts',(4.2002348556424,5.3056871522402,12.5894960013762));
#12141=CARTESIAN_POINT('Ctrl Pts',(4.06434482499791,5.41326417796179,12.5976229997431));
#12142=CARTESIAN_POINT('Ctrl Pts',(3.92437264431104,5.51557483790704,12.60574999811));
#12143=CARTESIAN_POINT('Ctrl Pts',(3.7807765139826,5.61230950245241,12.6138769964769));
#12144=CARTESIAN_POINT('Ctrl Pts',(3.6370642353945,5.709122411188,12.6220105683964));
#12145=CARTESIAN_POINT('Ctrl Pts',(3.48972246127582,5.80035012042969,12.6301441403159));
#12146=CARTESIAN_POINT('Ctrl Pts',(3.33923637653553,5.88572760341675,12.6382777122353));
#12147=CARTESIAN_POINT('Ctrl Pts',(3.26006178148752,5.93064689049492,12.6425569933671));
#12148=CARTESIAN_POINT('Ctrl Pts',(3.18001721780825,5.9739475603292,12.6468362744988));
#12149=CARTESIAN_POINT('Ctrl Pts',(3.09917575053257,6.0155962852664,12.6511155556306));
#12150=CARTESIAN_POINT('Origin',(0.,0.,-3.69717978381041));
#12151=CARTESIAN_POINT('',(3.09917575053257,6.0155962852664,15.0458593505058));
#12152=CARTESIAN_POINT('',(3.09917575053259,6.01559628526639,14.6513920151221));
#12153=CARTESIAN_POINT('',(3.09917575053259,6.01559628526639,-3.69717978381041));
#12154=CARTESIAN_POINT('',(-6.76699862985715,0.00430621776387394,13.697179783847));
#12155=CARTESIAN_POINT('Ctrl Pts',(-6.76699862985715,0.00430621776387394,
13.697179783847));
#12156=CARTESIAN_POINT('Ctrl Pts',(-6.76710791901341,-0.167436042203893,
13.7052923628463));
#12157=CARTESIAN_POINT('Ctrl Pts',(-6.76067498570166,-0.339425333033403,
13.7134049418455));
#12158=CARTESIAN_POINT('Ctrl Pts',(-6.74766992581323,-0.51111600667133,
13.7215175208448));
#12159=CARTESIAN_POINT('Ctrl Pts',(-6.73467774622239,-0.68263663672721,
13.729622065092));
#12160=CARTESIAN_POINT('Ctrl Pts',(-6.71512642437169,-0.853858873096928,
13.7377266093393));
#12161=CARTESIAN_POINT('Ctrl Pts',(-6.68903806257846,-1.02423571377715,
13.7458311535865));
#12162=CARTESIAN_POINT('Ctrl Pts',(-6.6629699464566,-1.19448033482812,13.7539294083648));
#12163=CARTESIAN_POINT('Ctrl Pts',(-6.63037494574035,-1.36388050322722,
13.7620276631432));
#12164=CARTESIAN_POINT('Ctrl Pts',(-6.59132708286434,-1.53189304022805,
13.7701259179215));
#12165=CARTESIAN_POINT('Ctrl Pts',(-6.55230115731951,-1.6998111867451,13.7782196230502));
#12166=CARTESIAN_POINT('Ctrl Pts',(-6.50682967182941,-1.86634289563401,
13.7863133281788));
#12167=CARTESIAN_POINT('Ctrl Pts',(-6.45503795771554,-2.03095395429135,
13.7944070333075));
#12168=CARTESIAN_POINT('Ctrl Pts',(-6.40325802058797,-2.19552758182253,
13.8024988979979));
#12169=CARTESIAN_POINT('Ctrl Pts',(-6.34516082144924,-2.35818107520942,
13.8105907626882));
#12170=CARTESIAN_POINT('Ctrl Pts',(-6.28092193695672,-2.51839405611112,
13.8186826273786));
#12171=CARTESIAN_POINT('Ctrl Pts',(-6.21668840886093,-2.67859367805907,
13.8267738173493));
#12172=CARTESIAN_POINT('Ctrl Pts',(-6.14631435157219,-2.83635284963488,
13.83486500732));
#12173=CARTESIAN_POINT('Ctrl Pts',(-6.0700239420726,-2.99117006247813,13.8429561972907));
#12174=CARTESIAN_POINT('Ctrl Pts',(-5.9937250956006,-3.14600439658946,13.8510482820678));
#12175=CARTESIAN_POINT('Ctrl Pts',(-5.91150875758756,-3.29789579299366,
13.8591403668449));
#12176=CARTESIAN_POINT('Ctrl Pts',(-5.82364557679827,-3.44636637574097,
13.867232451622));
#12177=CARTESIAN_POINT('Ctrl Pts',(-5.73575563432666,-3.59488218019017,
13.8753270011153));
#12178=CARTESIAN_POINT('Ctrl Pts',(-5.6422156132573,-3.73997477928341,13.8834215506086));
#12179=CARTESIAN_POINT('Ctrl Pts',(-5.54334002749553,-3.88119444753363,
13.8915161001018));
#12180=CARTESIAN_POINT('Ctrl Pts',(-5.44436299263744,-4.0225590110845,13.8996189548276));
#12181=CARTESIAN_POINT('Ctrl Pts',(-5.34003967278028,-4.16004240580135,
13.9077218095534));
#12182=CARTESIAN_POINT('Ctrl Pts',(-5.23072596280807,-4.29322663063641,
13.9158246642792));
#12183=CARTESIAN_POINT('Ctrl Pts',(-5.12134985217798,-4.42648688237833,
13.9239321444401));
#12184=CARTESIAN_POINT('Ctrl Pts',(-5.00697792077875,-4.5554427997631,13.9320396246009));
#12185=CARTESIAN_POINT('Ctrl Pts',(-4.88800332975851,-4.67971285959616,
13.9401471047618));
#12186=CARTESIAN_POINT('Ctrl Pts',(-4.76886601445183,-4.80415288645025,
13.9482656737098));
#12187=CARTESIAN_POINT('Ctrl Pts',(-4.64511373259073,-4.92389400117209,
13.9563842426579));
#12188=CARTESIAN_POINT('Ctrl Pts',(-4.51717380191012,-5.03859403438468,
13.964502811606));
#12189=CARTESIAN_POINT('Ctrl Pts',(-4.44544148123866,-5.10290311693352,
13.9690546648709));
#12190=CARTESIAN_POINT('Ctrl Pts',(-4.37239332102361,-5.16562827586466,
13.9736065181357));
#12191=CARTESIAN_POINT('Ctrl Pts',(-4.29810856065524,-5.22671520180908,
13.9781583714006));
#12192=CARTESIAN_POINT('Ctrl Pts',(-4.16508719060017,-5.33610327200389,
13.9863093535749));
#12193=CARTESIAN_POINT('Ctrl Pts',(-4.02767819514069,-5.44058171598578,
13.9944603357492));
#12194=CARTESIAN_POINT('Ctrl Pts',(-3.88628208341779,-5.5397744149113,14.0026113179234));
#12195=CARTESIAN_POINT('Ctrl Pts',(-3.74505021638349,-5.63885189232368,
14.0107528319765));
#12196=CARTESIAN_POINT('Ctrl Pts',(-3.59984074856104,-5.73265563871572,
14.0188943460295));
#12197=CARTESIAN_POINT('Ctrl Pts',(-3.45108880764441,-5.8208483094607,14.0270358600825));
#12198=CARTESIAN_POINT('Ctrl Pts',(-3.30247835302977,-5.90895709521723,
14.0351696302856));
#12199=CARTESIAN_POINT('Ctrl Pts',(-3.15033244579128,-5.99146524530517,
14.0433034004886));
#12200=CARTESIAN_POINT('Ctrl Pts',(-2.99511687030795,-6.06807744950546,
14.0514371706917));
#12201=CARTESIAN_POINT('Ctrl Pts',(-2.84001628402086,-6.14463289667118,
14.0595649151097));
#12202=CARTESIAN_POINT('Ctrl Pts',(-2.68185088416405,-6.21530093398868,
14.0676926595276));
#12203=CARTESIAN_POINT('Ctrl Pts',(-2.52111284102055,-6.27983113171376,
14.0758204039456));
#12204=CARTESIAN_POINT('Ctrl Pts',(-2.36046008435082,-6.34432709017035,
14.0839438358396));
#12205=CARTESIAN_POINT('Ctrl Pts',(-2.19723774149744,-6.40269155886517,
14.0920672677336));
#12206=CARTESIAN_POINT('Ctrl Pts',(-2.03195983261033,-6.45472139124984,
14.1001906996277));
#12207=CARTESIAN_POINT('Ctrl Pts',(-1.86563346567688,-6.50708128042661,
14.1083656633785));
#12208=CARTESIAN_POINT('Ctrl Pts',(-1.6972257023513,-6.55302572609678,14.1165406271293));
#12209=CARTESIAN_POINT('Ctrl Pts',(-1.5272783993263,-6.59239787110512,14.1247155908801));
#12210=CARTESIAN_POINT('Ctrl Pts',(-1.35844068722097,-6.63151295422539,
14.1328371800532));
#12211=CARTESIAN_POINT('Ctrl Pts',(-1.18808384551203,-6.66414124503068,
14.1409587692262));
#12212=CARTESIAN_POINT('Ctrl Pts',(-1.01675155659607,-6.69017976381498,
14.1490803583992));
#12213=CARTESIAN_POINT('Ctrl Pts',(-0.84539664830377,-6.71622172021784,
14.1572030197886));
#12214=CARTESIAN_POINT('Ctrl Pts',(-0.673066398166757,-6.73567211674775,
14.165325681178));
#12215=CARTESIAN_POINT('Ctrl Pts',(-0.500311634498783,-6.74847962643329,
14.1734483425673));
#12216=CARTESIAN_POINT('Ctrl Pts',(-0.32750116604283,-6.76129126590139,
14.1815736231096));
#12217=CARTESIAN_POINT('Ctrl Pts',(-0.15426627627263,-6.76745572610162,
14.1896989036518));
#12218=CARTESIAN_POINT('Ctrl Pts',(0.018840212519595,-6.76697377314204,
14.197824184194));
#12219=CARTESIAN_POINT('Ctrl Pts',(0.193832660588631,-6.76648656940497,
14.2060379879818));
#12220=CARTESIAN_POINT('Ctrl Pts',(0.36869350937776,-6.75920728251903,14.2142517917696));
#12221=CARTESIAN_POINT('Ctrl Pts',(0.542855862123635,-6.74519062095046,
14.2224655955574));
#12222=CARTESIAN_POINT('Ctrl Pts',(0.715439331337447,-6.73130102861227,
14.2306049364125));
#12223=CARTESIAN_POINT('Ctrl Pts',(0.887336562306852,-6.71079582288724,
14.2387442772677));
#12224=CARTESIAN_POINT('Ctrl Pts',(1.05800550951591,-6.68377986934294,14.2468836181229));
#12225=CARTESIAN_POINT('Ctrl Pts',(1.23101650945525,-6.65639318176182,14.255134653377));
#12226=CARTESIAN_POINT('Ctrl Pts',(1.40276488520187,-6.62231583582359,14.263385688631));
#12227=CARTESIAN_POINT('Ctrl Pts',(1.57270155325428,-6.58170941506776,14.2716367238851));
#12228=CARTESIAN_POINT('Ctrl Pts',(1.74263822130669,-6.54110299431192,14.2798877591392));
#12229=CARTESIAN_POINT('Ctrl Pts',(1.91076283014249,-6.49396766694165,14.2881387943933));
#12230=CARTESIAN_POINT('Ctrl Pts',(2.07654738497298,-6.44051550405415,14.2963898296474));
#12231=CARTESIAN_POINT('Ctrl Pts',(2.24194489202171,-6.38718813289467,14.3046216016782));
#12232=CARTESIAN_POINT('Ctrl Pts',(2.40552965522928,-6.3274070782602,14.3128533737091));
#12233=CARTESIAN_POINT('Ctrl Pts',(2.56676137122036,-6.26131176856823,14.3210851457399));
#12234=CARTESIAN_POINT('Ctrl Pts',(2.72780056043021,-6.19529538328112,14.3293070882123));
#12235=CARTESIAN_POINT('Ctrl Pts',(2.88649196906151,-6.12297989109231,14.3375290306847));
#12236=CARTESIAN_POINT('Ctrl Pts',(3.04230956560976,-6.04455469881772,14.3457509731571));
#12237=CARTESIAN_POINT('Ctrl Pts',(3.19797231980186,-5.96620744088317,14.353964745147));
#12238=CARTESIAN_POINT('Ctrl Pts',(3.35076663142432,-5.88176273412973,14.3621785171369));
#12239=CARTESIAN_POINT('Ctrl Pts',(3.50018552170184,-5.79145839263901,14.3703922891268));
#12240=CARTESIAN_POINT('Ctrl Pts',(3.64948585479403,-5.70122570359151,14.3785995438572));
#12241=CARTESIAN_POINT('Ctrl Pts',(3.79541579575059,-5.60514282481725,14.3868067985876));
#12242=CARTESIAN_POINT('Ctrl Pts',(3.93749202181478,-5.50349394277353,14.3950140533179));
#12243=CARTESIAN_POINT('Ctrl Pts',(4.07948396523469,-5.4019053610123,14.4032164393299));
#12244=CARTESIAN_POINT('Ctrl Pts',(4.21762645732611,-5.29475756163349,14.4114188253419));
#12245=CARTESIAN_POINT('Ctrl Pts',(4.35146421202563,-5.18237862486524,14.4196212113539));
#12246=CARTESIAN_POINT('Ctrl Pts',(4.48526201940106,-5.07003323048434,14.4278211491526));
#12247=CARTESIAN_POINT('Ctrl Pts',(4.61475737221627,-4.95246003604422,14.4360210869513));
#12248=CARTESIAN_POINT('Ctrl Pts',(4.73952701790977,-4.83002822419324,14.44422102475));
#12249=CARTESIAN_POINT('Ctrl Pts',(4.86427921758664,-4.70761353146938,14.4524198159858));
#12250=CARTESIAN_POINT('Ctrl Pts',(4.98430676985345,-4.58034182473609,14.4606186072215));
#12251=CARTESIAN_POINT('Ctrl Pts',(5.09922233718302,-4.44862007323325,14.4688173984573));
#12252=CARTESIAN_POINT('Ctrl Pts',(5.21414268263058,-4.31689284482169,14.4770165305937));
#12253=CARTESIAN_POINT('Ctrl Pts',(5.32395038398178,-4.18071547306964,14.4852156627301));
#12254=CARTESIAN_POINT('Ctrl Pts',(5.42829752155873,-4.04052905167621,14.4934147948665));
#12255=CARTESIAN_POINT('Ctrl Pts',(5.53266792686751,-3.90031137096761,14.5016157552774));
#12256=CARTESIAN_POINT('Ctrl Pts',(5.63157512928682,-3.75608314758275,14.5098167156883));
#12257=CARTESIAN_POINT('Ctrl Pts',(5.7247137470009,-3.60831560633198,14.5180176760992));
#12258=CARTESIAN_POINT('Ctrl Pts',(5.81793965802138,-3.46040957132243,14.5262263227842));
#12259=CARTESIAN_POINT('Ctrl Pts',(5.90538599100199,-3.30895789451858,14.5344349694692));
#12260=CARTESIAN_POINT('Ctrl Pts',(5.98679220429685,-3.15445844838231,14.5426436161543));
#12261=CARTESIAN_POINT('Ctrl Pts',(6.06823728320451,-2.99988523987078,14.5508561818778));
#12262=CARTESIAN_POINT('Ctrl Pts',(6.14363633818558,-2.84226168399215,14.5590687476013));
#12263=CARTESIAN_POINT('Ctrl Pts',(6.21277650421415,-2.6821068414,14.5672813133249));
#12264=CARTESIAN_POINT('Ctrl Pts',(6.2820115405274,-2.52173224325353,14.5755051478736));
#12265=CARTESIAN_POINT('Ctrl Pts',(6.34497039488857,-2.35881975129657,14.5837289824224));
#12266=CARTESIAN_POINT('Ctrl Pts',(6.40148931351874,-2.19390600730873,14.5919528169712));
#12267=CARTESIAN_POINT('Ctrl Pts',(6.45341956803154,-2.04238129831731,14.5995089739455));
#12268=CARTESIAN_POINT('Ctrl Pts',(6.49991364943102,-1.8891674794027,14.6070651309199));
#12269=CARTESIAN_POINT('Ctrl Pts',(6.54088257718518,-1.73468847678058,14.6146212878942));
#12270=CARTESIAN_POINT('Ctrl Pts',(6.58775902502417,-1.55793435345847,14.6232670059466));
#12271=CARTESIAN_POINT('Ctrl Pts',(6.62750858751518,-1.37912093385762,14.6319127239989));
#12272=CARTESIAN_POINT('Ctrl Pts',(6.65996096138983,-1.19883651627882,14.6405584420513));
#12273=CARTESIAN_POINT('Ctrl Pts',(6.69237167303007,-1.01878354715095,14.6491930607636));
#12274=CARTESIAN_POINT('Ctrl Pts',(6.71750382276465,-0.837263644455639,
14.657827679476));
#12275=CARTESIAN_POINT('Ctrl Pts',(6.73523747564718,-0.654877963163986,
14.6664622981884));
#12276=CARTESIAN_POINT('Ctrl Pts',(6.75359741225974,-0.466051128121339,
14.6754018580908));
#12277=CARTESIAN_POINT('Ctrl Pts',(6.76402663197152,-0.276296549436255,
14.6843414179932));
#12278=CARTESIAN_POINT('Ctrl Pts',(6.7664497667447,-0.0862934187562398,
14.6932809778957));
#12279=CARTESIAN_POINT('Ctrl Pts',(6.76878374890793,0.09671906691934,14.7018916311661));
#12280=CARTESIAN_POINT('Ctrl Pts',(6.76369021095113,0.279961794029591,14.7105022844366));
#12281=CARTESIAN_POINT('Ctrl Pts',(6.7511543544222,0.462821653303111,14.7191129377071));
#12282=CARTESIAN_POINT('Ctrl Pts',(6.73863036392011,0.645508423486494,14.7277154404182));
#12283=CARTESIAN_POINT('Ctrl Pts',(6.71867812078026,0.827812745107107,14.7363179431293));
#12284=CARTESIAN_POINT('Ctrl Pts',(6.69133485708387,1.009121811465,14.7449204458404));
#12285=CARTESIAN_POINT('Ctrl Pts',(6.66402236768029,1.19022681811882,14.7535132666079));
#12286=CARTESIAN_POINT('Ctrl Pts',(6.62933549815467,1.37033850321513,14.7621060873754));
#12287=CARTESIAN_POINT('Ctrl Pts',(6.58736327713615,1.54884926801741,14.7706989081429));
#12288=CARTESIAN_POINT('Ctrl Pts',(6.58241666024053,1.56988757249101,14.7717116111011));
#12289=CARTESIAN_POINT('Ctrl Pts',(6.57736891118489,1.59090364736417,14.7727243140594));
#12290=CARTESIAN_POINT('Ctrl Pts',(6.57222022306497,1.61189650397781,14.7737370170176));
#12291=CARTESIAN_POINT('Ctrl Pts',(6.52852103056551,1.79007215977691,14.7823322747777));
#12292=CARTESIAN_POINT('Ctrl Pts',(6.47759776454528,1.9663647392222,14.7909275325378));
#12293=CARTESIAN_POINT('Ctrl Pts',(6.4196470761144,2.14019167789614,14.7995227902978));
#12294=CARTESIAN_POINT('Ctrl Pts',(6.36164211932129,2.31418139812675,14.8081260971523));
#12295=CARTESIAN_POINT('Ctrl Pts',(6.29659670099373,2.4857005791225,14.8167294040068));
#12296=CARTESIAN_POINT('Ctrl Pts',(6.22475593460164,2.65418585533148,14.8253327108613));
#12297=CARTESIAN_POINT('Ctrl Pts',(6.14993662512315,2.82965658951669,14.8342927138013));
#12298=CARTESIAN_POINT('Ctrl Pts',(6.06774664756277,3.00183613942243,14.8432527167412));
#12299=CARTESIAN_POINT('Ctrl Pts',(5.97851554764615,3.17011685061502,14.8522127196812));
#12300=CARTESIAN_POINT('Ctrl Pts',(5.89260232717896,3.33214038113938,14.860839562886));
#12301=CARTESIAN_POINT('Ctrl Pts',(5.80016235165871,3.49054955350911,14.8694664060907));
#12302=CARTESIAN_POINT('Ctrl Pts',(5.70153411846878,3.64483164164498,14.8780932492955));
#12303=CARTESIAN_POINT('Ctrl Pts',(5.60281162161947,3.79926118445721,14.8867283375816));
#12304=CARTESIAN_POINT('Ctrl Pts',(5.49788923338844,3.94955551788104,14.8953634258678));
#12305=CARTESIAN_POINT('Ctrl Pts',(5.38714710240445,4.09523321644267,14.9039985141539));
#12306=CARTESIAN_POINT('Ctrl Pts',(5.27624049713202,4.24112727562152,14.9126464272791));
#12307=CARTESIAN_POINT('Ctrl Pts',(5.15949706732643,4.38239076018922,14.9212943404042));
#12308=CARTESIAN_POINT('Ctrl Pts',(5.0373362968425,4.51857632806099,14.9299422535294));
#12309=CARTESIAN_POINT('Ctrl Pts',(5.02363171806996,4.53385427559839,14.9309124177333));
#12310=CARTESIAN_POINT('Ctrl Pts',(5.00985899663787,4.54906835482126,14.9318825819371));
#12311=CARTESIAN_POINT('Ctrl Pts',(4.99601875237309,4.56421796433261,14.932852746141));
#12312=CARTESIAN_POINT('Ctrl Pts',(4.87866384123369,4.69267531262694,14.9410790123657));
#12313=CARTESIAN_POINT('Ctrl Pts',(4.7561967314082,4.81677293629984,14.9493052785904));
#12314=CARTESIAN_POINT('Ctrl Pts',(4.62897400458076,4.93608029360499,14.9575315448151));
#12315=CARTESIAN_POINT('Ctrl Pts',(4.50191908125205,5.05523028757988,14.9657469608065));
#12316=CARTESIAN_POINT('Ctrl Pts',(4.37012130086407,5.16960236340963,14.973962376798));
#12317=CARTESIAN_POINT('Ctrl Pts',(4.23397606086872,5.27880059445236,14.9821777927895));
#12318=CARTESIAN_POINT('Ctrl Pts',(4.09793449084457,5.38791567475499,14.990386953021));
#12319=CARTESIAN_POINT('Ctrl Pts',(3.95755232917933,5.4918645300023,14.9985961132526));
#12320=CARTESIAN_POINT('Ctrl Pts',(3.81326072202526,5.590289050296,15.0068052734841));
#12321=CARTESIAN_POINT('Ctrl Pts',(3.66906843414041,5.68864582270318,15.0150087831597));
#12322=CARTESIAN_POINT('Ctrl Pts',(3.52097235714589,5.78148563488334,15.0232122928354));
#12323=CARTESIAN_POINT('Ctrl Pts',(3.36943541864658,5.86849162558574,15.031415802511));
#12324=CARTESIAN_POINT('Ctrl Pts',(3.28050067686138,5.9195541281908,15.0362303185093));
#12325=CARTESIAN_POINT('Ctrl Pts',(3.19038138094769,5.96860804591482,15.0410448345075));
#12326=CARTESIAN_POINT('Ctrl Pts',(3.09917575053257,6.0155962852664,15.0458593505058));
#12327=CARTESIAN_POINT('Ctrl Pts',(3.09917575053261,6.01559628526638,13.045945719425));
#12328=CARTESIAN_POINT('Ctrl Pts',(2.94589749677957,6.09456372666182,13.054090403068));
#12329=CARTESIAN_POINT('Ctrl Pts',(2.7893836746281,6.16778000659029,13.062235086711));
#12330=CARTESIAN_POINT('Ctrl Pts',(2.63010911547121,6.234967124269,13.070379770354));
#12331=CARTESIAN_POINT('Ctrl Pts',(2.47099810587648,6.30208525149666,13.0785160907062));
#12332=CARTESIAN_POINT('Ctrl Pts',(2.30913233709464,6.3631864003597,13.0866524110585));
#12333=CARTESIAN_POINT('Ctrl Pts',(2.1450116533509,6.41803817431689,13.0947887314108));
#12334=CARTESIAN_POINT('Ctrl Pts',(1.98102497110466,6.47284516281692,13.1029184086082));
#12335=CARTESIAN_POINT('Ctrl Pts',(1.81478738476683,6.52141282054947,13.1110480858057));
#12336=CARTESIAN_POINT('Ctrl Pts',(1.64681915269871,6.56355663328235,13.1191777630031));
#12337=CARTESIAN_POINT('Ctrl Pts',(1.47895274518715,6.60567489788038,13.1273025118831));
#12338=CARTESIAN_POINT('Ctrl Pts',(1.30935813494568,6.64137698378639,13.135427260763));
#12339=CARTESIAN_POINT('Ctrl Pts',(1.13857118912809,6.67052806360092,13.143552009643));
#12340=CARTESIAN_POINT('Ctrl Pts',(0.965025754317399,6.70014998111572,13.151807986529));
#12341=CARTESIAN_POINT('Ctrl Pts',(0.790249501735948,6.72300733236068,13.160063963415));
#12342=CARTESIAN_POINT('Ctrl Pts',(0.614816607369404,6.73901250475934,13.168319940301));
#12343=CARTESIAN_POINT('Ctrl Pts',(0.442243001821795,6.75475681723975,13.1764413573458));
#12344=CARTESIAN_POINT('Ctrl Pts',(0.269034373158783,6.7638705907001,13.1845627743907));
#12345=CARTESIAN_POINT('Ctrl Pts',(0.0957431469898265,6.76632265339191,
13.1926841914355));
#12346=CARTESIAN_POINT('Ctrl Pts',(-0.0775591384366407,6.76877487257169,
13.2008061267804));
#12347=CARTESIAN_POINT('Ctrl Pts',(-0.250943665915966,6.76456452879857,
13.2089280621252));
#12348=CARTESIAN_POINT('Ctrl Pts',(-0.42385758428952,6.75371258999376,13.21704999747));
#12349=CARTESIAN_POINT('Ctrl Pts',(-0.596815464492231,6.74285789217983,
13.2251739977449));
#12350=CARTESIAN_POINT('Ctrl Pts',(-0.769302132211122,6.7253582599974,13.2332979980197));
#12351=CARTESIAN_POINT('Ctrl Pts',(-0.940769476151189,6.70128657742244,
13.2414219982945));
#12352=CARTESIAN_POINT('Ctrl Pts',(-1.11713603092092,6.67652711229222,13.2497781196789));
#12353=CARTESIAN_POINT('Ctrl Pts',(-1.29242373346546,6.64481450465825,13.2581342410633));
#12354=CARTESIAN_POINT('Ctrl Pts',(-1.46604785067862,6.60628433383855,13.2664903624476));
#12355=CARTESIAN_POINT('Ctrl Pts',(-1.63511721627612,6.56876494055718,13.2746272743236));
#12356=CARTESIAN_POINT('Ctrl Pts',(-1.80260884726462,6.52478134245833,13.2827641861996));
#12357=CARTESIAN_POINT('Ctrl Pts',(-1.96799907955178,6.47450914146265,13.2909010980756));
#12358=CARTESIAN_POINT('Ctrl Pts',(-2.14007276473768,6.42220543060798,13.2993668242142));
#12359=CARTESIAN_POINT('Ctrl Pts',(-2.309871248914,6.36309443250584,13.3078325503527));
#12360=CARTESIAN_POINT('Ctrl Pts',(-2.47682913674139,6.29742855675147,13.3162982764913));
#12361=CARTESIAN_POINT('Ctrl Pts',(-2.64378702456875,6.23176268099711,13.3247640026299));
#12362=CARTESIAN_POINT('Ctrl Pts',(-2.80790394372058,6.15954216912804,13.3332297287684));
#12363=CARTESIAN_POINT('Ctrl Pts',(-2.968645063856,6.08107190262074,13.341695454907));
#12364=CARTESIAN_POINT('Ctrl Pts',(-3.12481293673833,6.00483419446846,13.3499203225846));
#12365=CARTESIAN_POINT('Ctrl Pts',(-3.27826137829459,5.92246977420169,13.3581451902622));
#12366=CARTESIAN_POINT('Ctrl Pts',(-3.42847643053927,5.8341956056715,13.3663700579398));
#12367=CARTESIAN_POINT('Ctrl Pts',(-3.57852224871382,5.74602088787282,13.3745856593833));
#12368=CARTESIAN_POINT('Ctrl Pts',(-3.72534162477454,5.65194985968362,13.3828012608268));
#12369=CARTESIAN_POINT('Ctrl Pts',(-3.86844208815066,5.55224682544144,13.3910168622704));
#12370=CARTESIAN_POINT('Ctrl Pts',(-4.01141008459231,5.45263608548672,13.3992248585985));
#12371=CARTESIAN_POINT('Ctrl Pts',(-4.1506657317795,5.34740392607763,13.4074328549267));
#12372=CARTESIAN_POINT('Ctrl Pts',(-4.28574254716233,5.23685972883011,13.4156408512548));
#12373=CARTESIAN_POINT('Ctrl Pts',(-4.4207214539168,5.12639565806984,13.4238428981262));
#12374=CARTESIAN_POINT('Ctrl Pts',(-4.55152728548307,5.01062744495931,13.4320449449977));
#12375=CARTESIAN_POINT('Ctrl Pts',(-4.67772380324455,4.88990685193076,13.4402469918691));
#12376=CARTESIAN_POINT('Ctrl Pts',(-4.80385419053292,4.76924951983898,13.4484447406407));
#12377=CARTESIAN_POINT('Ctrl Pts',(-4.92537981725779,4.64364522526605,13.4566424894123));
#12378=CARTESIAN_POINT('Ctrl Pts',(-5.04189865823783,4.51348500829011,13.4648402381838));
#12379=CARTESIAN_POINT('Ctrl Pts',(-5.15839527558922,4.38334961676131,13.4730364233994));
#12380=CARTESIAN_POINT('Ctrl Pts',(-5.26988676563717,4.24866029656104,13.4812326086151));
#12381=CARTESIAN_POINT('Ctrl Pts',(-5.37600881867134,4.10984405805963,13.4894287938307));
#12382=CARTESIAN_POINT('Ctrl Pts',(-5.48212302103556,3.9710380888702,13.497624372711));
#12383=CARTESIAN_POINT('Ctrl Pts',(-5.58286835882044,3.82810609391566,13.5058199515914));
#12384=CARTESIAN_POINT('Ctrl Pts',(-5.67792163962859,3.68150714439581,13.5140155304717));
#12385=CARTESIAN_POINT('Ctrl Pts',(-5.77298518242844,3.53489236799243,13.5222119941502));
#12386=CARTESIAN_POINT('Ctrl Pts',(-5.86235524868935,3.38461014943962,13.5304084578286));
#12387=CARTESIAN_POINT('Ctrl Pts',(-5.94575268618598,3.23114747337726,13.5386049215071));
#12388=CARTESIAN_POINT('Ctrl Pts',(-6.02917430054413,3.07764030858743,13.5468037613349));
#12389=CARTESIAN_POINT('Ctrl Pts',(-6.10661966599629,2.92095116496101,13.5550026011627));
#12390=CARTESIAN_POINT('Ctrl Pts',(-6.17785616444124,2.76159052204982,13.5632014409905));
#12391=CARTESIAN_POINT('Ctrl Pts',(-6.24916707143531,2.60206342241369,13.5714088447397));
#12392=CARTESIAN_POINT('Ctrl Pts',(-6.31425600792885,2.43985957655252,13.5796162484889));
#12393=CARTESIAN_POINT('Ctrl Pts',(-6.37293862778668,2.27550922794534,13.5878236522382));
#12394=CARTESIAN_POINT('Ctrl Pts',(-6.43165268116115,2.11107084459415,13.5960354523072));
#12395=CARTESIAN_POINT('Ctrl Pts',(-6.48395346961002,1.94448400841016,13.6042472523762));
#12396=CARTESIAN_POINT('Ctrl Pts',(-6.52970694613362,1.77629282428724,13.6124590524452));
#12397=CARTESIAN_POINT('Ctrl Pts',(-6.57552777816776,1.60785403924009,13.6206829414314));
#12398=CARTESIAN_POINT('Ctrl Pts',(-6.61478195517534,1.43780653585421,13.6289068304175));
#12399=CARTESIAN_POINT('Ctrl Pts',(-6.64738659624081,1.26670455912892,13.6371307194037));
#12400=CARTESIAN_POINT('Ctrl Pts',(-6.67751272092189,1.10860929061629,13.6447294506537));
#12401=CARTESIAN_POINT('Ctrl Pts',(-6.70196238596804,0.949614070944114,
13.6523281819037));
#12402=CARTESIAN_POINT('Ctrl Pts',(-6.72070973630126,0.790157984447094,
13.6599269131537));
#12403=CARTESIAN_POINT('Ctrl Pts',(-6.75134610589733,0.529579528642073,
13.6723445367058));
#12404=CARTESIAN_POINT('Ctrl Pts',(-6.76683134497133,0.267185721162299,
13.6847621602579));
#12405=CARTESIAN_POINT('Ctrl Pts',(-6.76699862985665,0.00430621854705538,
13.69717978381));
#12406=CARTESIAN_POINT('',(-6.767,1.40740026512327E-12,13.3028202161899));
#12407=CARTESIAN_POINT('Ctrl Pts',(3.09917575053257,6.0155962852664,12.6511155556306));
#12408=CARTESIAN_POINT('Ctrl Pts',(2.94532479176222,6.09485877862638,12.6592595382568));
#12409=CARTESIAN_POINT('Ctrl Pts',(2.78858665361273,6.16813513728891,12.6674035208829));
#12410=CARTESIAN_POINT('Ctrl Pts',(2.62947835233266,6.23523316281067,12.6755475035091));
#12411=CARTESIAN_POINT('Ctrl Pts',(2.47013644809179,6.30242970171796,12.6837034431384));
#12412=CARTESIAN_POINT('Ctrl Pts',(2.30841777229537,6.36342966448213,12.6918593827677));
#12413=CARTESIAN_POINT('Ctrl Pts',(2.14485468170803,6.41809063463232,12.700015322397));
#12414=CARTESIAN_POINT('Ctrl Pts',(2.06389975203557,6.44514487393807,12.7040520737003));
#12415=CARTESIAN_POINT('Ctrl Pts',(1.98249316051284,6.47064702757832,12.7080888250036));
#12416=CARTESIAN_POINT('Ctrl Pts',(1.90070022083335,6.49458448790406,12.7121255763069));
#12417=CARTESIAN_POINT('Ctrl Pts',(1.73388157825965,6.54340550661118,12.7203586264389));
#12418=CARTESIAN_POINT('Ctrl Pts',(1.56493684531338,6.58586646477601,12.7285916765709));
#12419=CARTESIAN_POINT('Ctrl Pts',(1.39439157355043,6.62177930314893,12.7368247267029));
#12420=CARTESIAN_POINT('Ctrl Pts',(1.2240493949906,6.65764937485173,12.7450479725378));
#12421=CARTESIAN_POINT('Ctrl Pts',(1.0521108199802,6.68698678103675,12.7532712183727));
#12422=CARTESIAN_POINT('Ctrl Pts',(0.879117648729215,6.70965283451334,12.7614944642075));
#12423=CARTESIAN_POINT('Ctrl Pts',(0.706295860796889,6.73229643286387,12.769709563321));
#12424=CARTESIAN_POINT('Ctrl Pts',(0.532421910026123,6.74828179473598,12.7779246624345));
#12425=CARTESIAN_POINT('Ctrl Pts',(0.358049008625063,6.75752098830796,12.786139761548));
#12426=CARTESIAN_POINT('Ctrl Pts',(0.183813968928741,6.76675287724164,12.7943483656869));
#12427=CARTESIAN_POINT('Ctrl Pts',(0.009081120393062,6.76924920250609,12.8025569698258));
#12428=CARTESIAN_POINT('Ctrl Pts',(-0.165589862747555,6.76497368785387,
12.8107655739647));
#12429=CARTESIAN_POINT('Ctrl Pts',(-0.340157687582229,6.76070069826244,
12.8189693302137));
#12430=CARTESIAN_POINT('Ctrl Pts',(-0.514663362693545,6.74966384475748,
12.8271730864627));
#12431=CARTESIAN_POINT('Ctrl Pts',(-0.688545766638032,6.731878915076,12.8353768427117));
#12432=CARTESIAN_POINT('Ctrl Pts',(-0.862376723161842,6.71409924750696,
12.8435781716759));
#12433=CARTESIAN_POINT('Ctrl Pts',(-1.03558441959404,6.68957551344629,12.8517795006402));
#12434=CARTESIAN_POINT('Ctrl Pts',(-1.20761115969753,6.65837549909691,12.8599808296045));
#12435=CARTESIAN_POINT('Ctrl Pts',(-1.3796141756712,6.62717978752738,12.8681810275272));
#12436=CARTESIAN_POINT('Ctrl Pts',(-1.55043620713395,6.58930969255507,12.8763812254499));
#12437=CARTESIAN_POINT('Ctrl Pts',(-1.71952805575321,6.5448844348451,12.8845814233727));
#12438=CARTESIAN_POINT('Ctrl Pts',(-1.8886272278758,6.50045725304164,12.8927819764525));
#12439=CARTESIAN_POINT('Ctrl Pts',(-2.05599572130581,6.44947443387279,12.9009825295324));
#12440=CARTESIAN_POINT('Ctrl Pts',(-2.22109778859676,6.39210556964531,12.9091830826122));
#12441=CARTESIAN_POINT('Ctrl Pts',(-2.38623692631856,6.33472382436462,12.9173854769654));
#12442=CARTESIAN_POINT('Ctrl Pts',(-2.54910828598719,6.27095329575223,12.9255878713186));
#12443=CARTESIAN_POINT('Ctrl Pts',(-2.70919439336898,6.20101239628966,12.9337902656718));
#12444=CARTESIAN_POINT('Ctrl Pts',(-2.86943020940303,6.13100608979105,12.9420003307056));
#12445=CARTESIAN_POINT('Ctrl Pts',(-3.0268752404332,6.05481802732757,12.9502103957395));
#12446=CARTESIAN_POINT('Ctrl Pts',(-3.18103414974751,5.97271385034811,12.9584204607733));
#12447=CARTESIAN_POINT('Ctrl Pts',(-3.33526683678104,5.89057037976607,12.9666344549986));
#12448=CARTESIAN_POINT('Ctrl Pts',(-3.48620995713884,5.80250532987613,12.9748484492239));
#12449=CARTESIAN_POINT('Ctrl Pts',(-3.63339571791366,5.70882865017393,12.9830624434493));
#12450=CARTESIAN_POINT('Ctrl Pts',(-3.78078214190203,5.61502425795739,12.9912876360844));
#12451=CARTESIAN_POINT('Ctrl Pts',(-3.92440067420043,5.51559315026165,12.9995128287196));
#12452=CARTESIAN_POINT('Ctrl Pts',(-4.0638142893429,5.41088739688163,13.0077380213548));
#12453=CARTESIAN_POINT('Ctrl Pts',(-4.18918865484122,5.31672573712818,13.0151349194747));
#12454=CARTESIAN_POINT('Ctrl Pts',(-4.31116265020452,5.21829894024396,13.0225318175947));
#12455=CARTESIAN_POINT('Ctrl Pts',(-4.4294436240944,5.11588879677515,13.0299287157146));
#12456=CARTESIAN_POINT('Ctrl Pts',(-4.56769797344227,4.9961852866816,13.0385746822055));
#12457=CARTESIAN_POINT('Ctrl Pts',(-4.70122024466824,4.87076751104999,13.0472206486964));
#12458=CARTESIAN_POINT('Ctrl Pts',(-4.82953855572552,4.74002598503011,13.0558666151873));
#12459=CARTESIAN_POINT('Ctrl Pts',(-4.95769273021877,4.60945169519562,13.0645015223116));
#12460=CARTESIAN_POINT('Ctrl Pts',(-5.08065600555787,4.47356745071522,13.073136429436));
#12461=CARTESIAN_POINT('Ctrl Pts',(-5.19799090404531,4.33280273742785,13.0817713365604));
#12462=CARTESIAN_POINT('Ctrl Pts',(-5.31922122645921,4.18736474927332,13.0906929156319));
#12463=CARTESIAN_POINT('Ctrl Pts',(-5.43444277310879,4.03671685598993,13.0996144947034));
#12464=CARTESIAN_POINT('Ctrl Pts',(-5.54321367318089,3.88137490761462,13.1085360737749));
#12465=CARTESIAN_POINT('Ctrl Pts',(-5.64819874677098,3.73143971473676,13.1171471327506));
#12466=CARTESIAN_POINT('Ctrl Pts',(-5.7471744107683,3.57713197712779,13.1257581917263));
#12467=CARTESIAN_POINT('Ctrl Pts',(-5.83978328245506,3.41895016254383,13.134369250702));
#12468=CARTESIAN_POINT('Ctrl Pts',(-5.93230481970014,3.26091752071413,13.1429721890515));
#12469=CARTESIAN_POINT('Ctrl Pts',(-6.01847138182566,3.09901834820389,13.151575127401));
#12470=CARTESIAN_POINT('Ctrl Pts',(-6.09796876350521,2.93378014842878,13.1601780657506));
#12471=CARTESIAN_POINT('Ctrl Pts',(-6.17737712650779,2.76872697721207,13.1687713707993));
#12472=CARTESIAN_POINT('Ctrl Pts',(-6.25013107546449,2.60034251203016,13.177364675848));
#12473=CARTESIAN_POINT('Ctrl Pts',(-6.31596214781488,2.42917910977548,13.1859579808968));
#12474=CARTESIAN_POINT('Ctrl Pts',(-6.32329680681988,2.41010870510411,13.1869154157373));
#12475=CARTESIAN_POINT('Ctrl Pts',(-6.33054557508072,2.39100382863419,13.1878728505779));
#12476=CARTESIAN_POINT('Ctrl Pts',(-6.3377081169916,2.37186526257686,13.1888302854184));
#12477=CARTESIAN_POINT('Ctrl Pts',(-6.39853439478797,2.20933529066032,13.1969610856716));
#12478=CARTESIAN_POINT('Ctrl Pts',(-6.45309310219485,2.04449445500953,13.2050918859248));
#12479=CARTESIAN_POINT('Ctrl Pts',(-6.50122165943161,1.87787271531842,13.213222686178));
#12480=CARTESIAN_POINT('Ctrl Pts',(-6.5493880577674,1.71111996921211,13.2213598792764));
#12481=CARTESIAN_POINT('Ctrl Pts',(-6.59111410585841,1.54258387283326,13.2294970723749));
#12482=CARTESIAN_POINT('Ctrl Pts',(-6.62628766982595,1.3728076036767,13.2376342654733));
#12483=CARTESIAN_POINT('Ctrl Pts',(-6.66147613186161,1.20295942430871,13.2457749051505));
#12484=CARTESIAN_POINT('Ctrl Pts',(-6.69010651725162,1.03187038450069,13.2539155448276));
#12485=CARTESIAN_POINT('Ctrl Pts',(-6.7121183391382,0.86009092624247,13.2620561845048));
#12486=CARTESIAN_POINT('Ctrl Pts',(-6.73415609503676,0.688109079897025,
13.2702064153665));
#12487=CARTESIAN_POINT('Ctrl Pts',(-6.74955967681732,0.515435553012798,
13.2783566462283));
#12488=CARTESIAN_POINT('Ctrl Pts',(-6.75832064195188,0.342623847049734,
13.28650687709));
#12489=CARTESIAN_POINT('Ctrl Pts',(-6.76411034278237,0.228420895415216,
13.2918929729897));
#12490=CARTESIAN_POINT('Ctrl Pts',(-6.76700012102719,0.114157610253499,
13.2972790688895));
#12491=CARTESIAN_POINT('Ctrl Pts',(-6.7669999999962,-7.17398757052791E-6,
13.3026651647892));
#12492=CARTESIAN_POINT('Ctrl Pts',(-6.767,1.4554827223919E-12,13.3028202161899));
#12493=CARTESIAN_POINT('Ctrl Pts',(-6.76700000000004,-0.186007249414258,
13.3115697279959));
#12494=CARTESIAN_POINT('Ctrl Pts',(-6.75932637295446,-0.372014355526148,
13.3203192398018));
#12495=CARTESIAN_POINT('Ctrl Pts',(-6.74400518266939,-0.557389537153701,
13.3290687516078));
#12496=CARTESIAN_POINT('Ctrl Pts',(-6.72868405709659,-0.742763935810194,
13.3378182264583));
#12497=CARTESIAN_POINT('Ctrl Pts',(-6.70571545653006,-0.927506129693977,
13.3465677013089));
#12498=CARTESIAN_POINT('Ctrl Pts',(-6.67517739415665,-1.11098863924884,
13.3553171761594));
#12499=CARTESIAN_POINT('Ctrl Pts',(-6.64463945823081,-1.294470389066,13.3640666147814));
#12500=CARTESIAN_POINT('Ctrl Pts',(-6.6065321702713,-1.4766921822834,13.3728160534034));
#12501=CARTESIAN_POINT('Ctrl Pts',(-6.56098496116674,-1.65703510504269,
13.3815654920254));
#12502=CARTESIAN_POINT('Ctrl Pts',(-6.51543793687471,-1.83737729604186,
13.3903148951456));
#12503=CARTESIAN_POINT('Ctrl Pts',(-6.46245112202583,-2.01584035397235,
13.3990642982659));
#12504=CARTESIAN_POINT('Ctrl Pts',(-6.40220448416175,-2.19181813638341,
13.4078137013861));
#12505=CARTESIAN_POINT('Ctrl Pts',(-6.34195808575111,-2.36779521936147,
13.4165630697314));
#12506=CARTESIAN_POINT('Ctrl Pts',(-6.2744520148915,-2.54128677545037,13.4253124380767));
#12507=CARTESIAN_POINT('Ctrl Pts',(-6.19991555136089,-2.71170355238056,
13.4340618064219));
#12508=CARTESIAN_POINT('Ctrl Pts',(-6.12537937788937,-2.88211966613287,
13.442811140719));
#12509=CARTESIAN_POINT('Ctrl Pts',(-6.04381298133509,-3.04946076210659,
13.4515604750161));
#12510=CARTESIAN_POINT('Ctrl Pts',(-5.95549339426192,-3.21315848207067,
13.4603098093131));
#12511=CARTESIAN_POINT('Ctrl Pts',(-5.86717414355034,-3.37685557859857,
13.4690591102887));
#12512=CARTESIAN_POINT('Ctrl Pts',(-5.77210188986098,-3.5369090746754,13.4778084112642));
#12513=CARTESIAN_POINT('Ctrl Pts',(-5.67059953466914,-3.69277536785141,
13.4865577122398));
#12514=CARTESIAN_POINT('Ctrl Pts',(-5.56909755761607,-3.84864108036022,
13.4953069806206));
#12515=CARTESIAN_POINT('Ctrl Pts',(-5.46116568337908,-4.00031938104501,
13.5040562490013));
#12516=CARTESIAN_POINT('Ctrl Pts',(-5.34717048685949,-4.14729511663432,
13.5128055173821));
#12517=CARTESIAN_POINT('Ctrl Pts',(-5.23317570555347,-4.29427031688248,
13.5215547538947));
#12518=CARTESIAN_POINT('Ctrl Pts',(-5.1131178217863,-4.43654275987332,13.5303039904073));
#12519=CARTESIAN_POINT('Ctrl Pts',(-4.98740459171835,-4.57362924147845,
13.53905322692));
#12520=CARTESIAN_POINT('Ctrl Pts',(-4.86169180910641,-4.71071523514631,
13.5478024322911));
#12521=CARTESIAN_POINT('Ctrl Pts',(-4.73032391415233,-4.84261509316718,
13.5565516376622));
#12522=CARTESIAN_POINT('Ctrl Pts',(-4.59374707237085,-4.96888084331716,
13.5653008430333));
#12523=CARTESIAN_POINT('Ctrl Pts',(-4.45717070537192,-5.09514615452908,
13.5740500179895));
#12524=CARTESIAN_POINT('Ctrl Pts',(-4.31538563819297,-5.21577720253808,
13.5827991929458));
#12525=CARTESIAN_POINT('Ctrl Pts',(-4.16887341290434,-5.33036429028817,
13.591548367902));
#12526=CARTESIAN_POINT('Ctrl Pts',(-4.02236168477138,-5.44495098921324,
13.6002975131699));
#12527=CARTESIAN_POINT('Ctrl Pts',(-3.87112305634253,-5.55349359238888,
13.6090466584378));
#12528=CARTESIAN_POINT('Ctrl Pts',(-3.71567117316562,-5.65562346102585,
13.6177958037057));
#12529=CARTESIAN_POINT('Ctrl Pts',(-3.56021980457113,-5.75775299158886,
13.6265449200119));
#12530=CARTESIAN_POINT('Ctrl Pts',(-3.40055544862182,-5.85346967275473,
13.6352940363181));
#12531=CARTESIAN_POINT('Ctrl Pts',(-3.23722036323179,-5.94244842803683,
13.6440431526242));
#12532=CARTESIAN_POINT('Ctrl Pts',(-3.07388580495831,-6.03142689616585,
13.6527922406952));
#12533=CARTESIAN_POINT('Ctrl Pts',(-2.906880792575,-6.1136673448492,13.6615413287661));
#12534=CARTESIAN_POINT('Ctrl Pts',(-2.73677251094418,-6.18889046787389,
13.670290416837));
#12535=CARTESIAN_POINT('Ctrl Pts',(-2.5666647641648,-6.26411335438337,13.6790394773993));
#12536=CARTESIAN_POINT('Ctrl Pts',(-2.39345402971961,-6.3323188435034,13.6877885379615));
#12537=CARTESIAN_POINT('Ctrl Pts',(-2.2177285647394,-6.39327529621077,13.6965375985237));
#12538=CARTESIAN_POINT('Ctrl Pts',(-2.0420036376821,-6.45423156232099,13.7052866323037));
#12539=CARTESIAN_POINT('Ctrl Pts',(-1.86376426620073,-6.5079387425206,13.7140356660836));
#12540=CARTESIAN_POINT('Ctrl Pts',(-1.68361578194709,-6.55421443796117,
13.7227846998636));
#12541=CARTESIAN_POINT('Ctrl Pts',(-1.50346783419883,-6.60048999558676,
13.7315337075879));
#12542=CARTESIAN_POINT('Ctrl Pts',(-1.32141106257256,-6.63933404145494,
13.7402827153121));
#12543=CARTESIAN_POINT('Ctrl Pts',(-1.13806375959048,-6.67061465527029,
13.7490317230363));
#12544=CARTESIAN_POINT('Ctrl Pts',(-0.954716987419194,-6.7018951785248,
13.7577807054312));
#12545=CARTESIAN_POINT('Ctrl Pts',(-0.770079973809923,-6.72561226535827,
13.7665296878261));
#12546=CARTESIAN_POINT('Ctrl Pts',(-0.58477977055251,-6.74168536939782,
13.775278670221));
#12547=CARTESIAN_POINT('Ctrl Pts',(-0.391490647553973,-6.75845143942393,
13.784404850897));
#12548=CARTESIAN_POINT('Ctrl Pts',(-0.197480213104408,-6.76689975924026,
13.7935310315731));
#12549=CARTESIAN_POINT('Ctrl Pts',(-0.00346532629787789,-6.76699911271707,
13.8026572122491));
#12550=CARTESIAN_POINT('Ctrl Pts',(0.184486595295947,-6.76709536139774,
13.8114981997791));
#12551=CARTESIAN_POINT('Ctrl Pts',(0.372442378185097,-6.75935659726771,
13.820339187309));
#12552=CARTESIAN_POINT('Ctrl Pts',(0.559750217721928,-6.74380965729018,
13.8291801748389));
#12553=CARTESIAN_POINT('Ctrl Pts',(0.745129914457576,-6.72842275717255,
13.8379301534367));
#12554=CARTESIAN_POINT('Ctrl Pts',(0.929874656313986,-6.70538772273475,
13.8466801320344));
#12555=CARTESIAN_POINT('Ctrl Pts',(1.11335688289756,-6.67478280180746,13.8554301106322));
#12556=CARTESIAN_POINT('Ctrl Pts',(1.29683723118834,-6.64417819418028,13.8641799996572));
#12557=CARTESIAN_POINT('Ctrl Pts',(1.47905480730212,-6.6060039023008,13.8729298886821));
#12558=CARTESIAN_POINT('Ctrl Pts',(1.65939064804784,-6.5603895979714,13.881679777707));
#12559=CARTESIAN_POINT('Ctrl Pts',(1.83972470264243,-6.51477574543262,13.890429580068));
#12560=CARTESIAN_POINT('Ctrl Pts',(2.01817678125828,-6.46172209820106,13.8991793824289));
#12561=CARTESIAN_POINT('Ctrl Pts',(2.19414072347661,-6.40140886724021,13.9079291847899));
#12562=CARTESIAN_POINT('Ctrl Pts',(2.37010298132087,-6.34109621361378,13.9166789033954));
#12563=CARTESIAN_POINT('Ctrl Pts',(2.54357687926911,-6.27352420825972,13.9254286220009));
#12564=CARTESIAN_POINT('Ctrl Pts',(2.71397317789977,-6.19892237325494,13.9341783406063));
#12565=CARTESIAN_POINT('Ctrl Pts',(2.88436790207209,-6.1243212275696,13.9429279783646));
#12566=CARTESIAN_POINT('Ctrl Pts',(3.05168482126265,-6.04269049717413,13.9516776161229));
#12567=CARTESIAN_POINT('Ctrl Pts',(3.21535561997399,-5.95430745234924,13.9604272538812));
#12568=CARTESIAN_POINT('Ctrl Pts',(3.37902496075288,-5.86592519481512,13.9691768137002));
#12569=CARTESIAN_POINT('Ctrl Pts',(3.53904799384879,-5.77079087940229,13.9779263735192));
#12570=CARTESIAN_POINT('Ctrl Pts',(3.69488118814986,-5.66922763747023,13.9866759333382));
#12571=CARTESIAN_POINT('Ctrl Pts',(3.85071304610831,-5.56766526649053,13.9954254181256));
#12572=CARTESIAN_POINT('Ctrl Pts',(4.00235489705962,-5.45967423580718,14.0041749029131));
#12573=CARTESIAN_POINT('Ctrl Pts',(4.14929168607645,-5.34562133936335,14.0129243877005));
#12574=CARTESIAN_POINT('Ctrl Pts',(4.29622726385748,-5.23156938308538,14.0216738003638));
#12575=CARTESIAN_POINT('Ctrl Pts',(4.43845763092058,-5.1114558367721,14.0304232130271));
#12576=CARTESIAN_POINT('Ctrl Pts',(4.57549970660954,-4.98568866204219,14.0391726256904));
#12577=CARTESIAN_POINT('Ctrl Pts',(4.71254069815277,-4.85992248226178,14.0479219691367));
#12578=CARTESIAN_POINT('Ctrl Pts',(4.84439326931288,-4.72850295734028,14.056671312583));
#12579=CARTESIAN_POINT('Ctrl Pts',(4.97060959434664,-4.59187644221718,14.0654206560294));
#12580=CARTESIAN_POINT('Ctrl Pts',(5.0968249628049,-4.45525096256693,14.0741699331657));
#12581=CARTESIAN_POINT('Ctrl Pts',(5.21740397615822,-4.31341878218347,14.082919210302));
#12582=CARTESIAN_POINT('Ctrl Pts',(5.33193710451924,-4.16686161438689,14.0916684874383));
#12583=CARTESIAN_POINT('Ctrl Pts',(5.44646940289382,-4.02030550864516,14.1004177011712));
#12584=CARTESIAN_POINT('Ctrl Pts',(5.55495572749671,-3.86902470980125,14.1091669149042));
#12585=CARTESIAN_POINT('Ctrl Pts',(5.65702762491469,-3.71353301465762,14.1179161286372));
#12586=CARTESIAN_POINT('Ctrl Pts',(5.75909881655169,-3.55804239466869,14.1266652818733));
#12587=CARTESIAN_POINT('Ctrl Pts',(5.85475551250798,-3.39834117619525,14.1354144351094));
#12588=CARTESIAN_POINT('Ctrl Pts',(5.94367283728112,-3.23497174691937,14.1441635883455));
#12589=CARTESIAN_POINT('Ctrl Pts',(6.0325895767633,-3.0716033930093,14.1529126839911));
#12590=CARTESIAN_POINT('Ctrl Pts',(6.11476689685303,-2.90456712829465,14.1616617796366));
#12591=CARTESIAN_POINT('Ctrl Pts',(6.1899257052528,-2.73443024475861,14.1704108752821));
#12592=CARTESIAN_POINT('Ctrl Pts',(6.26508404388712,-2.56429442462993,14.1791599162431));
#12593=CARTESIAN_POINT('Ctrl Pts',(6.33322384283326,-2.39105828655963,14.1879089572042));
#12594=CARTESIAN_POINT('Ctrl Pts',(6.3941136872004,-2.21531017132059,14.1966579981652));
#12595=CARTESIAN_POINT('Ctrl Pts',(6.45500317120898,-2.03956309619489,14.2054069873476));
#12596=CARTESIAN_POINT('Ctrl Pts',(6.50864269270082,-1.86130434438603,14.21415597653));
#12597=CARTESIAN_POINT('Ctrl Pts',(6.55485008446342,-1.6811393071991,14.2229049657124));
#12598=CARTESIAN_POINT('Ctrl Pts',(6.60199664749412,-1.49731239211805,14.2318317792418));
#12599=CARTESIAN_POINT('Ctrl Pts',(6.64140563640914,-1.31150116499636,14.2407585927711));
#12600=CARTESIAN_POINT('Ctrl Pts',(6.67293772282178,-1.12436255155624,14.2496854063005));
#12601=CARTESIAN_POINT('Ctrl Pts',(6.70384494949876,-0.940932395050984,
14.258435320456));
#12602=CARTESIAN_POINT('Ctrl Pts',(6.72718449348934,-0.756227260506354,
14.2671852346116));
#12603=CARTESIAN_POINT('Ctrl Pts',(6.74287707373935,-0.57087456454133,14.2759351487671));
#12604=CARTESIAN_POINT('Ctrl Pts',(6.75856934538672,-0.385525513632149,
14.2846848908511));
#12605=CARTESIAN_POINT('Ctrl Pts',(6.76661493004104,-0.199529212417939,
14.293434632935));
#12606=CARTESIAN_POINT('Ctrl Pts',(6.76698649908907,-0.0135174386001735,
14.302184375019));
#12607=CARTESIAN_POINT('Ctrl Pts',(6.76735806132389,0.172490924446043,14.3109339566649));
#12608=CARTESIAN_POINT('Ctrl Pts',(6.76005588896288,0.358514472901682,14.3196835383108));
#12609=CARTESIAN_POINT('Ctrl Pts',(6.74510478454582,0.543921359662496,14.3284331199567));
#12610=CARTESIAN_POINT('Ctrl Pts',(6.73015393440685,0.729325093150733,14.3371825527958));
#12611=CARTESIAN_POINT('Ctrl Pts',(6.70755443556893,0.914111900256644,14.3459319856348));
#12612=CARTESIAN_POINT('Ctrl Pts',(6.67738304682314,1.09765415591568,14.3546814184738));
#12613=CARTESIAN_POINT('Ctrl Pts',(6.64721213111854,1.28119353391305,14.3634307141352));
#12614=CARTESIAN_POINT('Ctrl Pts',(6.60946960955487,1.46348811672688,14.3721800097965));
#12615=CARTESIAN_POINT('Ctrl Pts',(6.56428366991173,1.64391876348259,14.3809293054578));
#12616=CARTESIAN_POINT('Ctrl Pts',(6.51909837867706,1.82434682109758,14.3896784755687));
#12617=CARTESIAN_POINT('Ctrl Pts',(6.46646995271907,2.00291071820492,14.3984276456795));
#12618=CARTESIAN_POINT('Ctrl Pts',(6.40657713281532,2.17900400212755,14.4071768157903));
#12619=CARTESIAN_POINT('Ctrl Pts',(6.34668509279042,2.35509499309707,14.4159258719761));
#12620=CARTESIAN_POINT('Ctrl Pts',(6.27952894037507,2.5287151639817,14.4246749281619));
#12621=CARTESIAN_POINT('Ctrl Pts',(6.20533675061427,2.69927486771466,14.4334239843476));
#12622=CARTESIAN_POINT('Ctrl Pts',(6.12832117907898,2.87632521635964,14.4425059856299));
#12623=CARTESIAN_POINT('Ctrl Pts',(6.04372366626061,3.05007728920032,14.4515879869122));
#12624=CARTESIAN_POINT('Ctrl Pts',(5.95185378007852,3.21989527478226,14.4606699881944));
#12625=CARTESIAN_POINT('Ctrl Pts',(5.86334450817353,3.38350129286784,14.4694197685016));
#12626=CARTESIAN_POINT('Ctrl Pts',(5.76808562057235,3.54345567124996,14.4781695488087));
#12627=CARTESIAN_POINT('Ctrl Pts',(5.6664006880446,3.69921508465345,14.4869193291158));
#12628=CARTESIAN_POINT('Ctrl Pts',(5.56471941107898,3.85496889852319,14.4956687948693));
#12629=CARTESIAN_POINT('Ctrl Pts',(5.45661270815087,4.00652780919673,14.5044182606228));
#12630=CARTESIAN_POINT('Ctrl Pts',(5.34244776449086,4.15337704569265,14.5131677263763));
#12631=CARTESIAN_POINT('Ctrl Pts',(5.22828631819565,4.30022178356286,14.5219169240959));
#12632=CARTESIAN_POINT('Ctrl Pts',(5.10806717844037,4.44235690972716,14.5306661218155));
#12633=CARTESIAN_POINT('Ctrl Pts',(4.98219864544685,4.57929969070682,14.5394153195351));
#12634=CARTESIAN_POINT('Ctrl Pts',(4.85633329943983,4.71623900430044,14.5481642957253));
#12635=CARTESIAN_POINT('Ctrl Pts',(4.72481904033599,4.84798602483665,14.5569132719155));
#12636=CARTESIAN_POINT('Ctrl Pts',(4.58810250737141,4.97409332259178,14.5656622481058));
#12637=CARTESIAN_POINT('Ctrl Pts',(4.45137708685583,5.10020881822187,14.574411793042));
#12638=CARTESIAN_POINT('Ctrl Pts',(4.3094489263599,5.22068366307983,14.5831613379781));
#12639=CARTESIAN_POINT('Ctrl Pts',(4.16280009466598,5.33510865604899,14.5919108829143));
#12640=CARTESIAN_POINT('Ctrl Pts',(4.01615988348714,5.44952692272947,14.6006599135226));
#12641=CARTESIAN_POINT('Ctrl Pts',(3.86479978232144,5.55789587288687,14.6094089441309));
#12642=CARTESIAN_POINT('Ctrl Pts',(3.70923383580967,5.65984746713944,14.6181579747392));
#12643=CARTESIAN_POINT('Ctrl Pts',(3.5536657779943,5.76180044505452,14.6269071240872));
#12644=CARTESIAN_POINT('Ctrl Pts',(3.39389200026718,5.8573357357113,14.6356562734352));
#12645=CARTESIAN_POINT('Ctrl Pts',(3.23045513625908,5.94612887622,14.6444054227832));
#12646=CARTESIAN_POINT('Ctrl Pts',(3.18695122151489,5.96976399206735,14.6467342868962));
#12647=CARTESIAN_POINT('Ctrl Pts',(3.14318791262619,5.99292165435356,14.6490631510091));
#12648=CARTESIAN_POINT('Ctrl Pts',(3.09917575053259,6.01559628526639,14.6513920151221));
#12649=CARTESIAN_POINT('Origin',(0.,0.,-3.69717978381041));
#12650=CARTESIAN_POINT('',(3.0991757505326,6.01559628526638,17.0457515827422));
#12651=CARTESIAN_POINT('',(3.09917575053259,6.01559628526639,16.6515033120574));
#12652=CARTESIAN_POINT('',(3.09917575053259,6.01559628526639,-3.69717978381041));
#12653=CARTESIAN_POINT('',(-6.767,1.53662130762677E-12,15.69717978381));
#12654=CARTESIAN_POINT('Ctrl Pts',(-6.767,1.58470424476328E-12,15.69717978381));
#12655=CARTESIAN_POINT('Ctrl Pts',(-6.76700000000004,-0.186007249414097,
15.705929295616));
#12656=CARTESIAN_POINT('Ctrl Pts',(-6.75932637295447,-0.372014355525955,
15.7146788074219));
#12657=CARTESIAN_POINT('Ctrl Pts',(-6.74400518266941,-0.557389537153476,
15.7234283192279));
#12658=CARTESIAN_POINT('Ctrl Pts',(-6.72868405709662,-0.742763935809937,
15.7321777940784));
#12659=CARTESIAN_POINT('Ctrl Pts',(-6.7057154565301,-0.92750612969369,15.7409272689289));
#12660=CARTESIAN_POINT('Ctrl Pts',(-6.67517739415671,-1.11098863924853,
15.7496767437795));
#12661=CARTESIAN_POINT('Ctrl Pts',(-6.6446394582309,-1.29447038906553,15.7584261824015));
#12662=CARTESIAN_POINT('Ctrl Pts',(-6.60653217027144,-1.47669218228277,
15.7671756210235));
#12663=CARTESIAN_POINT('Ctrl Pts',(-6.56098496116694,-1.65703510504191,
15.7759250596455));
#12664=CARTESIAN_POINT('Ctrl Pts',(-6.51543793687494,-1.83737729604105,
15.7846744627657));
#12665=CARTESIAN_POINT('Ctrl Pts',(-6.46245112202609,-2.01584035397152,
15.7934238658859));
#12666=CARTESIAN_POINT('Ctrl Pts',(-6.40220448416204,-2.19181813638255,
15.8021732690062));
#12667=CARTESIAN_POINT('Ctrl Pts',(-6.34195808575144,-2.3677952193606,15.8109226373514));
#12668=CARTESIAN_POINT('Ctrl Pts',(-6.27445201489186,-2.54128677544947,
15.8196720056967));
#12669=CARTESIAN_POINT('Ctrl Pts',(-6.19991555136129,-2.71170355237965,
15.828421374042));
#12670=CARTESIAN_POINT('Ctrl Pts',(-6.12537937788975,-2.88211966613208,
15.8371707083391));
#12671=CARTESIAN_POINT('Ctrl Pts',(-6.04381298133543,-3.04946076210593,
15.8459200426361));
#12672=CARTESIAN_POINT('Ctrl Pts',(-5.95549339426221,-3.21315848207013,
15.8546693769332));
#12673=CARTESIAN_POINT('Ctrl Pts',(-5.86717414355068,-3.37685557859797,
15.8634186779088));
#12674=CARTESIAN_POINT('Ctrl Pts',(-5.77210188986139,-3.53690907467474,
15.8721679788843));
#12675=CARTESIAN_POINT('Ctrl Pts',(-5.67059953466961,-3.69277536785069,
15.8809172798599));
#12676=CARTESIAN_POINT('Ctrl Pts',(-5.56909755761669,-3.84864108035931,
15.8896665482406));
#12677=CARTESIAN_POINT('Ctrl Pts',(-5.46116568337986,-4.00031938104392,
15.8984158166214));
#12678=CARTESIAN_POINT('Ctrl Pts',(-5.34717048686045,-4.14729511663308,
15.9071650850021));
#12679=CARTESIAN_POINT('Ctrl Pts',(-5.2331757055545,-4.29427031688122,15.9159143215147));
#12680=CARTESIAN_POINT('Ctrl Pts',(-5.11311782178739,-4.43654275987205,
15.9246635580274));
#12681=CARTESIAN_POINT('Ctrl Pts',(-4.98740459171951,-4.57362924147719,
15.93341279454));
#12682=CARTESIAN_POINT('Ctrl Pts',(-4.86169180910741,-4.71071523514529,
15.9421619999111));
#12683=CARTESIAN_POINT('Ctrl Pts',(-4.73032391415315,-4.84261509316638,
15.9509112052822));
#12684=CARTESIAN_POINT('Ctrl Pts',(-4.59374707237148,-4.96888084331658,
15.9596604106534));
#12685=CARTESIAN_POINT('Ctrl Pts',(-4.4571707053728,-5.0951461545283,15.9684095856096));
#12686=CARTESIAN_POINT('Ctrl Pts',(-4.31538563819412,-5.21577720253712,
15.9771587605658));
#12687=CARTESIAN_POINT('Ctrl Pts',(-4.16887341290578,-5.33036429028705,
15.985907935522));
#12688=CARTESIAN_POINT('Ctrl Pts',(-4.02236168477261,-5.44495098921234,
15.9946570807899));
#12689=CARTESIAN_POINT('Ctrl Pts',(-3.87112305634355,-5.55349359238818,
16.0034062260579));
#12690=CARTESIAN_POINT('Ctrl Pts',(-3.71567117316642,-5.65562346102533,
16.0121553713258));
#12691=CARTESIAN_POINT('Ctrl Pts',(-3.56021980457218,-5.7577529915882,16.0209044876319));
#12692=CARTESIAN_POINT('Ctrl Pts',(-3.40055544862314,-5.85346967275396,
16.0296536039381));
#12693=CARTESIAN_POINT('Ctrl Pts',(-3.23722036323339,-5.94244842803596,
16.0384027202442));
#12694=CARTESIAN_POINT('Ctrl Pts',(-3.0738858049597,-6.03142689616515,16.0471518083152));
#12695=CARTESIAN_POINT('Ctrl Pts',(-2.90688079257619,-6.11366734484865,
16.0559008963862));
#12696=CARTESIAN_POINT('Ctrl Pts',(-2.73677251094514,-6.18889046787347,
16.0646499844571));
#12697=CARTESIAN_POINT('Ctrl Pts',(-2.56666476416559,-6.26411335438305,
16.0733990450193));
#12698=CARTESIAN_POINT('Ctrl Pts',(-2.39345402972023,-6.33231884350316,
16.0821481055815));
#12699=CARTESIAN_POINT('Ctrl Pts',(-2.21772856473985,-6.39327529621062,
16.0908971661438));
#12700=CARTESIAN_POINT('Ctrl Pts',(-2.04200363768211,-6.454231562321,16.0996461999238));
#12701=CARTESIAN_POINT('Ctrl Pts',(-1.8637642662003,-6.50793874252074,16.1083952337038));
#12702=CARTESIAN_POINT('Ctrl Pts',(-1.6836157819462,-6.5542144379614,16.1171442674838));
#12703=CARTESIAN_POINT('Ctrl Pts',(-1.50346783419814,-6.60048999558692,
16.125893275208));
#12704=CARTESIAN_POINT('Ctrl Pts',(-1.32141106257207,-6.63933404145503,
16.1346422829322));
#12705=CARTESIAN_POINT('Ctrl Pts',(-1.13806375959019,-6.67061465527034,
16.1433912906564));
#12706=CARTESIAN_POINT('Ctrl Pts',(-0.954716987418967,-6.70189517852483,
16.1521402730513));
#12707=CARTESIAN_POINT('Ctrl Pts',(-0.77007997380976,-6.72561226535829,
16.1608892554462));
#12708=CARTESIAN_POINT('Ctrl Pts',(-0.584779770552411,-6.74168536939782,
16.1696382378411));
#12709=CARTESIAN_POINT('Ctrl Pts',(-0.391490647553874,-6.75845143942394,
16.1787644185171));
#12710=CARTESIAN_POINT('Ctrl Pts',(-0.197480213104304,-6.76689975924027,
16.1878905991932));
#12711=CARTESIAN_POINT('Ctrl Pts',(-0.00346532629777421,-6.76699911271707,
16.1970167798692));
#12712=CARTESIAN_POINT('Ctrl Pts',(0.184486595296051,-6.76709536139773,
16.2058577673992));
#12713=CARTESIAN_POINT('Ctrl Pts',(0.372442378185195,-6.7593565972677,16.2146987549291));
#12714=CARTESIAN_POINT('Ctrl Pts',(0.559750217722025,-6.74380965729017,
16.223539742459));
#12715=CARTESIAN_POINT('Ctrl Pts',(0.745129914457625,-6.72842275717255,
16.2322897210568));
#12716=CARTESIAN_POINT('Ctrl Pts',(0.929874656313991,-6.70538772273475,
16.2410396996546));
#12717=CARTESIAN_POINT('Ctrl Pts',(1.11335688289751,-6.67478280180747,16.2497896782523));
#12718=CARTESIAN_POINT('Ctrl Pts',(1.29683723118834,-6.64417819418028,16.2585395672773));
#12719=CARTESIAN_POINT('Ctrl Pts',(1.47905480730217,-6.60600390230079,16.2672894563022));
#12720=CARTESIAN_POINT('Ctrl Pts',(1.65939064804794,-6.56038959797138,16.2760393453271));
#12721=CARTESIAN_POINT('Ctrl Pts',(1.83972470264254,-6.51477574543259,16.2847891476881));
#12722=CARTESIAN_POINT('Ctrl Pts',(2.0181767812584,-6.46172209820103,16.293538950049));
#12723=CARTESIAN_POINT('Ctrl Pts',(2.19414072347675,-6.40140886724016,16.30228875241));
#12724=CARTESIAN_POINT('Ctrl Pts',(2.37010298132085,-6.34109621361378,16.3110384710155));
#12725=CARTESIAN_POINT('Ctrl Pts',(2.54357687926895,-6.27352420825978,16.319788189621));
#12726=CARTESIAN_POINT('Ctrl Pts',(2.71397317789947,-6.19892237325507,16.3285379082264));
#12727=CARTESIAN_POINT('Ctrl Pts',(2.88436790207177,-6.12432122756975,16.3372875459847));
#12728=CARTESIAN_POINT('Ctrl Pts',(3.05168482126232,-6.04269049717429,16.346037183743));
#12729=CARTESIAN_POINT('Ctrl Pts',(3.21535561997365,-5.95430745234942,16.3547868215012));
#12730=CARTESIAN_POINT('Ctrl Pts',(3.37902496075253,-5.86592519481532,16.3635363813203));
#12731=CARTESIAN_POINT('Ctrl Pts',(3.53904799384844,-5.77079087940251,16.3722859411393));
#12732=CARTESIAN_POINT('Ctrl Pts',(3.6948811881495,-5.66922763747047,16.3810355009583));
#12733=CARTESIAN_POINT('Ctrl Pts',(3.85071304610794,-5.56766526649079,16.3897849857457));
#12734=CARTESIAN_POINT('Ctrl Pts',(4.00235489705925,-5.45967423580745,16.3985344705331));
#12735=CARTESIAN_POINT('Ctrl Pts',(4.14929168607607,-5.34562133936365,16.4072839553206));
#12736=CARTESIAN_POINT('Ctrl Pts',(4.2962272638571,-5.2315693830857,16.4160333679839));
#12737=CARTESIAN_POINT('Ctrl Pts',(4.4384576309202,-5.11145583677243,16.4247827806472));
#12738=CARTESIAN_POINT('Ctrl Pts',(4.57549970660915,-4.98568866204255,16.4335321933105));
#12739=CARTESIAN_POINT('Ctrl Pts',(4.71254069815248,-4.85992248226207,16.4422815367568));
#12740=CARTESIAN_POINT('Ctrl Pts',(4.84439326931267,-4.72850295734051,16.4510308802031));
#12741=CARTESIAN_POINT('Ctrl Pts',(4.97060959434651,-4.59187644221732,16.4597802236495));
#12742=CARTESIAN_POINT('Ctrl Pts',(5.09682496280474,-4.45525096256711,16.4685295007858));
#12743=CARTESIAN_POINT('Ctrl Pts',(5.21740397615804,-4.31341878218369,16.4772787779221));
#12744=CARTESIAN_POINT('Ctrl Pts',(5.33193710451904,-4.16686161438716,16.4860280550583));
#12745=CARTESIAN_POINT('Ctrl Pts',(5.4464694028936,-4.02030550864546,16.4947772687913));
#12746=CARTESIAN_POINT('Ctrl Pts',(5.55495572749648,-3.86902470980158,16.5035264825243));
#12747=CARTESIAN_POINT('Ctrl Pts',(5.65702762491445,-3.71353301465798,16.5122756962573));
#12748=CARTESIAN_POINT('Ctrl Pts',(5.75909881655151,-3.55804239466898,16.5210248494934));
#12749=CARTESIAN_POINT('Ctrl Pts',(5.85475551250787,-3.39834117619546,16.5297740027295));
#12750=CARTESIAN_POINT('Ctrl Pts',(5.94367283728105,-3.2349717469195,16.5385231559656));
#12751=CARTESIAN_POINT('Ctrl Pts',(6.03258957676328,-3.07160339300933,16.5472722516112));
#12752=CARTESIAN_POINT('Ctrl Pts',(6.11476689685307,-2.90456712829458,16.5560213472567));
#12753=CARTESIAN_POINT('Ctrl Pts',(6.18992570525288,-2.73443024475844,16.5647704429022));
#12754=CARTESIAN_POINT('Ctrl Pts',(6.26508404388724,-2.56429442462965,16.5735194838633));
#12755=CARTESIAN_POINT('Ctrl Pts',(6.33322384283341,-2.39105828655925,16.5822685248243));
#12756=CARTESIAN_POINT('Ctrl Pts',(6.39411368720057,-2.2153101713201,16.5910175657853));
#12757=CARTESIAN_POINT('Ctrl Pts',(6.4550031712091,-2.0395630961945,16.5997665549677));
#12758=CARTESIAN_POINT('Ctrl Pts',(6.5086426927009,-1.86130434438574,16.6085155441501));
#12759=CARTESIAN_POINT('Ctrl Pts',(6.55485008446347,-1.68113930719892,16.6172645333325));
#12760=CARTESIAN_POINT('Ctrl Pts',(6.60199664749416,-1.49731239211787,16.6261913468619));
#12761=CARTESIAN_POINT('Ctrl Pts',(6.64140563640917,-1.31150116499617,16.6351181603913));
#12762=CARTESIAN_POINT('Ctrl Pts',(6.67293772282181,-1.12436255155606,16.6440449739206));
#12763=CARTESIAN_POINT('Ctrl Pts',(6.70384494949879,-0.940932395050799,
16.6527948880762));
#12764=CARTESIAN_POINT('Ctrl Pts',(6.72718449348936,-0.756227260506168,
16.6615448022317));
#12765=CARTESIAN_POINT('Ctrl Pts',(6.74287707373937,-0.570874564541144,
16.6702947163872));
#12766=CARTESIAN_POINT('Ctrl Pts',(6.75856934538673,-0.385525513631947,
16.6790444584712));
#12767=CARTESIAN_POINT('Ctrl Pts',(6.76661493004104,-0.19952921241772,16.6877942005552));
#12768=CARTESIAN_POINT('Ctrl Pts',(6.76698649908907,-0.0135174385999383,
16.6965439426391));
#12769=CARTESIAN_POINT('Ctrl Pts',(6.76735806132388,0.172490924446294,16.705293524285));
#12770=CARTESIAN_POINT('Ctrl Pts',(6.76005588896286,0.358514472901948,16.7140431059309));
#12771=CARTESIAN_POINT('Ctrl Pts',(6.7451047845458,0.543921359662778,16.7227926875768));
#12772=CARTESIAN_POINT('Ctrl Pts',(6.73015393440681,0.729325093151046,16.7315421204159));
#12773=CARTESIAN_POINT('Ctrl Pts',(6.70755443556889,0.914111900256987,16.7402915532549));
#12774=CARTESIAN_POINT('Ctrl Pts',(6.67738304682308,1.09765415591605,16.749040986094));
#12775=CARTESIAN_POINT('Ctrl Pts',(6.64721213111846,1.28119353391347,16.7577902817553));
#12776=CARTESIAN_POINT('Ctrl Pts',(6.60946960955476,1.46348811672734,16.7665395774166));
#12777=CARTESIAN_POINT('Ctrl Pts',(6.56428366991161,1.6439187634831,16.775288873078));
#12778=CARTESIAN_POINT('Ctrl Pts',(6.51909837867692,1.82434682109806,16.7840380431888));
#12779=CARTESIAN_POINT('Ctrl Pts',(6.46646995271892,2.00291071820538,16.7927872132996));
#12780=CARTESIAN_POINT('Ctrl Pts',(6.40657713281517,2.17900400212799,16.8015363834104));
#12781=CARTESIAN_POINT('Ctrl Pts',(6.34668509279023,2.35509499309758,16.8102854395962));
#12782=CARTESIAN_POINT('Ctrl Pts',(6.27952894037484,2.52871516398226,16.819034495782));
#12783=CARTESIAN_POINT('Ctrl Pts',(6.205336750614,2.69927486771527,16.8277835519678));
#12784=CARTESIAN_POINT('Ctrl Pts',(6.12832117907871,2.87632521636021,16.83686555325));
#12785=CARTESIAN_POINT('Ctrl Pts',(6.04372366626034,3.05007728920086,16.8459475545323));
#12786=CARTESIAN_POINT('Ctrl Pts',(5.95185378007825,3.21989527478275,16.8550295558146));
#12787=CARTESIAN_POINT('Ctrl Pts',(5.86334450817326,3.3835012928683,16.8637793361217));
#12788=CARTESIAN_POINT('Ctrl Pts',(5.76808562057208,3.54345567125039,16.8725291164288));
#12789=CARTESIAN_POINT('Ctrl Pts',(5.66640068804435,3.69921508465385,16.8812788967359));
#12790=CARTESIAN_POINT('Ctrl Pts',(5.56471941107871,3.85496889852359,16.8900283624894));
#12791=CARTESIAN_POINT('Ctrl Pts',(5.45661270815058,4.00652780919714,16.8987778282429));
#12792=CARTESIAN_POINT('Ctrl Pts',(5.34244776449054,4.15337704569306,16.9075272939964));
#12793=CARTESIAN_POINT('Ctrl Pts',(5.22828631819538,4.30022178356319,16.916276491716));
#12794=CARTESIAN_POINT('Ctrl Pts',(5.10806717844015,4.4423569097274,16.9250256894356));
#12795=CARTESIAN_POINT('Ctrl Pts',(4.98219864544669,4.57929969070699,16.9337748871552));
#12796=CARTESIAN_POINT('Ctrl Pts',(4.85633329943964,4.71623900430064,16.9425238633454));
#12797=CARTESIAN_POINT('Ctrl Pts',(4.72481904033576,4.84798602483688,16.9512728395357));
#12798=CARTESIAN_POINT('Ctrl Pts',(4.58810250737114,4.97409332259204,16.9600218157259));
#12799=CARTESIAN_POINT('Ctrl Pts',(4.4513770868555,5.10020881822216,16.9687713606621));
#12800=CARTESIAN_POINT('Ctrl Pts',(4.30944892635952,5.22068366308015,16.9775209055983));
#12801=CARTESIAN_POINT('Ctrl Pts',(4.16280009466554,5.33510865604934,16.9862704505345));
#12802=CARTESIAN_POINT('Ctrl Pts',(4.01615988348669,5.4495269227298,16.9950194811427));
#12803=CARTESIAN_POINT('Ctrl Pts',(3.86479978232097,5.5578958728872,17.003768511751));
#12804=CARTESIAN_POINT('Ctrl Pts',(3.7092338358092,5.65984746713974,17.0125175423593));
#12805=CARTESIAN_POINT('Ctrl Pts',(3.55366577799386,5.76180044505479,17.0212666917073));
#12806=CARTESIAN_POINT('Ctrl Pts',(3.39389200026678,5.85733573571153,17.0300158410554));
#12807=CARTESIAN_POINT('Ctrl Pts',(3.23045513625871,5.9461288762202,17.0387649904034));
#12808=CARTESIAN_POINT('Ctrl Pts',(3.18695122151465,5.96976399206748,17.0410938545163));
#12809=CARTESIAN_POINT('Ctrl Pts',(3.14318791262608,5.99292165435362,17.0434227186293));
#12810=CARTESIAN_POINT('Ctrl Pts',(3.0991757505326,6.01559628526638,17.0457515827422));
#12811=CARTESIAN_POINT('Ctrl Pts',(3.09917575053257,6.0155962852664,15.0458593505058));
#12812=CARTESIAN_POINT('Ctrl Pts',(2.93718592831312,6.09905184063424,15.0544103860842));
#12813=CARTESIAN_POINT('Ctrl Pts',(2.77176774995393,6.17598800827926,15.0629614216626));
#12814=CARTESIAN_POINT('Ctrl Pts',(2.60349464973925,6.24612716879661,15.071512457241));
#12815=CARTESIAN_POINT('Ctrl Pts',(2.44214626671966,6.31337998651606,15.0797116035215));
#12816=CARTESIAN_POINT('Ctrl Pts',(2.27817359794682,6.37438389895123,15.0879107498019));
#12817=CARTESIAN_POINT('Ctrl Pts',(2.11210332844844,6.42894303365312,15.0961098960823));
#12818=CARTESIAN_POINT('Ctrl Pts',(1.9460151590607,6.48350804901311,15.104309926108));
#12819=CARTESIAN_POINT('Ctrl Pts',(1.77782927902566,6.53162679041381,15.1125099561337));
#12820=CARTESIAN_POINT('Ctrl Pts',(1.60808817656457,6.57315308024948,15.1207099861594));
#12821=CARTESIAN_POINT('Ctrl Pts',(1.43829798567515,6.6146913793173,15.1289123876));
#12822=CARTESIAN_POINT('Ctrl Pts',(1.26695202452738,6.6496333437127,15.1371147890406));
#12823=CARTESIAN_POINT('Ctrl Pts',(1.09460368215074,6.67788377998764,15.1453171904812));
#12824=CARTESIAN_POINT('Ctrl Pts',(0.922174230900824,6.70614751120366,15.1535234520549));
#12825=CARTESIAN_POINT('Ctrl Pts',(0.748741812018114,6.72771338321376,15.1617297136286));
#12826=CARTESIAN_POINT('Ctrl Pts',(0.57486570941015,6.74253798032643,15.1699359752023));
#12827=CARTESIAN_POINT('Ctrl Pts',(0.4007841667395,6.75738009316503,15.1781519327311));
#12828=CARTESIAN_POINT('Ctrl Pts',(0.226258250536156,6.76546499416257,15.18636789026));
#12829=CARTESIAN_POINT('Ctrl Pts',(0.0518489695518635,6.76680136285649,
15.1945838477888));
#12830=CARTESIAN_POINT('Ctrl Pts',(-0.122681401712306,6.76813865937523,
15.2028055095588));
#12831=CARTESIAN_POINT('Ctrl Pts',(-0.297094619409528,6.76271809633917,
15.2110271713288));
#12832=CARTESIAN_POINT('Ctrl Pts',(-0.470834143085268,6.750600285138,15.2192488330988));
#12833=CARTESIAN_POINT('Ctrl Pts',(-0.644813884131266,6.73846571949501,
15.22748186238));
#12834=CARTESIAN_POINT('Ctrl Pts',(-0.818117716461157,6.71961545386714,
15.2357148916611));
#12835=CARTESIAN_POINT('Ctrl Pts',(-0.99019775338741,6.69416144182276,15.2439479209422));
#12836=CARTESIAN_POINT('Ctrl Pts',(-1.03991667121275,6.68680703886141,15.2463266820908));
#12837=CARTESIAN_POINT('Ctrl Pts',(-1.08953351489694,6.67890167599312,15.2487054432393));
#12838=CARTESIAN_POINT('Ctrl Pts',(-1.13903530317154,6.6704488288367,15.2510842043879));
#12839=CARTESIAN_POINT('Ctrl Pts',(-1.30871700656454,6.64147424925049,15.2592380965546));
#12840=CARTESIAN_POINT('Ctrl Pts',(-1.47757036354887,6.60597347987454,15.2673919887213));
#12841=CARTESIAN_POINT('Ctrl Pts',(-1.64504892350012,6.56400053620436,15.2755458808881));
#12842=CARTESIAN_POINT('Ctrl Pts',(-1.81232311281691,6.52207881125214,15.2836898230283));
#12843=CARTESIAN_POINT('Ctrl Pts',(-1.97822549371729,6.47370072081307,15.2918337651685));
#12844=CARTESIAN_POINT('Ctrl Pts',(-2.14221597580984,6.41897185793684,15.2999777073087));
#12845=CARTESIAN_POINT('Ctrl Pts',(-2.30604086042381,6.36429826022955,15.3081134257016));
#12846=CARTESIAN_POINT('Ctrl Pts',(-2.46795734550539,6.30328677200131,15.3162491440945));
#12847=CARTESIAN_POINT('Ctrl Pts',(-2.62743676387958,6.23609373340507,15.3243848624874));
#12848=CARTESIAN_POINT('Ctrl Pts',(-2.78678868657676,6.16895441222286,15.3325140767876));
#12849=CARTESIAN_POINT('Ctrl Pts',(-2.9437070864688,6.09564352169102,15.3406432910878));
#12850=CARTESIAN_POINT('Ctrl Pts',(-3.09767967482999,6.0163668132973,15.3487725053879));
#12851=CARTESIAN_POINT('Ctrl Pts',(-3.25156154459385,5.93713681368379,15.3568969300634));
#12852=CARTESIAN_POINT('Ctrl Pts',(-3.40250073499562,5.85194816311061,15.3650213547388));
#12853=CARTESIAN_POINT('Ctrl Pts',(-3.55000613246669,5.76105419688523,15.3731457794143));
#12854=CARTESIAN_POINT('Ctrl Pts',(-3.69840698212802,5.66960844609784,15.3813195245484));
#12855=CARTESIAN_POINT('Ctrl Pts',(-3.84333186589893,5.57238802888942,15.3894932696826));
#12856=CARTESIAN_POINT('Ctrl Pts',(-3.98430646117621,5.46969752577138,15.3976670148168));
#12857=CARTESIAN_POINT('Ctrl Pts',(-4.12437829639739,5.36766462258596,15.405788417679));
#12858=CARTESIAN_POINT('Ctrl Pts',(-4.26055000252925,5.26023172297751,15.4139098205411));
#12859=CARTESIAN_POINT('Ctrl Pts',(-4.3923863096306,5.14774042731077,15.4220312234033));
#12860=CARTESIAN_POINT('Ctrl Pts',(-4.52423280962096,5.03524043440944,15.4301532541695));
#12861=CARTESIAN_POINT('Ctrl Pts',(-4.65174296446796,4.91768150396285,15.4382752849358));
#12862=CARTESIAN_POINT('Ctrl Pts',(-4.77451564793939,4.79544464336541,15.446397315702));
#12863=CARTESIAN_POINT('Ctrl Pts',(-4.89732120230261,4.67317505533621,15.4545215210431));
#12864=CARTESIAN_POINT('Ctrl Pts',(-5.01538650043006,4.54622530140399,15.4626457263843));
#12865=CARTESIAN_POINT('Ctrl Pts',(-5.12834828740515,4.41501221324117,15.4707699317254));
#12866=CARTESIAN_POINT('Ctrl Pts',(-5.24253280756064,4.28237883419153,15.4789820759679));
#12867=CARTESIAN_POINT('Ctrl Pts',(-5.3515024361904,4.14538957662682,15.4871942202103));
#12868=CARTESIAN_POINT('Ctrl Pts',(-5.45492525077838,4.00450739897186,15.4954063644527));
#12869=CARTESIAN_POINT('Ctrl Pts',(-5.55740392905579,3.86491132032675,15.5035435408692));
#12870=CARTESIAN_POINT('Ctrl Pts',(-5.65443649180515,3.72149344011123,15.5116807172856));
#12871=CARTESIAN_POINT('Ctrl Pts',(-5.74574511586462,3.57473104771784,15.5198178937021));
#12872=CARTESIAN_POINT('Ctrl Pts',(-5.8383155797852,3.42594047191086,15.5280675218575));
#12873=CARTESIAN_POINT('Ctrl Pts',(-5.92500254830411,3.27371260902382,15.5363171500129));
#12874=CARTESIAN_POINT('Ctrl Pts',(-6.00556614100093,3.11856767219555,15.5445667781684));
#12875=CARTESIAN_POINT('Ctrl Pts',(-6.08612973369775,2.9634227353673,15.5528164063238));
#12876=CARTESIAN_POINT('Ctrl Pts',(-6.16056984386216,2.80536109965522,15.5610660344792));
#12877=CARTESIAN_POINT('Ctrl Pts',(-6.22869846988963,2.64492048485292,15.5693156626347));
#12878=CARTESIAN_POINT('Ctrl Pts',(-6.30473358197508,2.46586036224554,15.5785226793916));
#12879=CARTESIAN_POINT('Ctrl Pts',(-6.37310104231516,2.28338407206856,15.5877296961485));
#12880=CARTESIAN_POINT('Ctrl Pts',(-6.43351813430323,2.09812616770096,15.5969367129054));
#12881=CARTESIAN_POINT('Ctrl Pts',(-6.49368700921999,1.91362937534562,15.6061059036323));
#12882=CARTESIAN_POINT('Ctrl Pts',(-6.54597060928338,1.72637396026775,15.6152750943593));
#12883=CARTESIAN_POINT('Ctrl Pts',(-6.59013575359022,1.53701000297717,15.6244442850862));
#12884=CARTESIAN_POINT('Ctrl Pts',(-6.63418090021955,1.34816055176226,15.6335885629183));
#12885=CARTESIAN_POINT('Ctrl Pts',(-6.6701515417064,1.15721418325689,15.6427328407505));
#12886=CARTESIAN_POINT('Ctrl Pts',(-6.69786384472593,0.964836212791147,
15.6518771185827));
#12887=CARTESIAN_POINT('Ctrl Pts',(-6.72544643478091,0.773358705807173,
15.6609785947976));
#12888=CARTESIAN_POINT('Ctrl Pts',(-6.74484773035244,0.580463161232371,
15.6700800710125));
#12889=CARTESIAN_POINT('Ctrl Pts',(-6.75593493639542,0.386823131665841,
15.6791815472275));
#12890=CARTESIAN_POINT('Ctrl Pts',(-6.7632432804006,0.259181601080143,15.6851809594216));
#12891=CARTESIAN_POINT('Ctrl Pts',(-6.76694011348344,0.131216943220901,
15.6911803716158));
#12892=CARTESIAN_POINT('Ctrl Pts',(-6.76699927814238,0.00312563922654881,
15.69717978381));
#12893=CARTESIAN_POINT('',(-6.767,1.40905773919446E-12,15.3028202161899));
#12894=CARTESIAN_POINT('Ctrl Pts',(3.09917575053259,6.01559628526639,14.6513920151221));
#12895=CARTESIAN_POINT('Ctrl Pts',(2.93382384459265,6.1007839529376,14.6601414630345));
#12896=CARTESIAN_POINT('Ctrl Pts',(2.76495772122983,6.17915010267049,14.6688909109469));
#12897=CARTESIAN_POINT('Ctrl Pts',(2.5931509331671,6.25042856433178,14.6776403588593));
#12898=CARTESIAN_POINT('Ctrl Pts',(2.42134553245609,6.32170645041454,14.6863897361193));
#12899=CARTESIAN_POINT('Ctrl Pts',(2.24659977927575,6.38589665313463,14.6951391133793));
#12900=CARTESIAN_POINT('Ctrl Pts',(2.06950718689896,6.44278115439083,14.7038884906393));
#12901=CARTESIAN_POINT('Ctrl Pts',(1.89241596572829,6.49966521519734,14.712637800154));
#12902=CARTESIAN_POINT('Ctrl Pts',(1.71297821457156,6.54924360009557,14.7213871096687));
#12903=CARTESIAN_POINT('Ctrl Pts',(1.53180337335793,6.59134792173568,14.7301364191833));
#12904=CARTESIAN_POINT('Ctrl Pts',(1.35062987477741,6.63345193135313,14.7388856638594));
#12905=CARTESIAN_POINT('Ctrl Pts',(1.1677195910292,6.66808192368243,14.7476349085356));
#12906=CARTESIAN_POINT('Ctrl Pts',(0.983693746906624,6.69512028363172,14.7563841532117));
#12907=CARTESIAN_POINT('Ctrl Pts',(0.799669205419539,6.72215845218871,14.7651333359559));
#12908=CARTESIAN_POINT('Ctrl Pts',(0.614529402873032,6.74160505424583,14.7738825187));
#12909=CARTESIAN_POINT('Ctrl Pts',(0.428903127362691,6.75339404354126,14.7826317014442));
#12910=CARTESIAN_POINT('Ctrl Pts',(0.243278104163457,6.76518295330331,14.7913808251628));
#12911=CARTESIAN_POINT('Ctrl Pts',(0.0571669005388305,6.76931433552276,
14.8001299488814));
#12912=CARTESIAN_POINT('Ctrl Pts',(-0.128798404777664,6.76577415902473,
14.8088790726));
#12913=CARTESIAN_POINT('Ctrl Pts',(-0.314762517259084,6.76223400523441,
14.8176281401992));
#12914=CARTESIAN_POINT('Ctrl Pts',(-0.500580446819331,6.7510223966509,14.8263772077984));
#12915=CARTESIAN_POINT('Ctrl Pts',(-0.685621118842269,6.73217741012501,
14.8351262753976));
#12916=CARTESIAN_POINT('Ctrl Pts',(-0.870660665414322,6.71333253821774,
14.8438752897834));
#12917=CARTESIAN_POINT('Ctrl Pts',(-1.05492267885487,6.68685441030612,14.8526243041692));
#12918=CARTESIAN_POINT('Ctrl Pts',(-1.2377813763527,6.65283295028174,14.861373318555));
#12919=CARTESIAN_POINT('Ctrl Pts',(-1.42999922978867,6.61707018861861,14.8705701289224));
#12920=CARTESIAN_POINT('Ctrl Pts',(-1.62066601233717,6.57297172934408,14.8797669392898));
#12921=CARTESIAN_POINT('Ctrl Pts',(-1.80906628500409,6.52070304311288,14.8889637496572));
#12922=CARTESIAN_POINT('Ctrl Pts',(-1.98831342545549,6.47097374915024,14.8977137473949));
#12923=CARTESIAN_POINT('Ctrl Pts',(-2.16550875896722,6.41384933989522,14.9064637451327));
#12924=CARTESIAN_POINT('Ctrl Pts',(-2.34005036714029,6.34952386240469,14.9152137428705));
#12925=CARTESIAN_POINT('Ctrl Pts',(-2.51458843547104,6.2851996894859,14.9239635631513));
#12926=CARTESIAN_POINT('Ctrl Pts',(-2.68647261718067,6.21367483971094,14.9327133834322));
#12927=CARTESIAN_POINT('Ctrl Pts',(-2.8551190590874,6.13519226743839,14.941463203713));
#12928=CARTESIAN_POINT('Ctrl Pts',(-3.02376230488892,6.05671118252933,14.9502128581716));
#12929=CARTESIAN_POINT('Ctrl Pts',(-3.18916767379911,5.97127275992629,14.9589625126301));
#12930=CARTESIAN_POINT('Ctrl Pts',(-3.35077334102793,5.87916720437993,14.9677121670886));
#12931=CARTESIAN_POINT('Ctrl Pts',(-3.51237616037376,5.78706327195638,14.9764616673571));
#12932=CARTESIAN_POINT('Ctrl Pts',(-3.6701791630231,5.68829258362292,14.9852111676255));
#12933=CARTESIAN_POINT('Ctrl Pts',(-3.82364636566474,5.58319061741034,14.993960667894));
#12934=CARTESIAN_POINT('Ctrl Pts',(-3.9771110677882,5.47809036367686,15.0027100256024));
#12935=CARTESIAN_POINT('Ctrl Pts',(-4.12623987481959,5.36665920043201,15.0114593833109));
#12936=CARTESIAN_POINT('Ctrl Pts',(-4.27052628213971,5.24927559512301,15.0202087410193));
#12937=CARTESIAN_POINT('Ctrl Pts',(-4.41481053025021,5.13189374643,15.0289579677958));
#12938=CARTESIAN_POINT('Ctrl Pts',(-4.55425230136573,5.00855981477314,15.0377071945723));
#12939=CARTESIAN_POINT('Ctrl Pts',(-4.68837800630592,4.87969268192035,15.0464564213489));
#12940=CARTESIAN_POINT('Ctrl Pts',(-4.82250188228941,4.75082730631762,15.0552055288197));
#12941=CARTESIAN_POINT('Ctrl Pts',(-4.95130963053016,4.61642907903473,15.0639546362906));
#12942=CARTESIAN_POINT('Ctrl Pts',(-5.07436379033419,4.4769544473163,15.0727037437614));
#12943=CARTESIAN_POINT('Ctrl Pts',(-5.19741643562879,4.33748153220499,15.0814527435512));
#12944=CARTESIAN_POINT('Ctrl Pts',(-5.31471544462867,4.19293255254472,15.0902017433409));
#12945=CARTESIAN_POINT('Ctrl Pts',(-5.42586245275738,4.04379841779454,15.0989507431307));
#12946=CARTESIAN_POINT('Ctrl Pts',(-5.53702160019253,3.894647994842,15.1077006984728));
#12947=CARTESIAN_POINT('Ctrl Pts',(-5.64202723081341,3.74091164443714,15.116450653815));
#12948=CARTESIAN_POINT('Ctrl Pts',(-5.74052265233047,3.58311159163104,15.1252006091571));
#12949=CARTESIAN_POINT('Ctrl Pts',(-5.83901427066998,3.42531763191648,15.1339502266396));
#12950=CARTESIAN_POINT('Ctrl Pts',(-5.93099603115819,3.26346052695469,15.142699844122));
#12951=CARTESIAN_POINT('Ctrl Pts',(-6.01615550622831,3.09809004466925,15.1514494616045));
#12952=CARTESIAN_POINT('Ctrl Pts',(-6.10131214578871,2.93272506863679,15.1601987877556));
#12953=CARTESIAN_POINT('Ctrl Pts',(-6.17964682328813,2.76384720416748,15.1689481139067));
#12954=CARTESIAN_POINT('Ctrl Pts',(-6.25089348288623,2.5920300279145,15.1776974400578));
#12955=CARTESIAN_POINT('Ctrl Pts',(-6.3221381488939,2.42021765936873,15.1864465213893));
#12956=CARTESIAN_POINT('Ctrl Pts',(-6.38629508412645,2.24546640831749,15.1951956027209));
#12957=CARTESIAN_POINT('Ctrl Pts',(-6.4431463981987,2.0683697665986,15.2039446840525));
#12958=CARTESIAN_POINT('Ctrl Pts',(-6.50000285283755,1.89125711158087,15.2126945564869));
#12959=CARTESIAN_POINT('Ctrl Pts',(-6.549552276733,1.7117989144006,15.2214444289213));
#12960=CARTESIAN_POINT('Ctrl Pts',(-6.59162635926432,1.5306047627823,15.2301943013557));
#12961=CARTESIAN_POINT('Ctrl Pts',(-6.63369752055237,1.34942319164494,15.2389435662782));
#12962=CARTESIAN_POINT('Ctrl Pts',(-6.66829431424289,1.16650618642502,15.2476928312007));
#12963=CARTESIAN_POINT('Ctrl Pts',(-6.69529923745447,0.982474997616538,
15.2564420961232));
#12964=CARTESIAN_POINT('Ctrl Pts',(-6.72230554731468,0.798434359175698,
15.2651918103029));
#12965=CARTESIAN_POINT('Ctrl Pts',(-6.74171916496722,0.613279706238272,
15.2739415244826));
#12966=CARTESIAN_POINT('Ctrl Pts',(-6.75347414817288,0.427639953653293,
15.2826912386623));
#12967=CARTESIAN_POINT('Ctrl Pts',(-6.76248837758749,0.285283364197127,
15.2894008978382));
#12968=CARTESIAN_POINT('Ctrl Pts',(-6.76699999999997,0.142641701104314,
15.296110557014));
#12969=CARTESIAN_POINT('Ctrl Pts',(-6.767,1.40905773244098E-12,15.3028202161899));
#12970=CARTESIAN_POINT('Ctrl Pts',(-6.76699999999571,7.62476850229202E-6,
15.3029847694131));
#12971=CARTESIAN_POINT('Ctrl Pts',(-6.76700019411946,-0.172277660166757,
15.3111106415999));
#12972=CARTESIAN_POINT('Ctrl Pts',(-6.76041659476757,-0.344787798069247,
15.3192365137866));
#12973=CARTESIAN_POINT('Ctrl Pts',(-6.74722363853828,-0.516974053072598,
15.3273623859734));
#12974=CARTESIAN_POINT('Ctrl Pts',(-6.73404536197283,-0.688968718238338,
15.3354792165876));
#12975=CARTESIAN_POINT('Ctrl Pts',(-6.71427240758308,-0.860639854770346,
15.3435960472017));
#12976=CARTESIAN_POINT('Ctrl Pts',(-6.68793124167346,-1.03143817393389,
15.3517128778159));
#12977=CARTESIAN_POINT('Ctrl Pts',(-6.66160701719624,-1.20212664343523,
15.359824488056));
#12978=CARTESIAN_POINT('Ctrl Pts',(-6.62872304411251,-1.37194305151308,
15.3679360982962));
#12979=CARTESIAN_POINT('Ctrl Pts',(-6.58935768176897,-1.54034228070008,
15.3760477085364));
#12980=CARTESIAN_POINT('Ctrl Pts',(-6.5500114938191,-1.70865948465161,15.3841553677089));
#12981=CARTESIAN_POINT('Ctrl Pts',(-6.50419028646302,-1.87556052756818,
15.3922630268815));
#12982=CARTESIAN_POINT('Ctrl Pts',(-6.45202365964257,-2.04050966560134,
15.400370686054));
#12983=CARTESIAN_POINT('Ctrl Pts',(-6.42396699379531,-2.12922390935568,
15.4047312111267));
#12984=CARTESIAN_POINT('Ctrl Pts',(-6.39407573517589,-2.21737372715716,
15.4090917361994));
#12985=CARTESIAN_POINT('Ctrl Pts',(-6.36237607960498,-2.30487735501704,
15.4134522612721));
#12986=CARTESIAN_POINT('Ctrl Pts',(-6.2998876065227,-2.47737033627018,15.4220480188197));
#12987=CARTESIAN_POINT('Ctrl Pts',(-6.23041695127076,-2.64721938535274,
15.4306437763672));
#12988=CARTESIAN_POINT('Ctrl Pts',(-6.15422180419717,-2.81386619879911,
15.4392395339148));
#12989=CARTESIAN_POINT('Ctrl Pts',(-6.07795556446078,-2.98066849938828,
15.4478433115964));
#12990=CARTESIAN_POINT('Ctrl Pts',(-5.99495243636424,-3.14426232293631,
15.456447089278));
#12991=CARTESIAN_POINT('Ctrl Pts',(-5.90551624899013,-3.30411362288186,
15.4650508669597));
#12992=CARTESIAN_POINT('Ctrl Pts',(-5.81256514124534,-3.47024721869621,
15.4739927806277));
#12993=CARTESIAN_POINT('Ctrl Pts',(-5.71266529432935,-3.63233785090521,
15.4829346942957));
#12994=CARTESIAN_POINT('Ctrl Pts',(-5.60620673434045,-3.78981992340477,
15.4918766079637));
#12995=CARTESIAN_POINT('Ctrl Pts',(-5.50349499153471,-3.94175940228537,
15.5005038102944));
#12996=CARTESIAN_POINT('Ctrl Pts',(-5.3946785514444,-4.08940898011079,15.5091310126252));
#12997=CARTESIAN_POINT('Ctrl Pts',(-5.28014860639894,-4.23229484964639,
15.5177582149559));
#12998=CARTESIAN_POINT('Ctrl Pts',(-5.1655095891114,-4.37531679610183,15.5263936333763));
#12999=CARTESIAN_POINT('Ctrl Pts',(-5.04514640347598,-4.51356574672446,
15.5350290517967));
#13000=CARTESIAN_POINT('Ctrl Pts',(-4.91948832618044,-4.64660344860355,
15.5436644702171));
#13001=CARTESIAN_POINT('Ctrl Pts',(-4.79364460697371,-4.77983769473804,
15.5523126462383));
#13002=CARTESIAN_POINT('Ctrl Pts',(-4.66249057938801,-4.90784509112603,
15.5609608222594));
#13003=CARTESIAN_POINT('Ctrl Pts',(-4.52649100017713,-5.03022546466015,
15.5696089982805));
#13004=CARTESIAN_POINT('Ctrl Pts',(-4.51210276036556,-5.043172844151,15.5705239425123));
#13005=CARTESIAN_POINT('Ctrl Pts',(-4.49766031399888,-5.05605727968782,
15.5714388867441));
#13006=CARTESIAN_POINT('Ctrl Pts',(-4.48316423160408,-5.06887832488272,
15.5723538309759));
#13007=CARTESIAN_POINT('Ctrl Pts',(-4.35283424916889,-5.18414854407318,
15.5805798235173));
#13008=CARTESIAN_POINT('Ctrl Pts',(-4.21788464793136,-5.29454029992256,
15.5888058160586));
#13009=CARTESIAN_POINT('Ctrl Pts',(-4.0787157418761,-5.3996635910927,15.5970318086));
#13010=CARTESIAN_POINT('Ctrl Pts',(-3.93969273643064,-5.5046766740797,15.6052491772514));
#13011=CARTESIAN_POINT('Ctrl Pts',(-3.7964595183313,-5.60443207715044,15.6134665459028));
#13012=CARTESIAN_POINT('Ctrl Pts',(-3.64945163446743,-5.69857804787151,
15.6216839145542));
#13013=CARTESIAN_POINT('Ctrl Pts',(-3.5025684537276,-5.79264415691198,15.6298943126166));
#13014=CARTESIAN_POINT('Ctrl Pts',(-3.35191728437171,-5.88111011833935,
15.638104710679));
#13015=CARTESIAN_POINT('Ctrl Pts',(-3.19796507179745,-5.96366568475829,
15.6463151087414));
#13016=CARTESIAN_POINT('Ctrl Pts',(-3.0441126565521,-6.04616773570722,15.6545201845302));
#13017=CARTESIAN_POINT('Ctrl Pts',(-2.88696377514848,-6.12276685466356,
15.6627252603189));
#13018=CARTESIAN_POINT('Ctrl Pts',(-2.72701263461551,-6.19319716226178,
15.6709303361077));
#13019=CARTESIAN_POINT('Ctrl Pts',(-2.56713319011603,-6.26359590038401,
15.6791317340772));
#13020=CARTESIAN_POINT('Ctrl Pts',(-2.40445431618188,-6.32783119193416,
15.6873331320468));
#13021=CARTESIAN_POINT('Ctrl Pts',(-2.23949308261818,-6.3856839675093,15.6955345300163));
#13022=CARTESIAN_POINT('Ctrl Pts',(-2.07454477019234,-6.44353221157317,
15.703735285584));
#13023=CARTESIAN_POINT('Ctrl Pts',(-1.90731478917572,-6.49499880875938,
15.7119360411517));
#13024=CARTESIAN_POINT('Ctrl Pts',(-1.73833872868661,-6.53991341413235,
15.7201367967194));
#13025=CARTESIAN_POINT('Ctrl Pts',(-1.56936352651522,-6.58482779136056,
15.7283375106312));
#13026=CARTESIAN_POINT('Ctrl Pts',(-1.39864260861118,-6.6231901499759,15.736538224543));
#13027=CARTESIAN_POINT('Ctrl Pts',(-1.22672509711896,-6.65488050502024,
15.7447389384548));
#13028=CARTESIAN_POINT('Ctrl Pts',(-1.05477730315248,-6.68657644217401,
15.7529410968843));
#13029=CARTESIAN_POINT('Ctrl Pts',(-0.881632848106059,-6.7115979693203,
15.761143255314));
#13030=CARTESIAN_POINT('Ctrl Pts',(-0.70784943497986,-6.72987653507839,
15.7693454137436));
#13031=CARTESIAN_POINT('Ctrl Pts',(-0.534003916493984,-6.74816163308763,
15.7775505033965));
#13032=CARTESIAN_POINT('Ctrl Pts',(-0.359519341230758,-6.75969893188969,
15.7857555930495));
#13033=CARTESIAN_POINT('Ctrl Pts',(-0.184956958686212,-6.76447188799196,
15.7939606827024));
#13034=CARTESIAN_POINT('Ctrl Pts',(-0.010195159258519,-6.76925029663227,
15.8021751457002));
#13035=CARTESIAN_POINT('Ctrl Pts',(0.164644266426632,-6.76724891465809,
15.810389608698));
#13036=CARTESIAN_POINT('Ctrl Pts',(0.339000575769034,-6.75850335574588,
15.8186040716958));
#13037=CARTESIAN_POINT('Ctrl Pts',(0.513460185714212,-6.74975261536641,
15.8268234015032));
#13038=CARTESIAN_POINT('Ctrl Pts',(0.687435752389432,-6.73424976481487,
15.8350427313107));
#13039=CARTESIAN_POINT('Ctrl Pts',(0.860373328558443,-6.71208214606357,
15.8432620611182));
#13040=CARTESIAN_POINT('Ctrl Pts',(1.03357886101643,-6.68988017993104,15.8514941262789));
#13041=CARTESIAN_POINT('Ctrl Pts',(1.20574283576622,-6.6609928681763,15.8597261914396));
#13042=CARTESIAN_POINT('Ctrl Pts',(1.37632182357283,-6.62555863591571,15.8679582566003));
#13043=CARTESIAN_POINT('Ctrl Pts',(1.52965046605641,-6.59370780364248,15.8753578278614));
#13044=CARTESIAN_POINT('Ctrl Pts',(1.681698490314,-6.55656798282131,15.8827573991225));
#13045=CARTESIAN_POINT('Ctrl Pts',(1.83208365428045,-6.51427344250442,15.8901569703836));
#13046=CARTESIAN_POINT('Ctrl Pts',(1.99783108834764,-6.46765839519737,15.8983124287904));
#13047=CARTESIAN_POINT('Ctrl Pts',(2.16206861792596,-6.41463733580045,15.9064678871972));
#13048=CARTESIAN_POINT('Ctrl Pts',(2.32425831719805,-6.35532157132396,15.914623345604));
#13049=CARTESIAN_POINT('Ctrl Pts',(2.48625061028653,-6.29607800192981,15.9227688777459));
#13050=CARTESIAN_POINT('Ctrl Pts',(2.64619969496623,-6.23055510214892,15.9309144098877));
#13051=CARTESIAN_POINT('Ctrl Pts',(2.80357940658717,-6.15891479978091,15.9390599420296));
#13052=CARTESIAN_POINT('Ctrl Pts',(2.9608006602082,-6.08734662855935,15.9471972728302));
#13053=CARTESIAN_POINT('Ctrl Pts',(3.11545736081302,-6.00967346715305,15.9553346036308));
#13054=CARTESIAN_POINT('Ctrl Pts',(3.26704005016765,-5.92610650516852,15.9634719344313));
#13055=CARTESIAN_POINT('Ctrl Pts',(3.41850197383363,-5.84260612085031,15.9716027822333));
#13056=CARTESIAN_POINT('Ctrl Pts',(3.56689444403819,-5.75322146108041,15.9797336300353));
#13057=CARTESIAN_POINT('Ctrl Pts',(3.71172949390902,-5.65821112756019,15.9878644778373));
#13058=CARTESIAN_POINT('Ctrl Pts',(3.85647957903511,-5.5632565300565,15.9959905558312));
#13059=CARTESIAN_POINT('Ctrl Pts',(3.99767609498685,-5.462683031053,16.0041166338249));
#13060=CARTESIAN_POINT('Ctrl Pts',(4.13485714190466,-5.35679432273072,16.0122427118188));
#13061=CARTESIAN_POINT('Ctrl Pts',(4.2725246077595,-5.2505301523887,16.0203976034009));
#13062=CARTESIAN_POINT('Ctrl Pts',(4.40614775341956,-5.13891319492401,16.0285524949831));
#13063=CARTESIAN_POINT('Ctrl Pts',(4.53529003060481,-5.02229363322144,16.0367073865653));
#13064=CARTESIAN_POINT('Ctrl Pts',(4.66392869806236,-4.90612884703464,16.0448304769216));
#13065=CARTESIAN_POINT('Ctrl Pts',(4.78812112006629,-4.78500066295599,16.0529535672779));
#13066=CARTESIAN_POINT('Ctrl Pts',(4.90747012568906,-4.65929457809543,16.0610766576342));
#13067=CARTESIAN_POINT('Ctrl Pts',(5.02682850314064,-4.53357862221917,16.0692003858527));
#13068=CARTESIAN_POINT('Ctrl Pts',(5.14134245472424,-4.4032843147964,16.0773241140711));
#13069=CARTESIAN_POINT('Ctrl Pts',(5.2506528988365,-4.268832760362,16.0854478422895));
#13070=CARTESIAN_POINT('Ctrl Pts',(5.35999272268617,-4.13434506892903,16.0935737539498));
#13071=CARTESIAN_POINT('Ctrl Pts',(5.46412602358371,-3.99569818934985,16.1016996656102));
#13072=CARTESIAN_POINT('Ctrl Pts',(5.56273513898187,-3.85334488120858,16.1098255772705));
#13073=CARTESIAN_POINT('Ctrl Pts',(5.66197486992334,-3.71008120886424,16.1180034549806));
#13074=CARTESIAN_POINT('Ctrl Pts',(5.75561930076206,-3.56306384617776,16.1261813326906));
#13075=CARTESIAN_POINT('Ctrl Pts',(5.84339034310917,-3.41278160714372,16.1343592104007));
#13076=CARTESIAN_POINT('Ctrl Pts',(5.93074247330753,-3.26321663264238,16.1424980568741));
#13077=CARTESIAN_POINT('Ctrl Pts',(6.01227703902131,-3.11041823033074,16.1506369033476));
#13078=CARTESIAN_POINT('Ctrl Pts',(6.08776746412453,-2.95489023531277,16.158775749821));
#13079=CARTESIAN_POINT('Ctrl Pts',(6.16380093018369,-2.79824344846164,16.1669731431494));
#13080=CARTESIAN_POINT('Ctrl Pts',(6.23370281893999,-2.63882799611478,16.1751705364778));
#13081=CARTESIAN_POINT('Ctrl Pts',(6.29729218555359,-2.47717583747414,16.1833679298062));
#13082=CARTESIAN_POINT('Ctrl Pts',(6.3608815521672,-2.31552367883348,16.1915653231345));
#13083=CARTESIAN_POINT('Ctrl Pts',(6.41815833152117,-2.15163518545198,16.1997627164629));
#13084=CARTESIAN_POINT('Ctrl Pts',(6.46899361040797,-1.98605404470796,16.2079601097913));
#13085=CARTESIAN_POINT('Ctrl Pts',(6.52000758876355,-1.81989084240084,16.2161863191283));
#13086=CARTESIAN_POINT('Ctrl Pts',(6.5646866391576,-1.6515285750688,16.2244125284653));
#13087=CARTESIAN_POINT('Ctrl Pts',(6.60283827210986,-1.48149105713174,16.2326387378022));
#13088=CARTESIAN_POINT('Ctrl Pts',(6.64094704333687,-1.31164456906182,16.2408557053454));
#13089=CARTESIAN_POINT('Ctrl Pts',(6.67254292186017,-1.14012692486209,16.2490726728886));
#13090=CARTESIAN_POINT('Ctrl Pts',(6.69748267882117,-0.967478561462939,
16.2572896404318));
#13091=CARTESIAN_POINT('Ctrl Pts',(6.7223994226426,-0.794989509194642,16.2654990257752));
#13092=CARTESIAN_POINT('Ctrl Pts',(6.74067222583302,-0.621372168358847,
16.2737084111186));
#13093=CARTESIAN_POINT('Ctrl Pts',(6.75220853874428,-0.447178766612269,
16.2819177964619));
#13094=CARTESIAN_POINT('Ctrl Pts',(6.76373652121989,-0.27311115088884,16.2901212537625));
#13095=CARTESIAN_POINT('Ctrl Pts',(6.76853767897606,-0.0984686592113893,
16.2983247110631));
#13096=CARTESIAN_POINT('Ctrl Pts',(6.76657107691549,0.0761896387359722,
16.3065281683637));
#13097=CARTESIAN_POINT('Ctrl Pts',(6.76460550045366,0.250756850980788,16.3147273474956));
#13098=CARTESIAN_POINT('Ctrl Pts',(6.7558791994782,0.42533949531331,16.3229265266274));
#13099=CARTESIAN_POINT('Ctrl Pts',(6.7404032964622,0.599376677091736,16.3311257057593));
#13100=CARTESIAN_POINT('Ctrl Pts',(6.72493030943986,0.773381066514288,16.3393233399891));
#13101=CARTESIAN_POINT('Ctrl Pts',(6.70271027915053,0.946839840694611,16.3475209742189));
#13102=CARTESIAN_POINT('Ctrl Pts',(6.67380636065729,1.11919509490095,16.3557186084487));
#13103=CARTESIAN_POINT('Ctrl Pts',(6.64490452848054,1.29153790831627,16.3639156509642));
#13104=CARTESIAN_POINT('Ctrl Pts',(6.60931982737665,1.46277700650654,16.3721126934798));
#13105=CARTESIAN_POINT('Ctrl Pts',(6.56716691202784,1.63236262808443,16.3803097359954));
#13106=CARTESIAN_POINT('Ctrl Pts',(6.52500937810087,1.80196683068908,16.3885076766382));
#13107=CARTESIAN_POINT('Ctrl Pts',(6.47628228269598,1.96991684758406,16.396705617281));
#13108=CARTESIAN_POINT('Ctrl Pts',(6.42115074664811,2.13567602618478,16.4049035579238));
#13109=CARTESIAN_POINT('Ctrl Pts',(6.36600314988914,2.30148349312409,16.4131038867598));
#13110=CARTESIAN_POINT('Ctrl Pts',(6.30444750937547,2.46509851023569,16.4213042155958));
#13111=CARTESIAN_POINT('Ctrl Pts',(6.23669788805495,2.62600237112059,16.4295045444317));
#13112=CARTESIAN_POINT('Ctrl Pts',(6.16887766987088,2.78707389800407,16.4377134182231));
#13113=CARTESIAN_POINT('Ctrl Pts',(6.0948507155596,2.9454282935398,16.4459222920146));
#13114=CARTESIAN_POINT('Ctrl Pts',(6.01487848943923,3.10056861837975,16.454131165806));
#13115=CARTESIAN_POINT('Ctrl Pts',(5.93486334310725,3.25579220532072,16.4623444452094));
#13116=CARTESIAN_POINT('Ctrl Pts',(5.84889674046926,3.40779797089882,16.4705577246128));
#13117=CARTESIAN_POINT('Ctrl Pts',(5.75728462341509,3.55611624739521,16.4787710040162));
#13118=CARTESIAN_POINT('Ctrl Pts',(5.66553850924091,3.70465146268238,16.4869962966317));
#13119=CARTESIAN_POINT('Ctrl Pts',(5.56813057882467,3.84948811265275,16.4952215892471));
#13120=CARTESIAN_POINT('Ctrl Pts',(5.46540911599033,3.99018698745433,16.5034468818626));
#13121=CARTESIAN_POINT('Ctrl Pts',(5.37250989221313,4.11743221834117,16.5108856709747));
#13122=CARTESIAN_POINT('Ctrl Pts',(5.27526536421087,4.24129342813061,16.5183244600868));
#13123=CARTESIAN_POINT('Ctrl Pts',(5.17395949578523,4.36147132696913,16.525763249199));
#13124=CARTESIAN_POINT('Ctrl Pts',(5.06191368188543,4.49438989030008,16.5339906618203));
#13125=CARTESIAN_POINT('Ctrl Pts',(4.94458594637151,4.62317381704289,16.5422180744416));
#13126=CARTESIAN_POINT('Ctrl Pts',(4.82231245014207,4.74737734261822,16.5504454870629));
#13127=CARTESIAN_POINT('Ctrl Pts',(4.69715469852805,4.87451065018614,16.5588669724791));
#13128=CARTESIAN_POINT('Ctrl Pts',(4.56681515025296,4.99684446344319,16.5672884578953));
#13129=CARTESIAN_POINT('Ctrl Pts',(4.43169984610697,5.11393444170098,16.5757099433115));
#13130=CARTESIAN_POINT('Ctrl Pts',(4.29999521699383,5.22806875281235,16.5839188477013));
#13131=CARTESIAN_POINT('Ctrl Pts',(4.16375330290666,5.33722049437015,16.592127752091));
#13132=CARTESIAN_POINT('Ctrl Pts',(4.02338898069103,5.44101370243212,16.6003366564807));
#13133=CARTESIAN_POINT('Ctrl Pts',(3.87757226368288,5.54883871528751,16.6088644324102));
#13134=CARTESIAN_POINT('Ctrl Pts',(3.72730670528221,5.65088024959378,16.6173922083396));
#13135=CARTESIAN_POINT('Ctrl Pts',(3.57309691048976,5.74676147654038,16.6259199842691));
#13136=CARTESIAN_POINT('Ctrl Pts',(3.41888711569731,5.84264270348698,16.6344477601985));
#13137=CARTESIAN_POINT('Ctrl Pts',(3.26073343455383,5.9323633632272,16.6429755361279));
#13138=CARTESIAN_POINT('Ctrl Pts',(3.09917575053259,6.01559628526639,16.6515033120574));
#13139=CARTESIAN_POINT('Origin',(0.,0.,-3.69717978381041));
#13140=CARTESIAN_POINT('',(3.09917575053257,6.0155962852664,19.0456175016683));
#13141=CARTESIAN_POINT('',(3.0991757505326,6.01559628526638,18.6513920151221));
#13142=CARTESIAN_POINT('',(3.09917575053259,6.01559628526639,-3.69717978381041));
#13143=CARTESIAN_POINT('',(-6.76699920193514,-0.00194542300215272,17.69717978381));
#13144=CARTESIAN_POINT('Ctrl Pts',(-6.76699772241609,-0.0055520100402695,
17.69717978381));
#13145=CARTESIAN_POINT('Ctrl Pts',(-6.76682955409667,-0.210521854514989,
17.7067908133179));
#13146=CARTESIAN_POINT('Ctrl Pts',(-6.75734493412658,-0.415082670399996,
17.7164018428258));
#13147=CARTESIAN_POINT('Ctrl Pts',(-6.73867812456815,-0.618470802436715,
17.7260128723337));
#13148=CARTESIAN_POINT('Ctrl Pts',(-6.71988957760058,-0.823185349904371,
17.7356865811028));
#13149=CARTESIAN_POINT('Ctrl Pts',(-6.69179878842976,-1.02671180498338,
17.7453602898719));
#13150=CARTESIAN_POINT('Ctrl Pts',(-6.65459139278692,-1.22829247129757,
17.7550339986409));
#13151=CARTESIAN_POINT('Ctrl Pts',(-6.61709441421887,-1.43144202782853,
17.7647829973042));
#13152=CARTESIAN_POINT('Ctrl Pts',(-6.5703384359958,-1.63261532843543,17.7745319959675));
#13153=CARTESIAN_POINT('Ctrl Pts',(-6.5145615175188,-1.83105904723556,17.7842809946309));
#13154=CARTESIAN_POINT('Ctrl Pts',(-6.49042741594287,-1.91692361267588,
17.7884992865414));
#13155=CARTESIAN_POINT('Ctrl Pts',(-6.46460501037005,-2.00227743012385,
17.7927175784519));
#13156=CARTESIAN_POINT('Ctrl Pts',(-6.43711629998103,-2.08706078984742,
17.7969358703624));
#13157=CARTESIAN_POINT('Ctrl Pts',(-6.38351853804928,-2.2523722310147,17.80516073804));
#13158=CARTESIAN_POINT('Ctrl Pts',(-6.32347339824635,-2.41584976197224,
17.8133856057175));
#13159=CARTESIAN_POINT('Ctrl Pts',(-6.25712366996655,-2.57695408937458,
17.8216104733951));
#13160=CARTESIAN_POINT('Ctrl Pts',(-6.19084869208219,-2.73787691471967,
17.8298260748387));
#13161=CARTESIAN_POINT('Ctrl Pts',(-6.11828340463295,-2.89643153177296,
17.8380416762822));
#13162=CARTESIAN_POINT('Ctrl Pts',(-6.03962048177441,-3.05209328758659,
17.8462572777258));
#13163=CARTESIAN_POINT('Ctrl Pts',(-5.96103037654355,-3.20761094857933,
17.8544652740539));
#13164=CARTESIAN_POINT('Ctrl Pts',(-5.87635403789743,-3.36024076323195,
17.8626732703821));
#13165=CARTESIAN_POINT('Ctrl Pts',(-5.78583241465863,-3.50947749237483,
17.8708812667102));
#13166=CARTESIAN_POINT('Ctrl Pts',(-5.69537640481127,-3.65860604926475,
17.8790833135816));
#13167=CARTESIAN_POINT('Ctrl Pts',(-5.59908373473887,-3.80434611386227,
17.8872853604531));
#13168=CARTESIAN_POINT('Ctrl Pts',(-5.49724155456428,-3.9462164526001,17.8954874073246));
#13169=CARTESIAN_POINT('Ctrl Pts',(-5.39545274251451,-4.0880124473487,17.9036851560961));
#13170=CARTESIAN_POINT('Ctrl Pts',(-5.28812042248059,-4.22594246526505,
17.9118829048677));
#13171=CARTESIAN_POINT('Ctrl Pts',(-5.17557542968355,-4.35955364362637,
17.9200806536393));
#13172=CARTESIAN_POINT('Ctrl Pts',(-5.06305190258383,-4.49313933833851,
17.928276838855));
#13173=CARTESIAN_POINT('Ctrl Pts',(-4.94531790921027,-4.62240755613955,
17.9364730240706));
#13174=CARTESIAN_POINT('Ctrl Pts',(-4.82274518599496,-4.74693773615817,
17.9446692092862));
#13175=CARTESIAN_POINT('Ctrl Pts',(-4.70018153043303,-4.87145870371516,
17.9528647881666));
#13176=CARTESIAN_POINT('Ctrl Pts',(-4.57278010898451,-4.99124207518212,
17.9610603670469));
#13177=CARTESIAN_POINT('Ctrl Pts',(-4.44095016519683,-5.1059035077289,17.9692559459273));
#13178=CARTESIAN_POINT('Ctrl Pts',(-4.30910598899387,-5.22057731917138,
17.9774524096057));
#13179=CARTESIAN_POINT('Ctrl Pts',(-4.17283260872368,-5.33012785447943,
17.9856488732841));
#13180=CARTESIAN_POINT('Ctrl Pts',(-4.03257307824404,-5.43421046414485,
17.9938453369626));
#13181=CARTESIAN_POINT('Ctrl Pts',(-3.8922728866202,-5.5383232472893,18.0020441767904));
#13182=CARTESIAN_POINT('Ctrl Pts',(-3.74798453110036,-5.63696473360017,
18.0102430166181));
#13183=CARTESIAN_POINT('Ctrl Pts',(-3.6001808504722,-5.72983305549937,18.0184418564459));
#13184=CARTESIAN_POINT('Ctrl Pts',(-3.45222278469464,-5.82279838100288,
18.0266492601952));
#13185=CARTESIAN_POINT('Ctrl Pts',(-3.30074236215719,-5.90997830331226,
18.0348566639444));
#13186=CARTESIAN_POINT('Ctrl Pts',(-3.14623875598282,-5.99111598037892,
18.0430640676936));
#13187=CARTESIAN_POINT('Ctrl Pts',(-2.99165238950068,-6.07229711907921,
18.0512758677627));
#13188=CARTESIAN_POINT('Ctrl Pts',(-2.83403993471587,-6.14742940613931,
18.0594876678317));
#13189=CARTESIAN_POINT('Ctrl Pts',(-2.67392133894803,-6.21630385945848,
18.0676994679007));
#13190=CARTESIAN_POINT('Ctrl Pts',(-2.51356702623398,-6.2852797055967,18.0759233568869));
#13191=CARTESIAN_POINT('Ctrl Pts',(-2.35069953427168,-6.34797917833961,
18.084147245873));
#13192=CARTESIAN_POINT('Ctrl Pts',(-2.18585602150401,-6.40424253548027,
18.0923711348592));
#13193=CARTESIAN_POINT('Ctrl Pts',(-2.03354346549322,-6.4562289048069,18.0999698661092));
#13194=CARTESIAN_POINT('Ctrl Pts',(-1.87954426568277,-6.5027209735621,18.1075685973592));
#13195=CARTESIAN_POINT('Ctrl Pts',(-1.7242895488774,-6.54363160268304,18.1151673286092));
#13196=CARTESIAN_POINT('Ctrl Pts',(-1.55624221900217,-6.58791316867184,
18.1233921769312));
#13197=CARTESIAN_POINT('Ctrl Pts',(-1.38625214432185,-6.62577927521689,
18.1316170252533));
#13198=CARTESIAN_POINT('Ctrl Pts',(-1.21485021538482,-6.65705850614064,
18.1398418735753));
#13199=CARTESIAN_POINT('Ctrl Pts',(-1.04364132302305,-6.68830250971514,
18.1480574588945));
#13200=CARTESIAN_POINT('Ctrl Pts',(-0.87102409234731,-6.71297434553958,
18.1562730442137));
#13201=CARTESIAN_POINT('Ctrl Pts',(-0.697544064591326,-6.73095247925236,
18.1644886295329));
#13202=CARTESIAN_POINT('Ctrl Pts',(-0.524224558219132,-6.74891397776545,
18.1726966129562));
#13203=CARTESIAN_POINT('Ctrl Pts',(-0.350044199304795,-6.76019407228817,
18.1809045963794));
#13204=CARTESIAN_POINT('Ctrl Pts',(-0.175558293589939,-6.76472233617551,
18.1891125798026));
#13205=CARTESIAN_POINT('Ctrl Pts',(-0.00119879361789976,-6.76924731957691,
18.1973146169792));
#13206=CARTESIAN_POINT('Ctrl Pts',(0.173465455065159,-6.76703020570275,
18.2055166541557));
#13207=CARTESIAN_POINT('Ctrl Pts',(0.347874366087304,-6.75805241363363,
18.2137186913322));
#13208=CARTESIAN_POINT('Ctrl Pts',(0.522191950001651,-6.74907932267628,
18.2219164336116));
#13209=CARTESIAN_POINT('Ctrl Pts',(0.69625410516685,-6.7333526244639,18.230114175891));
#13210=CARTESIAN_POINT('Ctrl Pts',(0.869500997231249,-6.71090582677286,
18.2383119181704));
#13211=CARTESIAN_POINT('Ctrl Pts',(1.04271494926622,-6.68846329696892,18.2465081017848));
#13212=CARTESIAN_POINT('Ctrl Pts',(1.21511359071987,-6.65930325260606,18.2547042853991));
#13213=CARTESIAN_POINT('Ctrl Pts',(1.38614215096062,-6.6235110732398,18.2629004690135));
#13214=CARTESIAN_POINT('Ctrl Pts',(1.55715812111292,-6.58772152867736,18.2710960492744));
#13215=CARTESIAN_POINT('Ctrl Pts',(1.72680385951244,-6.54530089403478,18.2792916295352));
#13216=CARTESIAN_POINT('Ctrl Pts',(1.8945347890943,-6.49638568227837,18.2874872097961));
#13217=CARTESIAN_POINT('Ctrl Pts',(2.06228388799807,-6.44746517181986,18.2956836778368));
#13218=CARTESIAN_POINT('Ctrl Pts',(2.22811742028913,-6.39204878310216,18.3038801458776));
#13219=CARTESIAN_POINT('Ctrl Pts',(2.39150592463515,-6.33032293113353,18.3120766139183));
#13220=CARTESIAN_POINT('Ctrl Pts',(2.55494185464408,-6.2685791624243,18.3202754610917));
#13221=CARTESIAN_POINT('Ctrl Pts',(2.71593100748238,-6.20052240932084,18.3284743082651));
#13222=CARTESIAN_POINT('Ctrl Pts',(2.8739638120376,-6.12638727204691,18.3366731554384));
#13223=CARTESIAN_POINT('Ctrl Pts',(3.03216177624101,-6.05217465634547,18.3448805712044));
#13224=CARTESIAN_POINT('Ctrl Pts',(3.18739689410575,-5.97187111760412,18.3530879869704));
#13225=CARTESIAN_POINT('Ctrl Pts',(3.33918323730906,-5.88575775135829,18.3612954027363));
#13226=CARTESIAN_POINT('Ctrl Pts',(3.49105093265376,-5.7995982313769,18.3695072173885));
#13227=CARTESIAN_POINT('Ctrl Pts',(3.63946586374253,-5.70762286516864,18.3777190320406));
#13228=CARTESIAN_POINT('Ctrl Pts',(3.78397113575172,-5.61015609798853,18.3859308466928));
#13229=CARTESIAN_POINT('Ctrl Pts',(3.9286892137422,-5.51254579617646,18.3941547544904));
#13230=CARTESIAN_POINT('Ctrl Pts',(4.06948583682063,-5.40942814392912,18.402378662288));
#13231=CARTESIAN_POINT('Ctrl Pts',(4.20593623048949,-5.30116868483318,18.4106025700856));
#13232=CARTESIAN_POINT('Ctrl Pts',(4.33201387423434,-5.2011389439954,18.4182013090091));
#13233=CARTESIAN_POINT('Ctrl Pts',(4.45438117505745,-5.09672000800723,18.4258000479326));
#13234=CARTESIAN_POINT('Ctrl Pts',(4.57273176015609,-4.98822746570962,18.4333987868561));
#13235=CARTESIAN_POINT('Ctrl Pts',(4.69968355033694,-4.87185015794663,18.4415497690304));
#13236=CARTESIAN_POINT('Ctrl Pts',(4.82238911410713,-4.75044043053605,18.4497007512046));
#13237=CARTESIAN_POINT('Ctrl Pts',(4.94041991225922,-4.62434212516252,18.4578517333789));
#13238=CARTESIAN_POINT('Ctrl Pts',(5.05831360669997,-4.49839029465767,18.4659932474319));
#13239=CARTESIAN_POINT('Ctrl Pts',(5.17154309735107,-4.36776099155392,18.474134761485));
#13240=CARTESIAN_POINT('Ctrl Pts',(5.27971338460312,-4.23283776873656,18.482276275538));
#13241=CARTESIAN_POINT('Ctrl Pts',(5.38778078503692,-4.09804287895275,18.4904100457411));
#13242=CARTESIAN_POINT('Ctrl Pts',(5.49079833506234,-3.95896248383105,18.4985438159441));
#13243=CARTESIAN_POINT('Ctrl Pts',(5.58840835794962,-3.81601638162087,18.5066775861472));
#13244=CARTESIAN_POINT('Ctrl Pts',(5.68594606787453,-3.67317617894645,18.5148053305652));
#13245=CARTESIAN_POINT('Ctrl Pts',(5.77808402204886,-3.52647627229731,18.5229330749832));
#13246=CARTESIAN_POINT('Ctrl Pts',(5.86450528316306,-3.37636887554553,18.5310608194012));
#13247=CARTESIAN_POINT('Ctrl Pts',(5.95088068976486,-3.22634112472113,18.5391842512952));
#13248=CARTESIAN_POINT('Ctrl Pts',(6.03154526199955,-3.07290980067348,18.5473076831893));
#13249=CARTESIAN_POINT('Ctrl Pts',(6.10622581672461,-2.91655537838147,18.5554311150833));
#13250=CARTESIAN_POINT('Ctrl Pts',(6.18138011551486,-2.75920910513308,18.5636060788341));
#13251=CARTESIAN_POINT('Ctrl Pts',(6.25047400739617,-2.59890283282634,18.571781042585));
#13252=CARTESIAN_POINT('Ctrl Pts',(6.31327624034627,-2.4361510858482,18.5799560063358));
#13253=CARTESIAN_POINT('Ctrl Pts',(6.37566843567783,-2.27446194979337,18.5880775955088));
#13254=CARTESIAN_POINT('Ctrl Pts',(6.43185077589508,-2.11035953200006,18.5961991846818));
#13255=CARTESIAN_POINT('Ctrl Pts',(6.48164509876486,-1.94436771564883,18.6043207738548));
#13256=CARTESIAN_POINT('Ctrl Pts',(6.53144599550652,-1.77835398497344,18.6124434352442));
#13257=CARTESIAN_POINT('Ctrl Pts',(6.57485708992834,-1.61045070948888,18.6205660966336));
#13258=CARTESIAN_POINT('Ctrl Pts',(6.61175036118388,-1.44119608706966,18.6286887580229));
#13259=CARTESIAN_POINT('Ctrl Pts',(6.648655528678,-1.27188688848241,18.6368140385652));
#13260=CARTESIAN_POINT('Ctrl Pts',(6.67903861002489,-1.10122583266907,18.6449393191074));
#13261=CARTESIAN_POINT('Ctrl Pts',(6.70282288382531,-0.929760392825894,
18.6530645996497));
#13262=CARTESIAN_POINT('Ctrl Pts',(6.72686628235356,-0.756426872594672,
18.6612784034374));
#13263=CARTESIAN_POINT('Ctrl Pts',(6.74416619288582,-0.582271718917682,
18.6694922072252));
#13264=CARTESIAN_POINT('Ctrl Pts',(6.75469733137347,-0.407863900751406,
18.677706011013));
#13265=CARTESIAN_POINT('Ctrl Pts',(6.76513299893489,-0.235037191404557,
18.6858453518681));
#13266=CARTESIAN_POINT('Ctrl Pts',(6.76892217191133,-0.0619627460209338,
18.6939846927233));
#13267=CARTESIAN_POINT('Ctrl Pts',(6.76609271128249,0.110808042713229,18.7021240335784));
#13268=CARTESIAN_POINT('Ctrl Pts',(6.76322442258271,0.285949727290164,18.7103750688325));
#13269=CARTESIAN_POINT('Ctrl Pts',(6.75355455256377,0.460778968813002,18.7186261040866));
#13270=CARTESIAN_POINT('Ctrl Pts',(6.73716613396148,0.634729456857475,18.7268771393406));
#13271=CARTESIAN_POINT('Ctrl Pts',(6.72077771535918,0.808679944901949,18.7351281745947));
#13272=CARTESIAN_POINT('Ctrl Pts',(6.69767086544942,0.981751307841,18.7433792098488));
#13273=CARTESIAN_POINT('Ctrl Pts',(6.66798156185886,1.15339103980841,18.7516302451028));
#13274=CARTESIAN_POINT('Ctrl Pts',(6.63835991892323,1.32463961215692,18.7598624765999));
#13275=CARTESIAN_POINT('Ctrl Pts',(6.60209348720382,1.49499773932892,18.768094708097));
#13276=CARTESIAN_POINT('Ctrl Pts',(6.55924460544374,1.66391081670778,18.7763269395941));
#13277=CARTESIAN_POINT('Ctrl Pts',(6.5164473513962,1.83262037428767,18.7845492522494));
#13278=CARTESIAN_POINT('Ctrl Pts',(6.46708352766374,1.99988800516014,18.7927715649046));
#13279=CARTESIAN_POINT('Ctrl Pts',(6.41126696586366,2.16516625052799,18.8009938775599));
#13280=CARTESIAN_POINT('Ctrl Pts',(6.35550647238797,2.33027847215706,18.8092079308155));
#13281=CARTESIAN_POINT('Ctrl Pts',(6.29330626382452,2.49340495096386,18.8174219840711));
#13282=CARTESIAN_POINT('Ctrl Pts',(6.2248307750094,2.65401032825721,18.8256360373266));
#13283=CARTESIAN_POINT('Ctrl Pts',(6.15641035538368,2.81448654388855,18.8338434846965));
#13284=CARTESIAN_POINT('Ctrl Pts',(6.08172484786925,2.97244536841968,18.8420509320663));
#13285=CARTESIAN_POINT('Ctrl Pts',(6.00098791682371,3.12736838606133,18.8502583794361));
#13286=CARTESIAN_POINT('Ctrl Pts',(5.92030108248002,3.28219527505251,18.8584607341422));
#13287=CARTESIAN_POINT('Ctrl Pts',(5.83357047121772,3.43398979344032,18.8666630888483));
#13288=CARTESIAN_POINT('Ctrl Pts',(5.74105711948312,3.58225517667742,18.8748654435543));
#13289=CARTESIAN_POINT('Ctrl Pts',(5.64857490749069,3.73047065419043,18.8830650373702));
#13290=CARTESIAN_POINT('Ctrl Pts',(5.55031402033129,3.87515905834221,18.891264631186));
#13291=CARTESIAN_POINT('Ctrl Pts',(5.44658064382876,4.01584963491786,18.8994642250018));
#13292=CARTESIAN_POINT('Ctrl Pts',(5.34286336599554,4.1565183773342,18.9076625463));
#13293=CARTESIAN_POINT('Ctrl Pts',(5.23367550300273,4.29319023963244,18.9158608675982));
#13294=CARTESIAN_POINT('Ctrl Pts',(5.11936566405895,4.42542474771114,18.9240591888964));
#13295=CARTESIAN_POINT('Ctrl Pts',(5.0050528293004,4.55766272137161,18.932257725055));
#13296=CARTESIAN_POINT('Ctrl Pts',(4.88561798615235,4.68546283861832,18.9404562612135));
#13297=CARTESIAN_POINT('Ctrl Pts',(4.76144902863808,4.80841888230232,18.9486547973721));
#13298=CARTESIAN_POINT('Ctrl Pts',(4.63720149033507,4.93145273917801,18.9568585220049));
#13299=CARTESIAN_POINT('Ctrl Pts',(4.50821410524588,5.04963614355232,18.9650622466377));
#13300=CARTESIAN_POINT('Ctrl Pts',(4.37491108046193,5.16260031748066,18.9732659712705));
#13301=CARTESIAN_POINT('Ctrl Pts',(4.24156691491425,5.27559935507693,18.981472227785));
#13302=CARTESIAN_POINT('Ctrl Pts',(4.10390473449447,5.38337572724731,18.9896784842996));
#13303=CARTESIAN_POINT('Ctrl Pts',(3.96238058832069,5.48560197911764,18.9978847408141));
#13304=CARTESIAN_POINT('Ctrl Pts',(3.82070029851786,5.58794101723952,19.0061000512937));
#13305=CARTESIAN_POINT('Ctrl Pts',(3.67514982443726,5.68471749589009,19.0143153617733));
#13306=CARTESIAN_POINT('Ctrl Pts',(3.52621376002927,5.77564762763279,19.0225306722529));
#13307=CARTESIAN_POINT('Ctrl Pts',(3.38669939347668,5.86082551776338,19.0302262820581));
#13308=CARTESIAN_POINT('Ctrl Pts',(3.24421469581168,5.94087365416285,19.0379218918632));
#13309=CARTESIAN_POINT('Ctrl Pts',(3.09917575053257,6.0155962852664,19.0456175016683));
#13310=CARTESIAN_POINT('Ctrl Pts',(3.0991757505326,6.01559628526638,17.0457515827422));
#13311=CARTESIAN_POINT('Ctrl Pts',(2.93382384459263,6.1007839529376,17.0545010306546));
#13312=CARTESIAN_POINT('Ctrl Pts',(2.76495772122979,6.17915010267051,17.063250478567));
#13313=CARTESIAN_POINT('Ctrl Pts',(2.59315093316703,6.25042856433181,17.0719999264794));
#13314=CARTESIAN_POINT('Ctrl Pts',(2.42134553245612,6.32170645041453,17.0807493037394));
#13315=CARTESIAN_POINT('Ctrl Pts',(2.24659977927588,6.38589665313458,17.0894986809994));
#13316=CARTESIAN_POINT('Ctrl Pts',(2.0695071868992,6.44278115439075,17.0982480582594));
#13317=CARTESIAN_POINT('Ctrl Pts',(1.89241596572863,6.49966521519724,17.1069973677741));
#13318=CARTESIAN_POINT('Ctrl Pts',(1.71297821457199,6.54924360009546,17.1157466772887));
#13319=CARTESIAN_POINT('Ctrl Pts',(1.53180337335846,6.59134792173556,17.1244959868034));
#13320=CARTESIAN_POINT('Ctrl Pts',(1.35062987477791,6.63345193135303,17.1332452314795));
#13321=CARTESIAN_POINT('Ctrl Pts',(1.16771959102967,6.66808192368235,17.1419944761556));
#13322=CARTESIAN_POINT('Ctrl Pts',(0.98369374690707,6.69512028363165,17.1507437208318));
#13323=CARTESIAN_POINT('Ctrl Pts',(0.799669205420161,6.72215845218863,17.1594929035759));
#13324=CARTESIAN_POINT('Ctrl Pts',(0.614529402873832,6.74160505424576,17.1682420863201));
#13325=CARTESIAN_POINT('Ctrl Pts',(0.428903127363669,6.75339404354119,17.1769912690643));
#13326=CARTESIAN_POINT('Ctrl Pts',(0.243278104164388,6.76518295330328,17.1857403927829));
#13327=CARTESIAN_POINT('Ctrl Pts',(0.0571669005397141,6.76931433552275,
17.1944895165015));
#13328=CARTESIAN_POINT('Ctrl Pts',(-0.128798404776829,6.76577415902474,
17.2032386402201));
#13329=CARTESIAN_POINT('Ctrl Pts',(-0.314762517258441,6.76223400523445,
17.2119877078193));
#13330=CARTESIAN_POINT('Ctrl Pts',(-0.500580446818881,6.75102239665094,
17.2207367754185));
#13331=CARTESIAN_POINT('Ctrl Pts',(-0.68562111884201,6.73217741012504,17.2294858430177));
#13332=CARTESIAN_POINT('Ctrl Pts',(-0.870660665413904,6.71333253821779,
17.2382348574035));
#13333=CARTESIAN_POINT('Ctrl Pts',(-1.0549226788543,6.68685441030621,17.2469838717893));
#13334=CARTESIAN_POINT('Ctrl Pts',(-1.23778137635197,6.65283295028187,17.2557328861751));
#13335=CARTESIAN_POINT('Ctrl Pts',(-1.42999922978796,6.61707018861876,17.2649296965425));
#13336=CARTESIAN_POINT('Ctrl Pts',(-1.62066601233648,6.57297172934425,17.2741265069098));
#13337=CARTESIAN_POINT('Ctrl Pts',(-1.80906628500342,6.52070304311306,17.2833233172772));
#13338=CARTESIAN_POINT('Ctrl Pts',(-1.98831342545484,6.47097374915044,17.292073315015));
#13339=CARTESIAN_POINT('Ctrl Pts',(-2.16550875896659,6.41384933989543,17.3008233127528));
#13340=CARTESIAN_POINT('Ctrl Pts',(-2.34005036713969,6.34952386240492,17.3095733104905));
#13341=CARTESIAN_POINT('Ctrl Pts',(-2.51458843547048,6.28519968948612,17.3183231307714));
#13342=CARTESIAN_POINT('Ctrl Pts',(-2.68647261718017,6.21367483971116,17.3270729510523));
#13343=CARTESIAN_POINT('Ctrl Pts',(-2.85511905908695,6.13519226743861,17.3358227713331));
#13344=CARTESIAN_POINT('Ctrl Pts',(-3.02376230488844,6.05671118252957,17.3445724257917));
#13345=CARTESIAN_POINT('Ctrl Pts',(-3.18916767379861,5.97127275992656,17.3533220802502));
#13346=CARTESIAN_POINT('Ctrl Pts',(-3.35077334102741,5.87916720438023,17.3620717347087));
#13347=CARTESIAN_POINT('Ctrl Pts',(-3.5123761603733,5.78706327195666,17.3708212349772));
#13348=CARTESIAN_POINT('Ctrl Pts',(-3.6701791630227,5.68829258362318,17.3795707352456));
#13349=CARTESIAN_POINT('Ctrl Pts',(-3.8236463656644,5.58319061741057,17.3883202355141));
#13350=CARTESIAN_POINT('Ctrl Pts',(-3.97711106778777,5.47809036367717,17.3970695932225));
#13351=CARTESIAN_POINT('Ctrl Pts',(-4.12623987481906,5.36665920043241,17.4058189509309));
#13352=CARTESIAN_POINT('Ctrl Pts',(-4.27052628213909,5.24927559512351,17.4145683086394));
#13353=CARTESIAN_POINT('Ctrl Pts',(-4.41481053024959,5.13189374643053,17.4233175354159));
#13354=CARTESIAN_POINT('Ctrl Pts',(-4.55425230136512,5.00855981477369,17.4320667621924));
#13355=CARTESIAN_POINT('Ctrl Pts',(-4.68837800630531,4.87969268192093,17.4408159889689));
#13356=CARTESIAN_POINT('Ctrl Pts',(-4.82250188228881,4.75082730631823,17.4495650964398));
#13357=CARTESIAN_POINT('Ctrl Pts',(-4.95130963052956,4.61642907903537,17.4583142039106));
#13358=CARTESIAN_POINT('Ctrl Pts',(-5.0743637903336,4.47695444731697,17.4670633113815));
#13359=CARTESIAN_POINT('Ctrl Pts',(-5.19741643562807,4.33748153220584,17.4758123111712));
#13360=CARTESIAN_POINT('Ctrl Pts',(-5.31471544462783,4.19293255254577,17.484561310961));
#13361=CARTESIAN_POINT('Ctrl Pts',(-5.42586245275645,4.0437984177958,17.4933103107507));
#13362=CARTESIAN_POINT('Ctrl Pts',(-5.53702160019165,3.89464799484326,17.5020602660929));
#13363=CARTESIAN_POINT('Ctrl Pts',(-5.64202723081258,3.74091164443839,17.510810221435));
#13364=CARTESIAN_POINT('Ctrl Pts',(-5.74052265232969,3.58311159163229,17.5195601767772));
#13365=CARTESIAN_POINT('Ctrl Pts',(-5.83901427066926,3.4253176319177,17.5283097942596));
#13366=CARTESIAN_POINT('Ctrl Pts',(-5.93099603115752,3.2634605269559,17.5370594117421));
#13367=CARTESIAN_POINT('Ctrl Pts',(-6.01615550622771,3.09809004467044,17.5458090292245));
#13368=CARTESIAN_POINT('Ctrl Pts',(-6.10131214578817,2.93272506863792,17.5545583553756));
#13369=CARTESIAN_POINT('Ctrl Pts',(-6.17964682328765,2.76384720416855,17.5633076815267));
#13370=CARTESIAN_POINT('Ctrl Pts',(-6.25089348288581,2.59203002791551,17.5720570076778));
#13371=CARTESIAN_POINT('Ctrl Pts',(-6.32213814889336,2.42021765937011,17.5808060890094));
#13372=CARTESIAN_POINT('Ctrl Pts',(-6.38629508412582,2.24546640831924,17.5895551703409));
#13373=CARTESIAN_POINT('Ctrl Pts',(-6.44314639819802,2.06836976660073,17.5983042516725));
#13374=CARTESIAN_POINT('Ctrl Pts',(-6.50000285283694,1.891257111583,17.6070541241069));
#13375=CARTESIAN_POINT('Ctrl Pts',(-6.54955227673245,1.71179891440271,17.6158039965413));
#13376=CARTESIAN_POINT('Ctrl Pts',(-6.59162635926383,1.53060476278439,17.6245538689757));
#13377=CARTESIAN_POINT('Ctrl Pts',(-6.63369752055197,1.34942319164694,17.6333031338982));
#13378=CARTESIAN_POINT('Ctrl Pts',(-6.66829431424256,1.16650618642692,17.6420523988207));
#13379=CARTESIAN_POINT('Ctrl Pts',(-6.69529923745421,0.982474997618328,
17.6508016637432));
#13380=CARTESIAN_POINT('Ctrl Pts',(-6.72230554731447,0.798434359177448,
17.6595513779229));
#13381=CARTESIAN_POINT('Ctrl Pts',(-6.74171916496706,0.613279706239981,
17.6683010921026));
#13382=CARTESIAN_POINT('Ctrl Pts',(-6.75347414817278,0.427639953654957,
17.6770508062823));
#13383=CARTESIAN_POINT('Ctrl Pts',(-6.76248837758745,0.285283364198298,
17.6837604654582));
#13384=CARTESIAN_POINT('Ctrl Pts',(-6.76699999999997,0.142641701104988,
17.6904701246341));
#13385=CARTESIAN_POINT('Ctrl Pts',(-6.767,1.58636168174125E-12,17.69717978381));
#13386=CARTESIAN_POINT('',(-6.767,1.31424060002827E-12,17.3028202161899));
#13387=CARTESIAN_POINT('Ctrl Pts',(3.09917575053259,6.01559628526639,16.6515033120574));
#13388=CARTESIAN_POINT('Ctrl Pts',(2.94387506767171,6.09560566214935,16.6597008139785));
#13389=CARTESIAN_POINT('Ctrl Pts',(2.78542944909053,6.16962022082759,16.6678983158995));
#13390=CARTESIAN_POINT('Ctrl Pts',(2.62434447208533,6.23739569787225,16.6760958178206));
#13391=CARTESIAN_POINT('Ctrl Pts',(2.46326803250356,6.30516758285043,16.6842928852782));
#13392=CARTESIAN_POINT('Ctrl Pts',(2.29955284339014,6.36670090486711,16.6924899527357));
#13393=CARTESIAN_POINT('Ctrl Pts',(2.13372505003637,6.42179931256399,16.7006870201933));
#13394=CARTESIAN_POINT('Ctrl Pts',(1.96787590654538,6.47690481411734,16.7088851430138));
#13395=CARTESIAN_POINT('Ctrl Pts',(1.79991395740129,6.52557363774467,16.7170832658344));
#13396=CARTESIAN_POINT('Ctrl Pts',(1.6303811634924,6.5676591158288,16.7252813886549));
#13397=CARTESIAN_POINT('Ctrl Pts',(1.46079572998701,6.60975766137047,16.7334820569763));
#13398=CARTESIAN_POINT('Ctrl Pts',(1.28963882818744,6.64526870335634,16.7416827252977));
#13399=CARTESIAN_POINT('Ctrl Pts',(1.11746332919481,6.67409654619297,16.7498833936192));
#13400=CARTESIAN_POINT('Ctrl Pts',(0.945107085032572,6.70295465171721,16.7580926707798));
#13401=CARTESIAN_POINT('Ctrl Pts',(0.771730461697409,6.72511548321223,16.7663019479404));
#13402=CARTESIAN_POINT('Ctrl Pts',(0.597893167046674,6.7405350500386,16.7745112251011));
#13403=CARTESIAN_POINT('Ctrl Pts',(0.42395958531355,6.75596315763929,16.7827250493145));
#13404=CARTESIAN_POINT('Ctrl Pts',(0.249565181382425,6.76464253932623,16.7909388735278));
#13405=CARTESIAN_POINT('Ctrl Pts',(0.0752703002990371,6.76658136594048,
16.7991526977412));
#13406=CARTESIAN_POINT('Ctrl Pts',(-0.0992746015544309,6.76852297374325,
16.8073783044386));
#13407=CARTESIAN_POINT('Ctrl Pts',(-0.273719337000601,6.76370471566187,
16.815603911136));
#13408=CARTESIAN_POINT('Ctrl Pts',(-0.447506833163368,6.75218680386378,
16.8238295178335));
#13409=CARTESIAN_POINT('Ctrl Pts',(-0.586504537929725,6.74297461461549,
16.8304084747578));
#13410=CARTESIAN_POINT('Ctrl Pts',(-0.725081847503001,6.72947766089104,
16.8369874316822));
#13411=CARTESIAN_POINT('Ctrl Pts',(-0.862958650407477,6.71175024622393,
16.8435663886066));
#13412=CARTESIAN_POINT('Ctrl Pts',(-1.0338137569393,6.68978266895436,16.8517189448199));
#13413=CARTESIAN_POINT('Ctrl Pts',(-1.20409674113898,6.66125251078687,16.8598715010332));
#13414=CARTESIAN_POINT('Ctrl Pts',(-1.37325904243192,6.62619412652384,16.8680240572464));
#13415=CARTESIAN_POINT('Ctrl Pts',(-1.54222536512024,6.59117635824424,16.8761671685268));
#13416=CARTESIAN_POINT('Ctrl Pts',(-1.71007323507123,6.54964549238403,16.8843102798071));
#13417=CARTESIAN_POINT('Ctrl Pts',(-1.8762586493363,6.50168766404468,16.8924533910874));
#13418=CARTESIAN_POINT('Ctrl Pts',(-2.04228647220672,6.45377531346933,16.9005887803648));
#13419=CARTESIAN_POINT('Ctrl Pts',(-2.20665462915627,6.39944823464897,16.9087241696421));
#13420=CARTESIAN_POINT('Ctrl Pts',(-2.36882876158522,6.33884368779407,16.9168595589195));
#13421=CARTESIAN_POINT('Ctrl Pts',(-2.53088318316271,6.27828387693865,16.9249889429582));
#13422=CARTESIAN_POINT('Ctrl Pts',(-2.69074646403248,6.21145595216779,16.9331183269968));
#13423=CARTESIAN_POINT('Ctrl Pts',(-2.84789888639288,6.13854713534744,16.9412477110355));
#13424=CARTESIAN_POINT('Ctrl Pts',(-3.00496831426195,6.06567682273895,16.9493728018276));
#13425=CARTESIAN_POINT('Ctrl Pts',(-3.1593294039289,5.98673216723843,16.9574978926197));
#13426=CARTESIAN_POINT('Ctrl Pts',(-3.31048193344775,5.90194869245032,16.9656229834118));
#13427=CARTESIAN_POINT('Ctrl Pts',(-3.46221144494007,5.81684158075877,16.9737790894369));
#13428=CARTESIAN_POINT('Ctrl Pts',(-3.61070750648893,5.72585112334431,16.981935195462));
#13429=CARTESIAN_POINT('Ctrl Pts',(-3.7554881793884,5.62926261018919,16.9900913014871));
#13430=CARTESIAN_POINT('Ctrl Pts',(-3.89968613626307,5.53306284833147,16.9982145806605));
#13431=CARTESIAN_POINT('Ctrl Pts',(-4.04019826204967,5.43131023172939,17.0063378598339));
#13432=CARTESIAN_POINT('Ctrl Pts',(-4.17657693742558,5.32433038848688,17.0144611390073));
#13433=CARTESIAN_POINT('Ctrl Pts',(-4.31297377277473,5.21733629997409,17.0225854998639));
#13434=CARTESIAN_POINT('Ctrl Pts',(-4.44523577354727,5.10511382422921,17.0307098607206));
#13435=CARTESIAN_POINT('Ctrl Pts',(-4.57294805431455,4.98802917919901,17.0388342215773));
#13436=CARTESIAN_POINT('Ctrl Pts',(-4.70070163897,4.87090666740255,17.0469612099627));
#13437=CARTESIAN_POINT('Ctrl Pts',(-4.82390230400096,4.74891910207833,17.0550881983481));
#13438=CARTESIAN_POINT('Ctrl Pts',(-4.94217174629426,4.62246984091089,17.0632151867336));
#13439=CARTESIAN_POINT('Ctrl Pts',(-5.06120578706661,4.49520309966668,17.0713947151736));
#13440=CARTESIAN_POINT('Ctrl Pts',(-5.1752443677409,4.36341704834046,17.0795742436137));
#13441=CARTESIAN_POINT('Ctrl Pts',(-5.28394330108761,4.22755629068277,17.0877537720537));
#13442=CARTESIAN_POINT('Ctrl Pts',(-5.39213033611443,4.09233534513216,17.0958947804574));
#13443=CARTESIAN_POINT('Ctrl Pts',(-5.49502774242374,3.95307832093067,17.1040357888611));
#13444=CARTESIAN_POINT('Ctrl Pts',(-5.5923402341602,3.81025192151295,17.1121767972648));
#13445=CARTESIAN_POINT('Ctrl Pts',(-5.69034339231075,3.66641182492886,17.1203755857231));
#13446=CARTESIAN_POINT('Ctrl Pts',(-5.7826818672945,3.51895182023507,17.1285743741813));
#13447=CARTESIAN_POINT('Ctrl Pts',(-5.86910172030054,3.3683726036122,17.1367731626396));
#13448=CARTESIAN_POINT('Ctrl Pts',(-5.95552157330658,3.21779338698933,17.1449719510978));
#13449=CARTESIAN_POINT('Ctrl Pts',(-6.03602268941887,3.06409531746996,17.153170739556));
#13450=CARTESIAN_POINT('Ctrl Pts',(-6.11040100682139,2.90779788428223,17.1613695280143));
#13451=CARTESIAN_POINT('Ctrl Pts',(-6.19254802448167,2.73517542584659,17.170424667251));
#13452=CARTESIAN_POINT('Ctrl Pts',(-6.26744643549823,2.55892230665628,17.1794798064877));
#13453=CARTESIAN_POINT('Ctrl Pts',(-6.33479437433313,2.37963636611087,17.1885349457244));
#13454=CARTESIAN_POINT('Ctrl Pts',(-6.40198623639121,2.20076591521835,17.1975690999545));
#13455=CARTESIAN_POINT('Ctrl Pts',(-6.46166245057633,2.01887688447162,17.2066032541845));
#13456=CARTESIAN_POINT('Ctrl Pts',(-6.51356849724899,1.83458835482121,17.2156374084146));
#13457=CARTESIAN_POINT('Ctrl Pts',(-6.56528345218299,1.65097828207134,17.2246383034706));
#13458=CARTESIAN_POINT('Ctrl Pts',(-6.60928523640393,1.46498655862471,17.2336391985266));
#13459=CARTESIAN_POINT('Ctrl Pts',(-6.64536888477817,1.27724758180319,17.2426400935826));
#13460=CARTESIAN_POINT('Ctrl Pts',(-6.68136586184701,1.08995954558578,17.2516193688923));
#13461=CARTESIAN_POINT('Ctrl Pts',(-6.70948258695721,0.900932855765144,
17.260598644202));
#13462=CARTESIAN_POINT('Ctrl Pts',(-6.72956382804599,0.710816209898906,
17.2695779195117));
#13463=CARTESIAN_POINT('Ctrl Pts',(-6.74957342088702,0.52137788488361,17.2785251574917));
#13464=CARTESIAN_POINT('Ctrl Pts',(-6.76160468038598,0.330857593982595,
17.2874723954717));
#13465=CARTESIAN_POINT('Ctrl Pts',(-6.7655534494534,0.139912553365295,17.2964196334517));
#13466=CARTESIAN_POINT('Ctrl Pts',(-6.76649505933669,0.0943804560610796,
17.2985531610311));
#13467=CARTESIAN_POINT('Ctrl Pts',(-6.76697731126835,0.0488242673506343,
17.3006866886105));
#13468=CARTESIAN_POINT('Ctrl Pts',(-6.76699921811354,0.00325300641797097,
17.3028202161899));
#13469=CARTESIAN_POINT('Ctrl Pts',(-6.767,1.3142405932883E-12,17.3028202161899));
#13470=CARTESIAN_POINT('Ctrl Pts',(-6.76700000000004,-0.186007249414463,
17.3115697279959));
#13471=CARTESIAN_POINT('Ctrl Pts',(-6.75932637295445,-0.372014355526415,
17.3203192398018));
#13472=CARTESIAN_POINT('Ctrl Pts',(-6.74400518266936,-0.55738953715403,
17.3290687516078));
#13473=CARTESIAN_POINT('Ctrl Pts',(-6.72868405709656,-0.742763935810426,
17.3378182264583));
#13474=CARTESIAN_POINT('Ctrl Pts',(-6.70571545653004,-0.927506129694114,
17.3465677013089));
#13475=CARTESIAN_POINT('Ctrl Pts',(-6.67517739415665,-1.11098863924889,
17.3553171761594));
#13476=CARTESIAN_POINT('Ctrl Pts',(-6.64463945823082,-1.29447038906596,
17.3640666147814));
#13477=CARTESIAN_POINT('Ctrl Pts',(-6.60653217027133,-1.47669218228329,
17.3728160534034));
#13478=CARTESIAN_POINT('Ctrl Pts',(-6.56098496116679,-1.6570351050425,17.3815654920254));
#13479=CARTESIAN_POINT('Ctrl Pts',(-6.51543793687478,-1.8373772960416,17.3903148951456));
#13480=CARTESIAN_POINT('Ctrl Pts',(-6.46245112202593,-2.01584035397204,
17.3990642982658));
#13481=CARTESIAN_POINT('Ctrl Pts',(-6.40220448416188,-2.19181813638304,
17.4078137013861));
#13482=CARTESIAN_POINT('Ctrl Pts',(-6.34195808575124,-2.36779521936114,
17.4165630697314));
#13483=CARTESIAN_POINT('Ctrl Pts',(-6.27445201489162,-2.54128677545007,
17.4253124380766));
#13484=CARTESIAN_POINT('Ctrl Pts',(-6.19991555136101,-2.71170355238029,
17.4340618064219));
#13485=CARTESIAN_POINT('Ctrl Pts',(-6.12537937788951,-2.88211966613258,
17.442811140719));
#13486=CARTESIAN_POINT('Ctrl Pts',(-6.04381298133524,-3.04946076210629,
17.451560475016));
#13487=CARTESIAN_POINT('Ctrl Pts',(-5.95549339426208,-3.21315848207036,
17.4603098093131));
#13488=CARTESIAN_POINT('Ctrl Pts',(-5.86717414355064,-3.37685557859803,
17.4690591102886));
#13489=CARTESIAN_POINT('Ctrl Pts',(-5.77210188986144,-3.53690907467464,
17.4778084112642));
#13490=CARTESIAN_POINT('Ctrl Pts',(-5.67059953466978,-3.69277536785043,
17.4865577122398));
#13491=CARTESIAN_POINT('Ctrl Pts',(-5.56909755761672,-3.84864108035928,
17.4953069806205));
#13492=CARTESIAN_POINT('Ctrl Pts',(-5.46116568337973,-4.00031938104412,
17.5040562490013));
#13493=CARTESIAN_POINT('Ctrl Pts',(-5.34717048686014,-4.14729511663348,
17.512805517382));
#13494=CARTESIAN_POINT('Ctrl Pts',(-5.23317570555423,-4.29427031688155,
17.5215547538947));
#13495=CARTESIAN_POINT('Ctrl Pts',(-5.11311782178717,-4.43654275987231,
17.5303039904073));
#13496=CARTESIAN_POINT('Ctrl Pts',(-4.98740459171933,-4.57362924147738,
17.5390532269199));
#13497=CARTESIAN_POINT('Ctrl Pts',(-4.86169180910726,-4.71071523514545,
17.547802432291));
#13498=CARTESIAN_POINT('Ctrl Pts',(-4.73032391415303,-4.8426150931665,17.5565516376621));
#13499=CARTESIAN_POINT('Ctrl Pts',(-4.59374707237139,-4.96888084331666,
17.5653008430333));
#13500=CARTESIAN_POINT('Ctrl Pts',(-4.45717070537242,-5.09514615452864,
17.5740500179895));
#13501=CARTESIAN_POINT('Ctrl Pts',(-4.31538563819344,-5.21577720253769,
17.5827991929457));
#13502=CARTESIAN_POINT('Ctrl Pts',(-4.16887341290477,-5.33036429028783,
17.591548367902));
#13503=CARTESIAN_POINT('Ctrl Pts',(-4.0223616847716,-5.44495098921308,17.6002975131699));
#13504=CARTESIAN_POINT('Ctrl Pts',(-3.87112305634253,-5.55349359238889,
17.6090466584378));
#13505=CARTESIAN_POINT('Ctrl Pts',(-3.71567117316539,-5.655623461026,17.6177958037057));
#13506=CARTESIAN_POINT('Ctrl Pts',(-3.56021980457122,-5.75775299158879,
17.6265449200119));
#13507=CARTESIAN_POINT('Ctrl Pts',(-3.40055544862225,-5.85346967275447,
17.635294036318));
#13508=CARTESIAN_POINT('Ctrl Pts',(-3.23722036323257,-5.94244842803641,
17.6440431526242));
#13509=CARTESIAN_POINT('Ctrl Pts',(-3.07388580495924,-6.03142689616537,
17.6527922406951));
#13510=CARTESIAN_POINT('Ctrl Pts',(-2.90688079257609,-6.11366734484868,
17.661541328766));
#13511=CARTESIAN_POINT('Ctrl Pts',(-2.73677251094543,-6.18889046787334,
17.670290416837));
#13512=CARTESIAN_POINT('Ctrl Pts',(-2.56666476416605,-6.26411335438286,
17.6790394773992));
#13513=CARTESIAN_POINT('Ctrl Pts',(-2.39345402972086,-6.33231884350292,
17.6877885379614));
#13514=CARTESIAN_POINT('Ctrl Pts',(-2.21772856474065,-6.39327529621034,
17.6965375985236));
#13515=CARTESIAN_POINT('Ctrl Pts',(-2.04200363768265,-6.45423156232084,
17.7052866323036));
#13516=CARTESIAN_POINT('Ctrl Pts',(-1.86376426620056,-6.50793874252067,
17.7140356660836));
#13517=CARTESIAN_POINT('Ctrl Pts',(-1.68361578194618,-6.55421443796141,
17.7227846998637));
#13518=CARTESIAN_POINT('Ctrl Pts',(-1.50346783419837,-6.60048999558686,
17.7315337075879));
#13519=CARTESIAN_POINT('Ctrl Pts',(-1.32141106257255,-6.63933404145493,
17.7402827153121));
#13520=CARTESIAN_POINT('Ctrl Pts',(-1.13806375959093,-6.67061465527022,
17.7490317230363));
#13521=CARTESIAN_POINT('Ctrl Pts',(-0.954716987419442,-6.70189517852477,
17.7577807054312));
#13522=CARTESIAN_POINT('Ctrl Pts',(-0.770079973809966,-6.72561226535827,
17.7665296878261));
#13523=CARTESIAN_POINT('Ctrl Pts',(-0.584779770552345,-6.74168536939783,
17.775278670221));
#13524=CARTESIAN_POINT('Ctrl Pts',(-0.391490647553809,-6.75845143942394,
17.784404850897));
#13525=CARTESIAN_POINT('Ctrl Pts',(-0.19748021310424,-6.76689975924027,
17.7935310315731));
#13526=CARTESIAN_POINT('Ctrl Pts',(-0.0034653262977096,-6.76699911271707,
17.8026572122491));
#13527=CARTESIAN_POINT('Ctrl Pts',(0.184486595296115,-6.76709536139773,
17.8114981997791));
#13528=CARTESIAN_POINT('Ctrl Pts',(0.372442378185263,-6.7593565972677,17.820339187309));
#13529=CARTESIAN_POINT('Ctrl Pts',(0.559750217722093,-6.74380965729016,
17.8291801748389));
#13530=CARTESIAN_POINT('Ctrl Pts',(0.745129914457804,-6.72842275717253,
17.8379301534367));
#13531=CARTESIAN_POINT('Ctrl Pts',(0.929874656314276,-6.70538772273472,
17.8466801320345));
#13532=CARTESIAN_POINT('Ctrl Pts',(1.11335688289791,-6.6747828018074,17.8554301106322));
#13533=CARTESIAN_POINT('Ctrl Pts',(1.29683723118871,-6.64417819418021,17.8641799996572));
#13534=CARTESIAN_POINT('Ctrl Pts',(1.47905480730249,-6.60600390230072,17.8729298886821));
#13535=CARTESIAN_POINT('Ctrl Pts',(1.65939064804823,-6.56038959797131,17.881679777707));
#13536=CARTESIAN_POINT('Ctrl Pts',(1.83972470264283,-6.51477574543251,17.890429580068));
#13537=CARTESIAN_POINT('Ctrl Pts',(2.01817678125869,-6.46172209820093,17.8991793824289));
#13538=CARTESIAN_POINT('Ctrl Pts',(2.19414072347704,-6.40140886724006,17.9079291847899));
#13539=CARTESIAN_POINT('Ctrl Pts',(2.37010298132117,-6.34109621361367,17.9166789033954));
#13540=CARTESIAN_POINT('Ctrl Pts',(2.54357687926929,-6.27352420825964,17.9254286220009));
#13541=CARTESIAN_POINT('Ctrl Pts',(2.71397317789983,-6.19892237325491,17.9341783406064));
#13542=CARTESIAN_POINT('Ctrl Pts',(2.8843679020721,-6.12432122756959,17.9429279783646));
#13543=CARTESIAN_POINT('Ctrl Pts',(3.05168482126262,-6.04269049717414,17.9516776161229));
#13544=CARTESIAN_POINT('Ctrl Pts',(3.21535561997391,-5.95430745234928,17.9604272538812));
#13545=CARTESIAN_POINT('Ctrl Pts',(3.37902496075278,-5.86592519481518,17.9691768137002));
#13546=CARTESIAN_POINT('Ctrl Pts',(3.53904799384867,-5.77079087940237,17.9779263735192));
#13547=CARTESIAN_POINT('Ctrl Pts',(3.69488118814971,-5.66922763747033,17.9866759333382));
#13548=CARTESIAN_POINT('Ctrl Pts',(3.85071304610825,-5.56766526649057,17.9954254181256));
#13549=CARTESIAN_POINT('Ctrl Pts',(4.00235489705966,-5.45967423580715,18.0041749029131));
#13550=CARTESIAN_POINT('Ctrl Pts',(4.14929168607657,-5.34562133936326,18.0129243877005));
#13551=CARTESIAN_POINT('Ctrl Pts',(4.29622726385759,-5.23156938308529,18.0216738003638));
#13552=CARTESIAN_POINT('Ctrl Pts',(4.43845763092068,-5.11145583677202,18.0304232130271));
#13553=CARTESIAN_POINT('Ctrl Pts',(4.57549970660961,-4.98568866204212,18.0391726256904));
#13554=CARTESIAN_POINT('Ctrl Pts',(4.71254069815295,-4.85992248226161,18.0479219691367));
#13555=CARTESIAN_POINT('Ctrl Pts',(4.84439326931316,-4.72850295734001,18.0566713125831));
#13556=CARTESIAN_POINT('Ctrl Pts',(4.97060959434701,-4.59187644221679,18.0654206560294));
#13557=CARTESIAN_POINT('Ctrl Pts',(5.09682496280519,-4.4552509625666,18.0741699331657));
#13558=CARTESIAN_POINT('Ctrl Pts',(5.21740397615844,-4.3134187821832,18.082919210302));
#13559=CARTESIAN_POINT('Ctrl Pts',(5.3319371045194,-4.1668616143867,18.0916684874383));
#13560=CARTESIAN_POINT('Ctrl Pts',(5.44646940289394,-4.020305508645,18.1004177011712));
#13561=CARTESIAN_POINT('Ctrl Pts',(5.5549557274968,-3.86902470980112,18.1091669149042));
#13562=CARTESIAN_POINT('Ctrl Pts',(5.65702762491475,-3.71353301465753,18.1179161286372));
#13563=CARTESIAN_POINT('Ctrl Pts',(5.75909881655179,-3.55804239466852,18.1266652818733));
#13564=CARTESIAN_POINT('Ctrl Pts',(5.85475551250813,-3.398341176195,18.1354144351094));
#13565=CARTESIAN_POINT('Ctrl Pts',(5.94367283728131,-3.23497174691903,18.1441635883455));
#13566=CARTESIAN_POINT('Ctrl Pts',(6.03258957676337,-3.07160339300914,18.1529126839911));
#13567=CARTESIAN_POINT('Ctrl Pts',(6.11476689685301,-2.90456712829467,18.1616617796366));
#13568=CARTESIAN_POINT('Ctrl Pts',(6.18992570525271,-2.73443024475883,18.1704108752821));
#13569=CARTESIAN_POINT('Ctrl Pts',(6.26508404388721,-2.56429442462974,18.1791599162432));
#13570=CARTESIAN_POINT('Ctrl Pts',(6.3332238428335,-2.39105828655902,18.1879089572042));
#13571=CARTESIAN_POINT('Ctrl Pts',(6.39411368720077,-2.21531017131955,18.1966579981652));
#13572=CARTESIAN_POINT('Ctrl Pts',(6.45500317120938,-2.03956309619365,18.2054069873477));
#13573=CARTESIAN_POINT('Ctrl Pts',(6.50864269270123,-1.8613043443846,18.2141559765301));
#13574=CARTESIAN_POINT('Ctrl Pts',(6.55485008446384,-1.68113930719747,18.2229049657125));
#13575=CARTESIAN_POINT('Ctrl Pts',(6.60199664749448,-1.49731239211644,18.2318317792419));
#13576=CARTESIAN_POINT('Ctrl Pts',(6.64140563640945,-1.31150116499477,18.2407585927712));
#13577=CARTESIAN_POINT('Ctrl Pts',(6.67293772282205,-1.12436255155468,18.2496854063006));
#13578=CARTESIAN_POINT('Ctrl Pts',(6.70384494949898,-0.940932395049429,
18.2584353204561));
#13579=CARTESIAN_POINT('Ctrl Pts',(6.72718449348952,-0.756227260504809,
18.2671852346116));
#13580=CARTESIAN_POINT('Ctrl Pts',(6.74287707373948,-0.570874564539798,
18.2759351487672));
#13581=CARTESIAN_POINT('Ctrl Pts',(6.75856934538681,-0.385525513630582,
18.2846848908511));
#13582=CARTESIAN_POINT('Ctrl Pts',(6.76661493004109,-0.199529212416338,
18.2934346329351));
#13583=CARTESIAN_POINT('Ctrl Pts',(6.76698649908907,-0.0135174385985409,
18.3021843750191));
#13584=CARTESIAN_POINT('Ctrl Pts',(6.76735806132385,0.172490924447659,18.310933956665));
#13585=CARTESIAN_POINT('Ctrl Pts',(6.76005588896279,0.358514472903279,18.3196835383109));
#13586=CARTESIAN_POINT('Ctrl Pts',(6.74510478454569,0.543921359664073,18.3284331199568));
#13587=CARTESIAN_POINT('Ctrl Pts',(6.73015393440668,0.729325093152307,18.3371825527958));
#13588=CARTESIAN_POINT('Ctrl Pts',(6.70755443556872,0.914111900258213,18.3459319856349));
#13589=CARTESIAN_POINT('Ctrl Pts',(6.67738304682288,1.09765415591724,18.3546814184739));
#13590=CARTESIAN_POINT('Ctrl Pts',(6.64721213111824,1.28119353391464,18.3634307141353));
#13591=CARTESIAN_POINT('Ctrl Pts',(6.60946960955451,1.46348811672849,18.3721800097966));
#13592=CARTESIAN_POINT('Ctrl Pts',(6.56428366991133,1.64391876348422,18.3809293054579));
#13593=CARTESIAN_POINT('Ctrl Pts',(6.51909837867661,1.82434682109919,18.3896784755687));
#13594=CARTESIAN_POINT('Ctrl Pts',(6.46646995271857,2.00291071820652,18.3984276456796));
#13595=CARTESIAN_POINT('Ctrl Pts',(6.40657713281478,2.17900400212913,18.4071768157904));
#13596=CARTESIAN_POINT('Ctrl Pts',(6.34668509278982,2.35509499309869,18.4159258719762));
#13597=CARTESIAN_POINT('Ctrl Pts',(6.27952894037441,2.52871516398334,18.4246749281619));
#13598=CARTESIAN_POINT('Ctrl Pts',(6.20533675061354,2.69927486771632,18.4334239843477));
#13599=CARTESIAN_POINT('Ctrl Pts',(6.12832117907823,2.87632521636121,18.44250598563));
#13600=CARTESIAN_POINT('Ctrl Pts',(6.04372366625987,3.0500772892018,18.4515879869122));
#13601=CARTESIAN_POINT('Ctrl Pts',(5.95185378007777,3.21989527478364,18.4606699881945));
#13602=CARTESIAN_POINT('Ctrl Pts',(5.86334450817275,3.38350129286918,18.4694197685016));
#13603=CARTESIAN_POINT('Ctrl Pts',(5.76808562057155,3.54345567125125,18.4781695488088));
#13604=CARTESIAN_POINT('Ctrl Pts',(5.6664006880438,3.69921508465469,18.4869193291159));
#13605=CARTESIAN_POINT('Ctrl Pts',(5.56471941107814,3.85496889852441,18.4956687948694));
#13606=CARTESIAN_POINT('Ctrl Pts',(5.45661270815,4.00652780919792,18.5044182606228));
#13607=CARTESIAN_POINT('Ctrl Pts',(5.34244776448995,4.15337704569382,18.5131677263763));
#13608=CARTESIAN_POINT('Ctrl Pts',(5.2282863181947,4.30022178356402,18.5219169240959));
#13609=CARTESIAN_POINT('Ctrl Pts',(5.10806717843938,4.4423569097283,18.5306661218155));
#13610=CARTESIAN_POINT('Ctrl Pts',(4.98219864544582,4.57929969070794,18.5394153195351));
#13611=CARTESIAN_POINT('Ctrl Pts',(4.8563332994389,4.71623900430139,18.5481642957254));
#13612=CARTESIAN_POINT('Ctrl Pts',(4.72481904033517,4.84798602483744,18.5569132719156));
#13613=CARTESIAN_POINT('Ctrl Pts',(4.58810250737072,4.97409332259242,18.5656622481058));
#13614=CARTESIAN_POINT('Ctrl Pts',(4.45137708685508,5.10020881822252,18.574411793042));
#13615=CARTESIAN_POINT('Ctrl Pts',(4.3094489263591,5.2206836630805,18.5831613379782));
#13616=CARTESIAN_POINT('Ctrl Pts',(4.16280009466513,5.33510865604966,18.5919108829144));
#13617=CARTESIAN_POINT('Ctrl Pts',(4.01615988348645,5.44952692272997,18.6006599135226));
#13618=CARTESIAN_POINT('Ctrl Pts',(3.86479978232093,5.55789587288722,18.6094089441309));
#13619=CARTESIAN_POINT('Ctrl Pts',(3.70923383580937,5.65984746713964,18.6181579747392));
#13620=CARTESIAN_POINT('Ctrl Pts',(3.55366577799398,5.76180044505471,18.6269071240872));
#13621=CARTESIAN_POINT('Ctrl Pts',(3.39389200026687,5.85733573571148,18.6356562734352));
#13622=CARTESIAN_POINT('Ctrl Pts',(3.23045513625876,5.94612887622018,18.6444054227833));
#13623=CARTESIAN_POINT('Ctrl Pts',(3.18695122151468,5.96976399206746,18.6467342868962));
#13624=CARTESIAN_POINT('Ctrl Pts',(3.1431879126261,5.99292165435361,18.6490631510091));
#13625=CARTESIAN_POINT('Ctrl Pts',(3.0991757505326,6.01559628526638,18.6513920151221));
#13626=CARTESIAN_POINT('Origin',(0.,0.,-3.69717978381041));
#13627=CARTESIAN_POINT('',(3.09917575053256,6.01559628526641,21.0459192328109));
#13628=CARTESIAN_POINT('',(3.09917575053258,6.01559628526639,20.6513153324719));
#13629=CARTESIAN_POINT('',(3.09917575053259,6.01559628526639,-3.69717978381041));
#13630=CARTESIAN_POINT('',(-6.76699999885939,0.000124246054141125,19.6971797837639));
#13631=CARTESIAN_POINT('Ctrl Pts',(-6.7669999988594,0.000124245080715397,
19.69717978381));
#13632=CARTESIAN_POINT('Ctrl Pts',(-6.76700118044791,-0.0642308935099812,
19.7002280624878));
#13633=CARTESIAN_POINT('Ctrl Pts',(-6.76608434959876,-0.128580038527749,
19.7032763411655));
#13634=CARTESIAN_POINT('Ctrl Pts',(-6.76424985513672,-0.192906446970697,
19.7063246198433));
#13635=CARTESIAN_POINT('Ctrl Pts',(-6.75934273488779,-0.364974244362719,
19.71447851201));
#13636=CARTESIAN_POINT('Ctrl Pts',(-6.74785774407388,-0.537136539239102,
19.7226324041768));
#13637=CARTESIAN_POINT('Ctrl Pts',(-6.72977177811207,-0.708844704096933,
19.7307862963435));
#13638=CARTESIAN_POINT('Ctrl Pts',(-6.71170788208171,-0.880343337020776,
19.7389302384837));
#13639=CARTESIAN_POINT('Ctrl Pts',(-6.68705908253956,-1.05138858338574,
19.7470741806239));
#13640=CARTESIAN_POINT('Ctrl Pts',(-6.65585423478447,-1.22143088437358,
19.7552181227641));
#13641=CARTESIAN_POINT('Ctrl Pts',(-6.62468089766368,-1.39130147676015,
19.763353841157));
#13642=CARTESIAN_POINT('Ctrl Pts',(-6.58696475753452,-1.56017078306157,
19.7714895595499));
#13643=CARTESIAN_POINT('Ctrl Pts',(-6.54278651691789,-1.72749344254543,
19.7796252779428));
#13644=CARTESIAN_POINT('Ctrl Pts',(-6.49864359455563,-1.894682336081,19.787754492243));
#13645=CARTESIAN_POINT('Ctrl Pts',(-6.44804895089964,-2.06032669284818,
19.7958837065432));
#13646=CARTESIAN_POINT('Ctrl Pts',(-6.39113450760167,-2.22389044373665,
19.8040129208434));
#13647=CARTESIAN_POINT('Ctrl Pts',(-6.33425359753551,-2.387357825042,19.8121373455189));
#13648=CARTESIAN_POINT('Ctrl Pts',(-6.27106042297508,-2.54874669725629,
19.8202617701943));
#13649=CARTESIAN_POINT('Ctrl Pts',(-6.20173698750099,-2.70753528838725,
19.8283861948698));
#13650=CARTESIAN_POINT('Ctrl Pts',(-6.13199271439522,-2.86728782791703,
19.8365599400039));
#13651=CARTESIAN_POINT('Ctrl Pts',(-6.05604360342782,-3.02440804940822,
19.8447336851381));
#13652=CARTESIAN_POINT('Ctrl Pts',(-5.97412475089426,-3.17838362391211,
19.8529074302723));
#13653=CARTESIAN_POINT('Ctrl Pts',(-5.89273048272117,-3.3313731838933,19.8610288331345));
#13654=CARTESIAN_POINT('Ctrl Pts',(-5.80544290068403,-3.48125793792535,
19.8691502359966));
#13655=CARTESIAN_POINT('Ctrl Pts',(-5.71253922890306,-3.62755903580405,
19.8772716388588));
#13656=CARTESIAN_POINT('Ctrl Pts',(-5.61962837429932,-3.77387144491337,
19.885393669625));
#13657=CARTESIAN_POINT('Ctrl Pts',(-5.52110076120839,-3.91659933698607,
19.8935157003913));
#13658=CARTESIAN_POINT('Ctrl Pts',(-5.41727741718297,-4.05529214549081,
19.9016377311575));
#13659=CARTESIAN_POINT('Ctrl Pts',(-5.31342627572112,-4.19402208730659,
19.9097619364987));
#13660=CARTESIAN_POINT('Ctrl Pts',(-5.20427679933225,-4.32871450152973,
19.9178861418398));
#13661=CARTESIAN_POINT('Ctrl Pts',(-5.0901907940493,-4.45895129825117,19.9260103471809));
#13662=CARTESIAN_POINT('Ctrl Pts',(-4.9748698867004,-4.59059781818042,19.9342224914233));
#13663=CARTESIAN_POINT('Ctrl Pts',(-4.85450520926144,-4.71769140998133,
19.9424346356658));
#13664=CARTESIAN_POINT('Ctrl Pts',(-4.72950863058107,-4.83983854206514,
19.9506467799082));
#13665=CARTESIAN_POINT('Ctrl Pts',(-4.60565313290003,-4.96087060545654,
19.9587839563246));
#13666=CARTESIAN_POINT('Ctrl Pts',(-4.47725026378617,-5.07704594622458,
19.9669211327411));
#13667=CARTESIAN_POINT('Ctrl Pts',(-4.34473366381677,-5.18802258962867,
19.9750583091576));
#13668=CARTESIAN_POINT('Ctrl Pts',(-4.21038575021389,-5.30053287515843,
19.983307937313));
#13669=CARTESIAN_POINT('Ctrl Pts',(-4.07180988413855,-5.40769948419134,
19.9915575654684));
#13670=CARTESIAN_POINT('Ctrl Pts',(-3.92948752405395,-5.50921199431501,
19.9998071936238));
#13671=CARTESIAN_POINT('Ctrl Pts',(-3.78716516396939,-5.61072450443865,
20.0080568217793));
#13672=CARTESIAN_POINT('Ctrl Pts',(-3.64109666627524,-5.70658275743039,
20.0163064499347));
#13673=CARTESIAN_POINT('Ctrl Pts',(-3.49178809428973,-5.79652524402133,
20.0245560780901));
#13674=CARTESIAN_POINT('Ctrl Pts',(-3.34292765784637,-5.88619777675459,
20.0327809457677));
#13675=CARTESIAN_POINT('Ctrl Pts',(-3.19040169834388,-5.97025819324048,
20.0410058134453));
#13676=CARTESIAN_POINT('Ctrl Pts',(-3.03467163341242,-6.04839293344621,
20.0492306811229));
#13677=CARTESIAN_POINT('Ctrl Pts',(-2.87911701583027,-6.12643964612132,
20.0574462825664));
#13678=CARTESIAN_POINT('Ctrl Pts',(-2.72036579856576,-6.19857381658468,
20.06566188401));
#13679=CARTESIAN_POINT('Ctrl Pts',(-2.55890746445812,-6.26452564751239,
20.0738774854535));
#13680=CARTESIAN_POINT('Ctrl Pts',(-2.39759859101656,-6.33041642736686,
20.0820854817816));
#13681=CARTESIAN_POINT('Ctrl Pts',(-2.23358792143174,-6.39013613022706,
20.0902934781098));
#13682=CARTESIAN_POINT('Ctrl Pts',(-2.06738865823994,-6.44346126982858,
20.0985014744379));
#13683=CARTESIAN_POINT('Ctrl Pts',(-1.90130986236754,-6.49674775741382,
20.1067035213094));
#13684=CARTESIAN_POINT('Ctrl Pts',(-1.7330459728758,-6.54364880464831,20.1149055681808));
#13685=CARTESIAN_POINT('Ctrl Pts',(-1.56312933574331,-6.58398934383545,
20.1231076150523));
#13686=CARTESIAN_POINT('Ctrl Pts',(-1.39330173963801,-6.62430874346198,
20.1313053638238));
#13687=CARTESIAN_POINT('Ctrl Pts',(-1.22182346951432,-6.65807440118618,
20.1395031125954));
#13688=CARTESIAN_POINT('Ctrl Pts',(-1.04924125274902,-6.6851613139497,20.147700861367));
#13689=CARTESIAN_POINT('Ctrl Pts',(-0.876691952575874,-6.71224306042856,
20.1558970465826));
#13690=CARTESIAN_POINT('Ctrl Pts',(-0.703039478270456,-6.73264853755229,
20.1640932317982));
#13691=CARTESIAN_POINT('Ctrl Pts',(-0.528840259173994,-6.74630394959172,
20.1722894170138));
#13692=CARTESIAN_POINT('Ctrl Pts',(-0.354653926942446,-6.75995835143459,
20.1804849958942));
#13693=CARTESIAN_POINT('Ctrl Pts',(-0.179921288127777,-6.76686365373732,
20.1886805747745));
#13694=CARTESIAN_POINT('Ctrl Pts',(-0.00520334358890041,-6.76699799949841,
20.1968761536548));
#13695=CARTESIAN_POINT('Ctrl Pts',(0.169533463571664,-6.76713235976353,
20.2050726173333));
#13696=CARTESIAN_POINT('Ctrl Pts',(0.344255214392696,-6.76049430684536,
20.2132690810117));
#13697=CARTESIAN_POINT('Ctrl Pts',(0.51840140640271,-6.74711412248524,20.2214655446901));
#13698=CARTESIAN_POINT('Ctrl Pts',(0.69259808327754,-6.73373005921859,20.2296643845179));
#13699=CARTESIAN_POINT('Ctrl Pts',(0.866218511303148,-6.7135999988006,20.2378632243457));
#13700=CARTESIAN_POINT('Ctrl Pts',(1.0387077508507,-6.68680605433735,20.2460620641735));
#13701=CARTESIAN_POINT('Ctrl Pts',(1.21137716031634,-6.65998412283682,20.2542694679227));
#13702=CARTESIAN_POINT('Ctrl Pts',(1.38291266565133,-6.62648445604016,20.262476871672));
#13703=CARTESIAN_POINT('Ctrl Pts',(1.55276896648187,-6.58644042990832,20.2706842754212));
#13704=CARTESIAN_POINT('Ctrl Pts',(1.72271625133604,-6.54637495407692,20.2788960754902));
#13705=CARTESIAN_POINT('Ctrl Pts',(1.89098219308985,-6.49975822630718,20.2871078755593));
#13706=CARTESIAN_POINT('Ctrl Pts',(2.0570371872062,-6.44677337979635,20.2953196756283));
#13707=CARTESIAN_POINT('Ctrl Pts',(2.22333663747637,-6.393710532188,20.3035435646145));
#13708=CARTESIAN_POINT('Ctrl Pts',(2.38741829806059,-6.33426095287712,20.3117674536006));
#13709=CARTESIAN_POINT('Ctrl Pts',(2.54877185531134,-6.26865623794867,20.3199913425867));
#13710=CARTESIAN_POINT('Ctrl Pts',(2.69785975275912,-6.20803861551756,20.3275900738368));
#13711=CARTESIAN_POINT('Ctrl Pts',(2.84461859164236,-6.1421667003386,20.3351888050869));
#13712=CARTESIAN_POINT('Ctrl Pts',(2.98866572065,-6.07125738296538,20.3427875363369));
#13713=CARTESIAN_POINT('Ctrl Pts',(3.14458198460576,-5.99450530938605,20.3510123846589));
#13714=CARTESIAN_POINT('Ctrl Pts',(3.29775856464863,-5.91163551488225,20.359237232981));
#13715=CARTESIAN_POINT('Ctrl Pts',(3.44768222515461,-5.82286667152469,20.367462081303));
#13716=CARTESIAN_POINT('Ctrl Pts',(3.59743703837766,-5.73419780156664,20.3756776666222));
#13717=CARTESIAN_POINT('Ctrl Pts',(3.74394592114233,-5.63964329305354,20.3838932519414));
#13718=CARTESIAN_POINT('Ctrl Pts',(3.88671728283139,-5.53946908677536,20.3921088372606));
#13719=CARTESIAN_POINT('Ctrl Pts',(4.0293565379205,-5.43938757187195,20.4003168206838));
#13720=CARTESIAN_POINT('Ctrl Pts',(4.16826486743913,-5.33369691971145,20.408524804107));
#13721=CARTESIAN_POINT('Ctrl Pts',(4.30297681881327,-5.22270806160517,20.4167327875303));
#13722=CARTESIAN_POINT('Ctrl Pts',(4.4375911785558,-5.11179960901334,20.4249348247068));
#13723=CARTESIAN_POINT('Ctrl Pts',(4.56801493959037,-4.99560082279134,20.4331368618833));
#13724=CARTESIAN_POINT('Ctrl Pts',(4.69381303428616,-4.87446491413831,20.4413388990598));
#13725=CARTESIAN_POINT('Ctrl Pts',(4.819545256338,-4.75339243683215,20.4495366413392));
#13726=CARTESIAN_POINT('Ctrl Pts',(4.94065637958802,-4.62738823562199,20.4577343836186));
#13727=CARTESIAN_POINT('Ctrl Pts',(5.05674568048418,-4.49684468521035,20.465932125898));
#13728=CARTESIAN_POINT('Ctrl Pts',(5.1728129089207,-4.36632595549472,20.4741283095124));
#13729=CARTESIAN_POINT('Ctrl Pts',(5.28385997404797,-4.23126985941285,20.4823244931267));
#13730=CARTESIAN_POINT('Ctrl Pts',(5.38952398716172,-4.09210461643008,20.4905206767411));
#13731=CARTESIAN_POINT('Ctrl Pts',(5.49518022192991,-3.95294961795082,20.4987162570019));
#13732=CARTESIAN_POINT('Ctrl Pts',(5.59545397616269,-3.8096863602303,20.5069118372628));
#13733=CARTESIAN_POINT('Ctrl Pts',(5.69002358507626,-3.662774986438,20.5151074175237));
#13734=CARTESIAN_POINT('Ctrl Pts',(5.78460343816883,-3.51584769858592,20.5233038855644));
#13735=CARTESIAN_POINT('Ctrl Pts',(5.87347772063902,-3.36527180912787,20.5315003536051));
#13736=CARTESIAN_POINT('Ctrl Pts',(5.95636890063675,-3.21153522781977,20.5396968216459));
#13737=CARTESIAN_POINT('Ctrl Pts',(6.03928414089027,-3.05775402244587,20.5478956688193));
#13738=CARTESIAN_POINT('Ctrl Pts',(6.11621264918396,-2.90081061357969,20.5560945159927));
#13739=CARTESIAN_POINT('Ctrl Pts',(6.18692350580496,-2.74121625073945,20.5642933631661));
#13740=CARTESIAN_POINT('Ctrl Pts',(6.25770826214694,-2.58145509627134,20.5725007789321));
#13741=CARTESIAN_POINT('Ctrl Pts',(6.32226223900874,-2.41903778123316,20.5807081946981));
#13742=CARTESIAN_POINT('Ctrl Pts',(6.38040285408827,-2.25449515846503,20.588915610464));
#13743=CARTESIAN_POINT('Ctrl Pts',(6.43857463049258,-2.08986434663835,20.5971274251162));
#13744=CARTESIAN_POINT('Ctrl Pts',(6.49032608644602,-1.92310629865883,20.6053392397683));
#13745=CARTESIAN_POINT('Ctrl Pts',(6.53552498470891,-1.75476556104959,20.6135510544205));
#13746=CARTESIAN_POINT('Ctrl Pts',(6.5807904452208,-1.58617691611236,20.6217749622181));
#13747=CARTESIAN_POINT('Ctrl Pts',(6.61948398395507,-1.4160012735088,20.6299988700157));
#13748=CARTESIAN_POINT('Ctrl Pts',(6.65152456319241,-1.24479314958272,20.6382227778133));
#13749=CARTESIAN_POINT('Ctrl Pts',(6.68112946667294,-1.08660000499665,20.6458215167368));
#13750=CARTESIAN_POINT('Ctrl Pts',(6.70505500320042,-0.927525685242328,
20.6534202556602));
#13751=CARTESIAN_POINT('Ctrl Pts',(6.72327677779544,-0.76800935486266,20.6610189945837));
#13752=CARTESIAN_POINT('Ctrl Pts',(6.74282283160828,-0.596900072318996,
20.669169976758));
#13753=CARTESIAN_POINT('Ctrl Pts',(6.7558631551989,-0.424775329034652,20.6773209589323));
#13754=CARTESIAN_POINT('Ctrl Pts',(6.76229963874382,-0.252175724139254,
20.6854719411065));
#13755=CARTESIAN_POINT('Ctrl Pts',(6.76872864571657,-0.0797766096819023,
20.6936134551596));
#13756=CARTESIAN_POINT('Ctrl Pts',(6.76856906881038,0.0930959066924904,
20.7017549692126));
#13757=CARTESIAN_POINT('Ctrl Pts',(6.76177415979962,0.265893233960796,20.7098964832656));
#13758=CARTESIAN_POINT('Ctrl Pts',(6.75498571380733,0.438526204014682,20.7180302534687));
#13759=CARTESIAN_POINT('Ctrl Pts',(6.7415745147216,0.61108376443959,20.7261640236718));
#13760=CARTESIAN_POINT('Ctrl Pts',(6.72154575992354,0.783014429786534,20.7342977938749));
#13761=CARTESIAN_POINT('Ctrl Pts',(6.70153184313653,0.954817722806097,20.7424255382929));
#13762=CARTESIAN_POINT('Ctrl Pts',(6.67491017445478,1.12599468377619,20.7505532827109));
#13763=CARTESIAN_POINT('Ctrl Pts',(6.641737965366,1.29599606458348,20.7586810271289));
#13764=CARTESIAN_POINT('Ctrl Pts',(6.60858335721769,1.46590724385568,20.766804459023));
#13765=CARTESIAN_POINT('Ctrl Pts',(6.56888520041666,1.63464372704615,20.774927890917));
#13766=CARTESIAN_POINT('Ctrl Pts',(6.52275227273907,1.80166361690447,20.7830513228111));
#13767=CARTESIAN_POINT('Ctrl Pts',(6.47632669591376,1.9697430152501,20.7912262865619));
#13768=CARTESIAN_POINT('Ctrl Pts',(6.42338447627585,2.13608359423184,20.7994012503127));
#13769=CARTESIAN_POINT('Ctrl Pts',(6.36408837673153,2.3001452417512,20.8075762140636));
#13770=CARTESIAN_POINT('Ctrl Pts',(6.30517942315793,2.46313572596849,20.8156978032366));
#13771=CARTESIAN_POINT('Ctrl Pts',(6.23999946279605,2.62387660952087,20.8238193924096));
#13772=CARTESIAN_POINT('Ctrl Pts',(6.16875747958513,2.78185552429715,20.8319409815827));
#13773=CARTESIAN_POINT('Ctrl Pts',(6.0975060909713,2.93985529553022,20.840063642972));
#13774=CARTESIAN_POINT('Ctrl Pts',(6.02019123589836,3.09509203803165,20.8481863043614));
#13775=CARTESIAN_POINT('Ctrl Pts',(5.937069142705,3.24707545257885,20.8563089657508));
#13776=CARTESIAN_POINT('Ctrl Pts',(5.85392024678543,3.39910787419136,20.864434246293));
#13777=CARTESIAN_POINT('Ctrl Pts',(5.76496055945822,3.54788455796296,20.8725595268353));
#13778=CARTESIAN_POINT('Ctrl Pts',(5.67049112359437,3.69294183778156,20.8806848073775));
#13779=CARTESIAN_POINT('Ctrl Pts',(5.57499246282927,3.8395794865643,20.8888986111653));
#13780=CARTESIAN_POINT('Ctrl Pts',(5.47386350464339,3.98241589044244,20.897112414953));
#13781=CARTESIAN_POINT('Ctrl Pts',(5.36745822332432,4.12100487998597,20.9053262187408));
#13782=CARTESIAN_POINT('Ctrl Pts',(5.26201756807798,4.25833747932921,20.913465559596));
#13783=CARTESIAN_POINT('Ctrl Pts',(5.15139614488266,4.39149911872647,20.9216049004511));
#13784=CARTESIAN_POINT('Ctrl Pts',(5.03597652983962,4.52009174585036,20.9297442413063));
#13785=CARTESIAN_POINT('Ctrl Pts',(4.91897303659917,4.65044902154262,20.9379952765603));
#13786=CARTESIAN_POINT('Ctrl Pts',(4.79703898083779,4.77611069478899,20.9462463118144));
#13787=CARTESIAN_POINT('Ctrl Pts',(4.67060837656458,4.89670362517121,20.9544973470684));
#13788=CARTESIAN_POINT('Ctrl Pts',(4.54417777229138,5.0172965555534,20.9627483823225));
#13789=CARTESIAN_POINT('Ctrl Pts',(4.41325095172409,5.13282053937636,20.9709994175765));
#13790=CARTESIAN_POINT('Ctrl Pts',(4.2782928526313,5.24294757432533,20.9792504528306));
#13791=CARTESIAN_POINT('Ctrl Pts',(4.14363336315362,5.35283094111553,20.987483231763));
#13792=CARTESIAN_POINT('Ctrl Pts',(4.00454009237542,5.45768443132887,20.9957160106954));
#13793=CARTESIAN_POINT('Ctrl Pts',(3.86142383748823,5.55713009990568,21.0039487896279));
#13794=CARTESIAN_POINT('Ctrl Pts',(3.71850616935632,5.65643777861778,21.0121701448345));
#13795=CARTESIAN_POINT('Ctrl Pts',(3.57157692998338,5.75035238284981,21.0203915000411));
#13796=CARTESIAN_POINT('Ctrl Pts',(3.42108087175425,5.83853531880361,21.0286128552477));
#13797=CARTESIAN_POINT('Ctrl Pts',(3.31548021184615,5.90041186453465,21.0343816477688));
#13798=CARTESIAN_POINT('Ctrl Pts',(3.20812414316205,5.95946715018402,21.0401504402898));
#13799=CARTESIAN_POINT('Ctrl Pts',(3.09917575053256,6.01559628526641,21.0459192328109));
#13800=CARTESIAN_POINT('Ctrl Pts',(3.09917575053257,6.0155962852664,19.0456175016683));
#13801=CARTESIAN_POINT('Ctrl Pts',(2.94686581755147,6.09406485737061,19.0536989022288));
#13802=CARTESIAN_POINT('Ctrl Pts',(2.79173928855776,6.16666014621092,19.0617803027892));
#13803=CARTESIAN_POINT('Ctrl Pts',(2.63429393795789,6.23320017715125,19.0698617033497));
#13804=CARTESIAN_POINT('Ctrl Pts',(2.46585430923732,6.30438664321037,19.0785074214021));
#13805=CARTESIAN_POINT('Ctrl Pts',(2.29437685241815,6.36880518518817,19.0871531394545));
#13806=CARTESIAN_POINT('Ctrl Pts',(2.12042019058826,6.42620472871396,19.0957988575068));
#13807=CARTESIAN_POINT('Ctrl Pts',(1.94668685366066,6.4835305829236,19.1044334762192));
#13808=CARTESIAN_POINT('Ctrl Pts',(1.77048094661389,6.53385531190139,19.1130680949316));
#13809=CARTESIAN_POINT('Ctrl Pts',(1.59238088160172,6.57697591054653,19.1217027136439));
#13810=CARTESIAN_POINT('Ctrl Pts',(1.40799101415761,6.62161936122547,19.1306422735464));
#13811=CARTESIAN_POINT('Ctrl Pts',(1.22157104283931,6.65854039925769,19.1395818334488));
#13812=CARTESIAN_POINT('Ctrl Pts',(1.03378289244469,6.68756920945785,19.1485213933512));
#13813=CARTESIAN_POINT('Ctrl Pts',(0.852903892918512,6.71552998406161,19.1571320466217));
#13814=CARTESIAN_POINT('Ctrl Pts',(0.67075593199652,6.73616881881119,19.1657426998922));
#13815=CARTESIAN_POINT('Ctrl Pts',(0.487943993382733,6.74938513194511,19.1743533531627));
#13816=CARTESIAN_POINT('Ctrl Pts',(0.305305098499116,6.76258893495447,19.1829558558738));
#13817=CARTESIAN_POINT('Ctrl Pts',(0.122003782177149,6.76838420221161,19.1915583585849));
#13818=CARTESIAN_POINT('Ctrl Pts',(-0.0613479792059813,6.76672191134284,
19.2001608612961));
#13819=CARTESIAN_POINT('Ctrl Pts',(-0.244493381872622,6.76506149134899,
19.2087536820635));
#13820=CARTESIAN_POINT('Ctrl Pts',(-0.427688812005436,6.7559602604347,19.217346502831));
#13821=CARTESIAN_POINT('Ctrl Pts',(-0.610320190322639,6.73942121144572,
19.2259393235985));
#13822=CARTESIAN_POINT('Ctrl Pts',(-0.63184412781484,6.73747200939787,19.2269520265567));
#13823=CARTESIAN_POINT('Ctrl Pts',(-0.653360229137335,6.73541955783007,
19.2279647295149));
#13824=CARTESIAN_POINT('Ctrl Pts',(-0.67486748832631,6.73326390936819,19.2289774324731));
#13825=CARTESIAN_POINT('Ctrl Pts',(-0.857409106226856,6.71496796777942,
19.2375726902332));
#13826=CARTESIAN_POINT('Ctrl Pts',(-1.03909871287128,6.68925533611982,19.2461679479932));
#13827=CARTESIAN_POINT('Ctrl Pts',(-1.21933193254209,6.65623907610621,19.2547632057533));
#13828=CARTESIAN_POINT('Ctrl Pts',(-1.39973393297972,6.62319189776526,19.2633665126077));
#13829=CARTESIAN_POINT('Ctrl Pts',(-1.57867652380709,6.58282749410883,19.2719698194621));
#13830=CARTESIAN_POINT('Ctrl Pts',(-1.75556754650928,6.53530960166719,19.2805731263166));
#13831=CARTESIAN_POINT('Ctrl Pts',(-1.93979253235329,6.48582160092713,19.2895331292566));
#13832=CARTESIAN_POINT('Ctrl Pts',(-2.12179184305956,6.42857441130441,19.2984931321966));
#13833=CARTESIAN_POINT('Ctrl Pts',(-2.30091763490059,6.3638091609824,19.3074531351366));
#13834=CARTESIAN_POINT('Ctrl Pts',(-2.47338299350447,6.3014520765723,19.3160799783413));
#13835=CARTESIAN_POINT('Ctrl Pts',(-2.64318441557393,6.23212609278477,19.324706821546));
#13836=CARTESIAN_POINT('Ctrl Pts',(-2.8097667941681,6.15609450564157,19.3333336647508));
#13837=CARTESIAN_POINT('Ctrl Pts',(-2.97650838340709,6.07999025152052,19.3419687530369));
#13838=CARTESIAN_POINT('Ctrl Pts',(-3.14002451471794,5.99716773639052,19.350603841323));
#13839=CARTESIAN_POINT('Ctrl Pts',(-3.29978523525656,5.90793588329992,19.3592389296092));
#13840=CARTESIAN_POINT('Ctrl Pts',(-3.45978323252651,5.81857150300013,19.3678868427343));
#13841=CARTESIAN_POINT('Ctrl Pts',(-3.61601441093366,5.72277891785642,19.3765347558595));
#13842=CARTESIAN_POINT('Ctrl Pts',(-3.76797705164576,5.62091077480073,19.3851826689846));
#13843=CARTESIAN_POINT('Ctrl Pts',(-3.78502494657996,5.60948271990633,19.3861528331886));
#13844=CARTESIAN_POINT('Ctrl Pts',(-3.80201915402101,5.59797824357036,19.3871229973926));
#13845=CARTESIAN_POINT('Ctrl Pts',(-3.81895899163695,5.58639787521398,19.3880931615965));
#13846=CARTESIAN_POINT('Ctrl Pts',(-3.96180337141138,5.48874696657306,19.3962740253766));
#13847=CARTESIAN_POINT('Ctrl Pts',(-4.10109921560093,5.38547745589563,19.4044548891568));
#13848=CARTESIAN_POINT('Ctrl Pts',(-4.23637342288947,5.27687684353499,19.4126357529369));
#13849=CARTESIAN_POINT('Ctrl Pts',(-4.37150439222093,5.16839122523096,19.4208079542363));
#13850=CARTESIAN_POINT('Ctrl Pts',(-4.50262192258611,5.05458596943124,19.4289801555357));
#13851=CARTESIAN_POINT('Ctrl Pts',(-4.62928112906176,4.93579225941619,19.4371523568351));
#13852=CARTESIAN_POINT('Ctrl Pts',(-4.75583236725597,4.8170998128866,19.4453175918937));
#13853=CARTESIAN_POINT('Ctrl Pts',(-4.8779325861,4.6934276263923,19.4534828269523));
#13854=CARTESIAN_POINT('Ctrl Pts',(-4.99516927669712,4.56514763147274,19.4616480620109));
#13855=CARTESIAN_POINT('Ctrl Pts',(-5.11233022516387,4.43695051333902,19.4698080218243));
#13856=CARTESIAN_POINT('Ctrl Pts',(-5.22463365932423,4.30415178243408,19.4779679816376));
#13857=CARTESIAN_POINT('Ctrl Pts',(-5.33170329322226,4.16716078320035,19.4861279414509));
#13858=CARTESIAN_POINT('Ctrl Pts',(-5.43872584437381,4.03023002431911,19.4942843130077));
#13859=CARTESIAN_POINT('Ctrl Pts',(-5.54051895685914,3.88911095464416,19.5024406845644));
#13860=CARTESIAN_POINT('Ctrl Pts',(-5.63674606322884,3.74424662898616,19.5105970561212));
#13861=CARTESIAN_POINT('Ctrl Pts',(-5.732967112403,3.59939142208462,19.5187529142598));
#13862=CARTESIAN_POINT('Ctrl Pts',(-5.82362264514526,3.45079172577715,19.5269087723985));
#13863=CARTESIAN_POINT('Ctrl Pts',(-5.90841877517819,3.29892051694518,19.5350646305372));
#13864=CARTESIAN_POINT('Ctrl Pts',(-5.99321614319239,3.14704709086921,19.5432206077473));
#13865=CARTESIAN_POINT('Ctrl Pts',(-6.07215376042459,2.99190237360781,19.5513765849574));
#13866=CARTESIAN_POINT('Ctrl Pts',(-6.14498326134584,2.83398477726672,19.5595325621675));
#13867=CARTESIAN_POINT('Ctrl Pts',(-6.21782743848746,2.67603535819696,19.5676901829276));
#13868=CARTESIAN_POINT('Ctrl Pts',(-6.28456089576236,2.51531227665795,19.5758478036876));
#13869=CARTESIAN_POINT('Ctrl Pts',(-6.34498306284489,2.35233478319125,19.5840054244476));
#13870=CARTESIAN_POINT('Ctrl Pts',(-6.40542870009563,2.18929398333603,19.5921662139243));
#13871=CARTESIAN_POINT('Ctrl Pts',(-6.4595580387042,2.02399736752226,19.6003270034011));
#13872=CARTESIAN_POINT('Ctrl Pts',(-6.5072201019049,1.85698022212537,19.6084877928778));
#13873=CARTESIAN_POINT('Ctrl Pts',(-6.55493670145495,1.68977197074656,19.6166579201725));
#13874=CARTESIAN_POINT('Ctrl Pts',(-6.59617114600952,1.52083960689443,19.6248280474671));
#13875=CARTESIAN_POINT('Ctrl Pts',(-6.63082319994865,1.35073042870248,19.6329981747617));
#13876=CARTESIAN_POINT('Ctrl Pts',(-6.66549711024586,1.18051395623243,19.6411734552639));
#13877=CARTESIAN_POINT('Ctrl Pts',(-6.69358029800513,1.0091195473852,19.6493487357661));
#13878=CARTESIAN_POINT('Ctrl Pts',(-6.7150243541446,0.837100306561233,19.6575240162684));
#13879=CARTESIAN_POINT('Ctrl Pts',(-6.73649992711584,0.664828245028345,
19.6657113121719));
#13880=CARTESIAN_POINT('Ctrl Pts',(-6.75131684692723,0.491929877684113,
19.6738986080754));
#13881=CARTESIAN_POINT('Ctrl Pts',(-6.75947878720754,0.31896006849034,19.682085903979));
#13882=CARTESIAN_POINT('Ctrl Pts',(-6.76449449881954,0.212665896920379,
19.6871171972406));
#13883=CARTESIAN_POINT('Ctrl Pts',(-6.76699804858992,0.106344709920844,
19.6921484905023));
#13884=CARTESIAN_POINT('Ctrl Pts',(-6.76699999885939,0.000124246054141125,
19.6971797837639));
#13885=CARTESIAN_POINT('',(-6.76699834151218,-0.0027926855951009,19.3028202161899));
#13886=CARTESIAN_POINT('Ctrl Pts',(3.0991757505326,6.01559628526638,18.6513920151221));
#13887=CARTESIAN_POINT('Ctrl Pts',(2.93382384459268,6.10078395293758,18.6601414630345));
#13888=CARTESIAN_POINT('Ctrl Pts',(2.76495772122988,6.17915010267047,18.6688909109469));
#13889=CARTESIAN_POINT('Ctrl Pts',(2.59315093316717,6.25042856433175,18.6776403588593));
#13890=CARTESIAN_POINT('Ctrl Pts',(2.4213455324562,6.3217064504145,18.6863897361193));
#13891=CARTESIAN_POINT('Ctrl Pts',(2.24659977927591,6.38589665313457,18.6951391133793));
#13892=CARTESIAN_POINT('Ctrl Pts',(2.06950718689916,6.44278115439076,18.7038884906393));
#13893=CARTESIAN_POINT('Ctrl Pts',(1.89241596572865,6.49966521519723,18.712637800154));
#13894=CARTESIAN_POINT('Ctrl Pts',(1.71297821457207,6.54924360009543,18.7213871096686));
#13895=CARTESIAN_POINT('Ctrl Pts',(1.53180337335861,6.59134792173552,18.7301364191833));
#13896=CARTESIAN_POINT('Ctrl Pts',(1.35062987477793,6.63345193135303,18.7388856638594));
#13897=CARTESIAN_POINT('Ctrl Pts',(1.16771959102957,6.66808192368237,18.7476349085355));
#13898=CARTESIAN_POINT('Ctrl Pts',(0.98369374690684,6.69512028363168,18.7563841532117));
#13899=CARTESIAN_POINT('Ctrl Pts',(0.799669205419867,6.72215845218867,18.7651333359558));
#13900=CARTESIAN_POINT('Ctrl Pts',(0.614529402873472,6.74160505424579,18.7738825187));
#13901=CARTESIAN_POINT('Ctrl Pts',(0.428903127363245,6.75339404354122,18.7826317014442));
#13902=CARTESIAN_POINT('Ctrl Pts',(0.243278104163867,6.7651829533033,18.7913808251628));
#13903=CARTESIAN_POINT('Ctrl Pts',(0.0571669005390976,6.76931433552276,
18.8001299488814));
#13904=CARTESIAN_POINT('Ctrl Pts',(-0.128798404777541,6.76577415902473,
18.8088790726));
#13905=CARTESIAN_POINT('Ctrl Pts',(-0.314762517259088,6.76223400523441,
18.8176281401992));
#13906=CARTESIAN_POINT('Ctrl Pts',(-0.500580446819462,6.75102239665089,
18.8263772077984));
#13907=CARTESIAN_POINT('Ctrl Pts',(-0.685621118842526,6.73217741012498,
18.8351262753976));
#13908=CARTESIAN_POINT('Ctrl Pts',(-0.870660665414259,6.71333253821774,
18.8438752897834));
#13909=CARTESIAN_POINT('Ctrl Pts',(-1.05492267885449,6.68685441030618,18.8526243041692));
#13910=CARTESIAN_POINT('Ctrl Pts',(-1.23778137635201,6.65283295028187,18.8613733185549));
#13911=CARTESIAN_POINT('Ctrl Pts',(-1.429999229788,6.61707018861876,18.8705701289223));
#13912=CARTESIAN_POINT('Ctrl Pts',(-1.62066601233652,6.57297172934424,18.8797669392897));
#13913=CARTESIAN_POINT('Ctrl Pts',(-1.80906628500346,6.52070304311305,18.8889637496571));
#13914=CARTESIAN_POINT('Ctrl Pts',(-1.98831342545488,6.47097374915043,18.8977137473949));
#13915=CARTESIAN_POINT('Ctrl Pts',(-2.16550875896663,6.41384933989542,18.9064637451327));
#13916=CARTESIAN_POINT('Ctrl Pts',(-2.34005036713972,6.3495238624049,18.9152137428704));
#13917=CARTESIAN_POINT('Ctrl Pts',(-2.51458843547052,6.28519968948611,18.9239635631513));
#13918=CARTESIAN_POINT('Ctrl Pts',(-2.6864726171802,6.21367483971114,18.9327133834321));
#13919=CARTESIAN_POINT('Ctrl Pts',(-2.85511905908698,6.13519226743859,18.941463203713));
#13920=CARTESIAN_POINT('Ctrl Pts',(-3.02376230488862,6.05671118252948,18.9502128581716));
#13921=CARTESIAN_POINT('Ctrl Pts',(-3.18916767379893,5.97127275992639,18.9589625126301));
#13922=CARTESIAN_POINT('Ctrl Pts',(-3.35077334102786,5.87916720437997,18.9677121670886));
#13923=CARTESIAN_POINT('Ctrl Pts',(-3.51237616037372,5.78706327195641,18.9764616673571));
#13924=CARTESIAN_POINT('Ctrl Pts',(-3.67017916302308,5.68829258362293,18.9852111676255));
#13925=CARTESIAN_POINT('Ctrl Pts',(-3.82364636566475,5.58319061741033,18.993960667894));
#13926=CARTESIAN_POINT('Ctrl Pts',(-3.97711106778813,5.47809036367691,19.0027100256024));
#13927=CARTESIAN_POINT('Ctrl Pts',(-4.12623987481945,5.36665920043212,19.0114593833108));
#13928=CARTESIAN_POINT('Ctrl Pts',(-4.27052628213949,5.24927559512319,19.0202087410193));
#13929=CARTESIAN_POINT('Ctrl Pts',(-4.41481053024993,5.13189374643023,19.0289579677958));
#13930=CARTESIAN_POINT('Ctrl Pts',(-4.55425230136541,5.00855981477343,19.0377071945723));
#13931=CARTESIAN_POINT('Ctrl Pts',(-4.68837800630554,4.87969268192071,19.0464564213488));
#13932=CARTESIAN_POINT('Ctrl Pts',(-4.82250188228897,4.75082730631807,19.0552055288197));
#13933=CARTESIAN_POINT('Ctrl Pts',(-4.95130963052964,4.61642907903527,19.0639546362905));
#13934=CARTESIAN_POINT('Ctrl Pts',(-5.07436379033362,4.47695444731695,19.0727037437614));
#13935=CARTESIAN_POINT('Ctrl Pts',(-5.19741643562807,4.33748153220584,19.0814527435511));
#13936=CARTESIAN_POINT('Ctrl Pts',(-5.31471544462781,4.19293255254579,19.0902017433409));
#13937=CARTESIAN_POINT('Ctrl Pts',(-5.42586245275641,4.04379841779585,19.0989507431306));
#13938=CARTESIAN_POINT('Ctrl Pts',(-5.53702160019161,3.89464799484331,19.1077006984728));
#13939=CARTESIAN_POINT('Ctrl Pts',(-5.64202723081255,3.74091164443845,19.1164506538149));
#13940=CARTESIAN_POINT('Ctrl Pts',(-5.74052265232966,3.58311159163235,19.1252006091571));
#13941=CARTESIAN_POINT('Ctrl Pts',(-5.83901427066916,3.42531763191787,19.1339502266395));
#13942=CARTESIAN_POINT('Ctrl Pts',(-5.93099603115737,3.26346052695618,19.142699844122));
#13943=CARTESIAN_POINT('Ctrl Pts',(-6.0161555062275,3.09809004467083,19.1514494616044));
#13944=CARTESIAN_POINT('Ctrl Pts',(-6.10131214578803,2.9327250686382,19.1601987877555));
#13945=CARTESIAN_POINT('Ctrl Pts',(-6.17964682328758,2.76384720416873,19.1689481139066));
#13946=CARTESIAN_POINT('Ctrl Pts',(-6.25089348288579,2.59203002791557,19.1776974400577));
#13947=CARTESIAN_POINT('Ctrl Pts',(-6.32213814889351,2.42021765936975,19.1864465213893));
#13948=CARTESIAN_POINT('Ctrl Pts',(-6.38629508412611,2.24546640831846,19.1951956027209));
#13949=CARTESIAN_POINT('Ctrl Pts',(-6.44314639819841,2.06836976659952,19.2039446840524));
#13950=CARTESIAN_POINT('Ctrl Pts',(-6.50000285283728,1.8912571115818,19.2126945564868));
#13951=CARTESIAN_POINT('Ctrl Pts',(-6.54955227673276,1.71179891440153,19.2214444289212));
#13952=CARTESIAN_POINT('Ctrl Pts',(-6.5916263592641,1.53060476278324,19.2301943013556));
#13953=CARTESIAN_POINT('Ctrl Pts',(-6.63369752055216,1.34942319164596,19.2389435662781));
#13954=CARTESIAN_POINT('Ctrl Pts',(-6.6682943142427,1.16650618642613,19.2476928312006));
#13955=CARTESIAN_POINT('Ctrl Pts',(-6.69529923745429,0.982474997617727,
19.2564420961231));
#13956=CARTESIAN_POINT('Ctrl Pts',(-6.72230554731454,0.798434359176876,
19.2651918103028));
#13957=CARTESIAN_POINT('Ctrl Pts',(-6.74171916496711,0.61327970623944,19.2739415244825));
#13958=CARTESIAN_POINT('Ctrl Pts',(-6.75347414817281,0.427639953654448,
19.2826912386622));
#13959=CARTESIAN_POINT('Ctrl Pts',(-6.76248837758747,0.285283364197852,
19.2894008978381));
#13960=CARTESIAN_POINT('Ctrl Pts',(-6.76699999999997,0.142641701104605,
19.296110557014));
#13961=CARTESIAN_POINT('Ctrl Pts',(-6.767,1.26781560333738E-12,19.3028202161899));
#13962=CARTESIAN_POINT('Ctrl Pts',(-6.76699522683441,-0.00803741253624945,
19.3028202161899));
#13963=CARTESIAN_POINT('Ctrl Pts',(-6.76673659893204,-0.225785820121706,
19.313053212668));
#13964=CARTESIAN_POINT('Ctrl Pts',(-6.75596462743227,-0.443030194641021,
19.3232862091462));
#13965=CARTESIAN_POINT('Ctrl Pts',(-6.73484541930834,-0.658897699207909,
19.3335192056243));
#13966=CARTESIAN_POINT('Ctrl Pts',(-6.71331152130556,-0.87900390765003,
19.3439531338819));
#13967=CARTESIAN_POINT('Ctrl Pts',(-6.68102007315153,-1.09767877436092,
19.3543870621396));
#13968=CARTESIAN_POINT('Ctrl Pts',(-6.63819493462871,-1.31402321511825,
19.3648209903972));
#13969=CARTESIAN_POINT('Ctrl Pts',(-6.60923076601765,-1.4603446766781,19.3718778282208));
#13970=CARTESIAN_POINT('Ctrl Pts',(-6.57544915666674,-1.60560067636746,
19.3789346660444));
#13971=CARTESIAN_POINT('Ctrl Pts',(-6.53693137322275,-1.74951914015714,
19.385991503868));
#13972=CARTESIAN_POINT('Ctrl Pts',(-6.49199356254967,-1.91742549664685,
19.3942245540001));
#13973=CARTESIAN_POINT('Ctrl Pts',(-6.44051669011873,-2.08384480851689,
19.4024576041321));
#13974=CARTESIAN_POINT('Ctrl Pts',(-6.38261306167999,-2.24823030512268,
19.4106906542641));
#13975=CARTESIAN_POINT('Ctrl Pts',(-6.32477838756202,-2.41242004387065,
19.4189139000989));
#13976=CARTESIAN_POINT('Ctrl Pts',(-6.26053231483941,-2.57458045555605,
19.4271371459338));
#13977=CARTESIAN_POINT('Ctrl Pts',(-6.19003777798889,-2.73417653180447,
19.4353603917686));
#13978=CARTESIAN_POINT('Ctrl Pts',(-6.11961307966196,-2.89361449715761,
19.4435754908821));
#13979=CARTESIAN_POINT('Ctrl Pts',(-6.04295238902611,-3.05049286106434,
19.4517905899957));
#13980=CARTESIAN_POINT('Ctrl Pts',(-5.960267938881,-3.20429322889577,19.4600056891092));
#13981=CARTESIAN_POINT('Ctrl Pts',(-5.87764886024245,-3.35797199996097,
19.468214293248));
#13982=CARTESIAN_POINT('Ctrl Pts',(-5.78901567682439,-3.50857730794951,
19.4764228973869));
#13983=CARTESIAN_POINT('Ctrl Pts',(-5.69462811767156,-3.65561206932909,
19.4846315015258));
#13984=CARTESIAN_POINT('Ctrl Pts',(-5.60029630252679,-3.80255999397937,
19.4928352577748));
#13985=CARTESIAN_POINT('Ctrl Pts',(-5.50021707480888,-3.94594127225762,
19.5010390140238));
#13986=CARTESIAN_POINT('Ctrl Pts',(-5.39469540380842,-4.0852846290226,19.5092427702727));
#13987=CARTESIAN_POINT('Ctrl Pts',(-5.28920495401075,-4.22458675760044,
19.517444099237));
#13988=CARTESIAN_POINT('Ctrl Pts',(-5.17827548143832,-4.35985305698951,
19.5256454282013));
#13989=CARTESIAN_POINT('Ctrl Pts',(-5.06225460862956,-4.49064218986648,
19.5338467571656));
#13990=CARTESIAN_POINT('Ctrl Pts',(-4.9462497362068,-4.62141328567339,19.5420469550883));
#13991=CARTESIAN_POINT('Ctrl Pts',(-4.82515509906916,-4.74770817623819,
19.550247153011));
#13992=CARTESIAN_POINT('Ctrl Pts',(-4.69935785601289,-4.86911950368134,
19.5584473509337));
#13993=CARTESIAN_POINT('Ctrl Pts',(-4.57355516457748,-4.9905360895461,19.5666479040135));
#13994=CARTESIAN_POINT('Ctrl Pts',(-4.4430497192283,-5.10706844203911,19.5748484570934));
#13995=CARTESIAN_POINT('Ctrl Pts',(-4.30826473397986,-5.21834686293902,
19.5830490101732));
#13996=CARTESIAN_POINT('Ctrl Pts',(-4.17344948540597,-5.32965026922629,
19.5912514045264));
#13997=CARTESIAN_POINT('Ctrl Pts',(-4.03435305935044,-5.43569716629838,
19.5994537988797));
#13998=CARTESIAN_POINT('Ctrl Pts',(-3.89143089432966,-5.53615883033143,
19.6076561932329));
#13999=CARTESIAN_POINT('Ctrl Pts',(-3.7483750719605,-5.63671444368036,19.6158662582667));
#14000=CARTESIAN_POINT('Ctrl Pts',(-3.60148665609892,-5.7316741822211,19.6240763233006));
#14001=CARTESIAN_POINT('Ctrl Pts',(-3.45124994273824,-5.82075277200031,
19.6322863883344));
#14002=CARTESIAN_POINT('Ctrl Pts',(-3.30094132875186,-5.90987399321227,
19.6405003825597));
#14003=CARTESIAN_POINT('Ctrl Pts',(-3.14728153713205,-5.99310828323021,
19.648714376785));
#14004=CARTESIAN_POINT('Ctrl Pts',(-2.99077841709905,-6.0702169203262,19.6569283710103));
#14005=CARTESIAN_POINT('Ctrl Pts',(-2.83406193118852,-6.14743068217635,
19.6651535636455));
#14006=CARTESIAN_POINT('Ctrl Pts',(-2.67449469719987,-6.2185019550956,19.6733787562807));
#14007=CARTESIAN_POINT('Ctrl Pts',(-2.51260457361605,-6.2832401877251,19.6816039489159));
#14008=CARTESIAN_POINT('Ctrl Pts',(-2.36701713221715,-6.34145914167096,
19.6890008470358));
#14009=CARTESIAN_POINT('Ctrl Pts',(-2.21955149458719,-6.39455693454562,
19.6963977451558));
#14010=CARTESIAN_POINT('Ctrl Pts',(-2.07060046963125,-6.44242987506755,
19.7037946432757));
#14011=CARTESIAN_POINT('Ctrl Pts',(-1.89649700765637,-6.49838682254241,
19.7124406097666));
#14012=CARTESIAN_POINT('Ctrl Pts',(-1.71996884025011,-6.54733190881197,
19.7210865762575));
#14013=CARTESIAN_POINT('Ctrl Pts',(-1.54159478382049,-6.58906476842484,
19.7297325427484));
#14014=CARTESIAN_POINT('Ctrl Pts',(-1.36344889205843,-6.63074424603682,
19.7383674498727));
#14015=CARTESIAN_POINT('Ctrl Pts',(-1.18346211504224,-6.66522982388226,
19.7470023569971));
#14016=CARTESIAN_POINT('Ctrl Pts',(-1.0022286978934,-6.69237077851481,19.7556372641214));
#14017=CARTESIAN_POINT('Ctrl Pts',(-0.81497847757186,-6.72041279093522,
19.7645588431929));
#14018=CARTESIAN_POINT('Ctrl Pts',(-0.626397716056642,-6.74061400251836,
19.7734804222645));
#14019=CARTESIAN_POINT('Ctrl Pts',(-0.437156738393943,-6.75286479844494,
19.782402001336));
#14020=CARTESIAN_POINT('Ctrl Pts',(-0.254502389179452,-6.7646891991903,
19.7910130603117));
#14021=CARTESIAN_POINT('Ctrl Pts',(-0.0712333493827942,-6.76910723061142,
19.7996241192873));
#14022=CARTESIAN_POINT('Ctrl Pts',(0.112038797017181,-6.76607244329847,
19.808235178263));
#14023=CARTESIAN_POINT('Ctrl Pts',(0.295138109321486,-6.76304051793007,
19.8168381166126));
#14024=CARTESIAN_POINT('Ctrl Pts',(0.478240218476588,-6.75256979155271,
19.8254410549621));
#14025=CARTESIAN_POINT('Ctrl Pts',(0.660731158458518,-6.73466579246826,
19.8340439933116));
#14026=CARTESIAN_POINT('Ctrl Pts',(0.843017750805112,-6.71678184172087,
19.8426372983603));
#14027=CARTESIAN_POINT('Ctrl Pts',(1.02469423641944,-6.69148125322093,19.8512306034091));
#14028=CARTESIAN_POINT('Ctrl Pts',(1.20514917349521,-6.65882155261904,19.8598239084579));
#14029=CARTESIAN_POINT('Ctrl Pts',(1.2252548072328,-6.65518272738698,19.8607813432984));
#14030=CARTESIAN_POINT('Ctrl Pts',(1.2453452804058,-6.65145260219814,19.861738778139));
#14031=CARTESIAN_POINT('Ctrl Pts',(1.26541975028478,-6.64763129660402,19.8626962129795));
#14032=CARTESIAN_POINT('Ctrl Pts',(1.44564640244671,-6.61332398396923,19.8712919705271));
#14033=CARTESIAN_POINT('Ctrl Pts',(1.62437129409007,-6.5717032616975,19.8798877280747));
#14034=CARTESIAN_POINT('Ctrl Pts',(1.80100228832431,-6.52293490366496,19.8884834856222));
#14035=CARTESIAN_POINT('Ctrl Pts',(1.97779808528164,-6.47412104309625,19.8970872633039));
#14036=CARTESIAN_POINT('Ctrl Pts',(2.15249579092547,-6.41814631648068,19.9056910409855));
#14037=CARTESIAN_POINT('Ctrl Pts',(2.32451989163915,-6.35522590262329,19.9142948186671));
#14038=CARTESIAN_POINT('Ctrl Pts',(2.50330468993618,-6.28983266148097,19.9232367323351));
#14039=CARTESIAN_POINT('Ctrl Pts',(2.67920113432479,-6.21693689126618,19.9321786460032));
#14040=CARTESIAN_POINT('Ctrl Pts',(2.85158887552337,-6.13683386486806,19.9411205596712));
#14041=CARTESIAN_POINT('Ctrl Pts',(3.01790941694981,-6.05955007062722,19.9497477620019));
#14042=CARTESIAN_POINT('Ctrl Pts',(3.18096378271897,-5.97555787295674,19.9583749643326));
#14043=CARTESIAN_POINT('Ctrl Pts',(3.34022206281018,-5.88516827041641,19.9670021666633));
#14044=CARTESIAN_POINT('Ctrl Pts',(3.49963201203655,-5.79469258561502,19.9756375850837));
#14045=CARTESIAN_POINT('Ctrl Pts',(3.65523839899704,-5.69780749315107,19.9842730035042));
#14046=CARTESIAN_POINT('Ctrl Pts',(3.80654036991904,-5.59486723811894,19.9929084219246));
#14047=CARTESIAN_POINT('Ctrl Pts',(3.95806586795211,-5.49177490352247,20.0015565979457));
#14048=CARTESIAN_POINT('Ctrl Pts',(4.10527399472444,-5.38260970808873,20.0102047739669));
#14049=CARTESIAN_POINT('Ctrl Pts',(4.24769585966207,-5.26776697318795,20.018852949988));
#14050=CARTESIAN_POINT('Ctrl Pts',(4.26276355295241,-5.2556170472839,20.0197678942198));
#14051=CARTESIAN_POINT('Ctrl Pts',(4.27777770771166,-5.24340360825008,20.0206828384516));
#14052=CARTESIAN_POINT('Ctrl Pts',(4.29273779262652,-5.23112714849831,20.0215977826834));
#14053=CARTESIAN_POINT('Ctrl Pts',(4.42723948425975,-5.12075313569843,20.0298237752247));
#14054=CARTESIAN_POINT('Ctrl Pts',(4.5576581037315,-5.00504350632935,20.0380497677661));
#14055=CARTESIAN_POINT('Ctrl Pts',(4.68354503541923,-4.88433157158684,20.0462757603074));
#14056=CARTESIAN_POINT('Ctrl Pts',(4.80929999093065,-4.76374618770522,20.0544931289588));
#14057=CARTESIAN_POINT('Ctrl Pts',(4.93053246295187,-4.63816918767513,20.0627104976103));
#14058=CARTESIAN_POINT('Ctrl Pts',(5.04682600525942,-4.50797474179229,20.0709278662617));
#14059=CARTESIAN_POINT('Ctrl Pts',(5.16302089865326,-4.37789073661323,20.0791382643241));
#14060=CARTESIAN_POINT('Ctrl Pts',(5.2742849690863,-4.24319735225379,20.0873486623865));
#14061=CARTESIAN_POINT('Ctrl Pts',(5.3802377633856,-4.1043063493652,20.0955590604488));
#14062=CARTESIAN_POINT('Ctrl Pts',(5.48612187529514,-3.96550538059094,20.1037641362376));
#14063=CARTESIAN_POINT('Ctrl Pts',(5.58670135266541,-3.82251249726049,20.1119692120264));
#14064=CARTESIAN_POINT('Ctrl Pts',(5.68163521889898,-3.67577342056971,20.1201742878152));
#14065=CARTESIAN_POINT('Ctrl Pts',(5.77652653225256,-3.52910011777573,20.1283756857847));
#14066=CARTESIAN_POINT('Ctrl Pts',(5.86577708189894,-3.37868426723918,20.1365770837541));
#14067=CARTESIAN_POINT('Ctrl Pts',(5.9490884772207,-3.22500159537944,20.1447784817236));
#14068=CARTESIAN_POINT('Ctrl Pts',(6.03239334690032,-3.07133096122613,20.1529792372913));
#14069=CARTESIAN_POINT('Ctrl Pts',(6.10975981060414,-2.91439432601712,20.1611799928591));
#14070=CARTESIAN_POINT('Ctrl Pts',(6.18093464356704,-2.75469343701849,20.1693807484268));
#14071=CARTESIAN_POINT('Ctrl Pts',(6.25210911499566,-2.59499335922441,20.1775814623385));
#14072=CARTESIAN_POINT('Ctrl Pts',(6.31709187146914,-2.43252938251092,20.1857821762503));
#14073=CARTESIAN_POINT('Ctrl Pts',(6.37567726055921,-2.2678246116462,20.1939828901621));
#14074=CARTESIAN_POINT('Ctrl Pts',(6.43427296919467,-2.10309082879767,20.2021850485917));
#14075=CARTESIAN_POINT('Ctrl Pts',(6.48646894525464,-1.93611580306841,20.2103872070213));
#14076=CARTESIAN_POINT('Ctrl Pts',(6.53210895493344,-1.76743927784759,20.2185893654509));
#14077=CARTESIAN_POINT('Ctrl Pts',(6.57776527508248,-1.59870247232743,20.2267944551038));
#14078=CARTESIAN_POINT('Ctrl Pts',(6.61686086807522,-1.42826330172146,20.2349995447568));
#14079=CARTESIAN_POINT('Ctrl Pts',(6.64929028510915,-1.256673268735,20.2432046344097));
#14080=CARTESIAN_POINT('Ctrl Pts',(6.6817567489179,-1.08488721442299,20.2514190974075));
#14081=CARTESIAN_POINT('Ctrl Pts',(6.7075417560825,-0.911948023638369,20.2596335604053));
#14082=CARTESIAN_POINT('Ctrl Pts',(6.72659143378814,-0.738414980135131,
20.267848023403));
#14083=CARTESIAN_POINT('Ctrl Pts',(6.74565239782574,-0.564779123788346,
20.2760673532105));
#14084=CARTESIAN_POINT('Ctrl Pts',(6.75797005263394,-0.390549070252429,
20.284286683018));
#14085=CARTESIAN_POINT('Ctrl Pts',(6.76354267643597,-0.216285607540968,
20.2925060128255));
#14086=CARTESIAN_POINT('Ctrl Pts',(6.76912393468072,-0.0417521341593407,
20.3007380779862));
#14087=CARTESIAN_POINT('Ctrl Pts',(6.7679392791419,0.132814493732021,20.3089701431468));
#14088=CARTESIAN_POINT('Ctrl Pts',(6.76003909319362,0.306855761709051,20.3172022083075));
#14089=CARTESIAN_POINT('Ctrl Pts',(6.75293783879879,0.463296550216326,20.3246017795687));
#14090=CARTESIAN_POINT('Ctrl Pts',(6.74041135547517,0.619312751898104,20.3320013508299));
#14091=CARTESIAN_POINT('Ctrl Pts',(6.72253151655136,0.774505654578253,20.339400922091));
#14092=CARTESIAN_POINT('Ctrl Pts',(6.7028249356549,0.945554258777326,20.3475564905097));
#14093=CARTESIAN_POINT('Ctrl Pts',(6.67655368957025,1.11612924680917,20.3557120589283));
#14094=CARTESIAN_POINT('Ctrl Pts',(6.64374226276057,1.2856818214508,20.363867627347));
#14095=CARTESIAN_POINT('Ctrl Pts',(6.61097086302003,1.45502755679018,20.3720132466859));
#14096=CARTESIAN_POINT('Ctrl Pts',(6.57167523285376,1.62335300655458,20.3801588660248));
#14097=CARTESIAN_POINT('Ctrl Pts',(6.52593170486439,1.790112952706,20.3883044853637));
#14098=CARTESIAN_POINT('Ctrl Pts',(6.48023436084529,1.95670453326049,20.3964418806531));
#14099=CARTESIAN_POINT('Ctrl Pts',(6.42810217534318,2.12173340702392,20.4045792759425));
#14100=CARTESIAN_POINT('Ctrl Pts',(6.36966277152329,2.28466303359384,20.4127166712318));
#14101=CARTESIAN_POINT('Ctrl Pts',(6.31127008840033,2.44746240240607,20.4208475608973));
#14102=CARTESIAN_POINT('Ctrl Pts',(6.24658035008016,2.60816552330735,20.4289784505629));
#14103=CARTESIAN_POINT('Ctrl Pts',(6.1757714027542,2.76624955145473,20.4371093402284));
#14104=CARTESIAN_POINT('Ctrl Pts',(6.10500419044534,2.92424040437682,20.4452354375218));
#14105=CARTESIAN_POINT('Ctrl Pts',(6.02812510095207,3.07961490612009,20.4533615348153));
#14106=CARTESIAN_POINT('Ctrl Pts',(5.94536063683131,3.23186879344086,20.4614876321088));
#14107=CARTESIAN_POINT('Ctrl Pts',(5.86261858878466,3.38408144404898,20.4696115285157));
#14108=CARTESIAN_POINT('Ctrl Pts',(5.7739945103782,3.53317484009894,20.4777354249226));
#14109=CARTESIAN_POINT('Ctrl Pts',(5.67976160219044,3.67866784886636,20.4858593213295));
#14110=CARTESIAN_POINT('Ctrl Pts',(5.58553966311416,3.82414392162849,20.4939822720802));
#14111=CARTESIAN_POINT('Ctrl Pts',(5.48571039220702,3.96602013413904,20.502105222831));
#14112=CARTESIAN_POINT('Ctrl Pts',(5.38059115512394,4.10384305516208,20.5102281735818));
#14113=CARTESIAN_POINT('Ctrl Pts',(5.27546415673589,4.24167615211251,20.5183517240772));
#14114=CARTESIAN_POINT('Ctrl Pts',(5.16504663618726,4.37545507073959,20.5264752745726));
#14115=CARTESIAN_POINT('Ctrl Pts',(5.04969716750023,4.50475831943737,20.534598825068));
#14116=CARTESIAN_POINT('Ctrl Pts',(4.93431723734688,4.63409571451309,20.5427245208291));
#14117=CARTESIAN_POINT('Ctrl Pts',(4.81400300928169,4.75895481355426,20.5508502165902));
#14118=CARTESIAN_POINT('Ctrl Pts',(4.68915089294007,4.87894997957956,20.5589759123514));
#14119=CARTESIAN_POINT('Ctrl Pts',(4.56417402353802,4.99906504556841,20.5671097273614));
#14120=CARTESIAN_POINT('Ctrl Pts',(4.4346504728083,5.1143062170843,20.5752435423715));
#14121=CARTESIAN_POINT('Ctrl Pts',(4.30101144510691,5.22432670772602,20.5833773573816));
#14122=CARTESIAN_POINT('Ctrl Pts',(4.16730180463402,5.33440533147375,20.5915154701722));
#14123=CARTESIAN_POINT('Ctrl Pts',(4.02947264447767,5.43925755620232,20.5996535829629));
#14124=CARTESIAN_POINT('Ctrl Pts',(3.88798505814178,5.5385793474199,20.6077916957536));
#14125=CARTESIAN_POINT('Ctrl Pts',(3.74629840095428,5.63804088286575,20.6159412587434));
#14126=CARTESIAN_POINT('Ctrl Pts',(3.60094334091334,5.73195624109692,20.6240908217332));
#14127=CARTESIAN_POINT('Ctrl Pts',(3.45240745000457,5.82006630539146,20.6322403847231));
#14128=CARTESIAN_POINT('Ctrl Pts',(3.33651925814909,5.88881006808,20.6385987006394));
#14129=CARTESIAN_POINT('Ctrl Pts',(3.21869538117158,5.9540209528432,20.6449570165556));
#14130=CARTESIAN_POINT('Ctrl Pts',(3.09917575053258,6.01559628526639,20.6513153324719));
#14131=CARTESIAN_POINT('Origin',(0.,0.,-3.69717978381041));
#14132=CARTESIAN_POINT('',(3.09917575053259,6.01559628526639,23.0457515827422));
#14133=CARTESIAN_POINT('',(3.09917575053257,6.0155962852664,22.6516519666359));
#14134=CARTESIAN_POINT('',(3.09917575053259,6.01559628526639,-3.69717978381041));
#14135=CARTESIAN_POINT('',(-6.76724104181633,0.00151419972611408,21.6967615973392));
#14136=CARTESIAN_POINT('Ctrl Pts',(-6.767,1.39537968873079E-12,21.69717978381));
#14137=CARTESIAN_POINT('Ctrl Pts',(-6.76700000000004,-0.186007249414254,
21.705929295616));
#14138=CARTESIAN_POINT('Ctrl Pts',(-6.75932637295446,-0.372014355526077,
21.7146788074219));
#14139=CARTESIAN_POINT('Ctrl Pts',(-6.7440051826694,-0.557389537153566,
21.7234283192278));
#14140=CARTESIAN_POINT('Ctrl Pts',(-6.72868405709661,-0.742763935809995,
21.7321777940784));
#14141=CARTESIAN_POINT('Ctrl Pts',(-6.7057154565301,-0.927506129693716,
21.7409272689289));
#14142=CARTESIAN_POINT('Ctrl Pts',(-6.67517739415671,-1.11098863924852,
21.7496767437795));
#14143=CARTESIAN_POINT('Ctrl Pts',(-6.64463945823089,-1.2944703890656,21.7584261824015));
#14144=CARTESIAN_POINT('Ctrl Pts',(-6.60653217027141,-1.47669218228292,
21.7671756210235));
#14145=CARTESIAN_POINT('Ctrl Pts',(-6.56098496116688,-1.65703510504214,
21.7759250596455));
#14146=CARTESIAN_POINT('Ctrl Pts',(-6.51543793687491,-1.83737729604112,
21.7846744627657));
#14147=CARTESIAN_POINT('Ctrl Pts',(-6.46245112202611,-2.01584035397144,
21.7934238658859));
#14148=CARTESIAN_POINT('Ctrl Pts',(-6.40220448416212,-2.19181813638232,
21.8021732690062));
#14149=CARTESIAN_POINT('Ctrl Pts',(-6.3419580857515,-2.36779521936043,21.8109226373514));
#14150=CARTESIAN_POINT('Ctrl Pts',(-6.27445201489191,-2.54128677544937,
21.8196720056967));
#14151=CARTESIAN_POINT('Ctrl Pts',(-6.19991555136132,-2.7117035523796,21.828421374042));
#14152=CARTESIAN_POINT('Ctrl Pts',(-6.12537937788981,-2.88211966613193,
21.837170708339));
#14153=CARTESIAN_POINT('Ctrl Pts',(-6.04381298133555,-3.04946076210567,
21.8459200426361));
#14154=CARTESIAN_POINT('Ctrl Pts',(-5.95549339426239,-3.21315848206978,
21.8546693769332));
#14155=CARTESIAN_POINT('Ctrl Pts',(-5.86717414355097,-3.37685557859746,
21.8634186779087));
#14156=CARTESIAN_POINT('Ctrl Pts',(-5.77210188986179,-3.53690907467407,
21.8721679788843));
#14157=CARTESIAN_POINT('Ctrl Pts',(-5.67059953467014,-3.69277536784988,
21.8809172798598));
#14158=CARTESIAN_POINT('Ctrl Pts',(-5.56909755761717,-3.84864108035863,
21.8896665482406));
#14159=CARTESIAN_POINT('Ctrl Pts',(-5.46116568338027,-4.00031938104338,
21.8984158166213));
#14160=CARTESIAN_POINT('Ctrl Pts',(-5.34717048686078,-4.14729511663265,
21.9071650850021));
#14161=CARTESIAN_POINT('Ctrl Pts',(-5.23317570555477,-4.2942703168809,21.9159143215147));
#14162=CARTESIAN_POINT('Ctrl Pts',(-5.1131178217876,-4.43654275987182,21.9246635580273));
#14163=CARTESIAN_POINT('Ctrl Pts',(-4.98740459171965,-4.57362924147704,
21.93341279454));
#14164=CARTESIAN_POINT('Ctrl Pts',(-4.86169180910783,-4.71071523514485,
21.9421619999111));
#14165=CARTESIAN_POINT('Ctrl Pts',(-4.73032391415386,-4.84261509316568,
21.9509112052822));
#14166=CARTESIAN_POINT('Ctrl Pts',(-4.59374707237251,-4.96888084331563,
21.9596604106533));
#14167=CARTESIAN_POINT('Ctrl Pts',(-4.45717070537357,-5.09514615452764,
21.9684095856095));
#14168=CARTESIAN_POINT('Ctrl Pts',(-4.31538563819461,-5.21577720253672,
21.9771587605658));
#14169=CARTESIAN_POINT('Ctrl Pts',(-4.16887341290597,-5.3303642902869,21.985907935522));
#14170=CARTESIAN_POINT('Ctrl Pts',(-4.0223616847728,-5.4449509892122,21.9946570807899));
#14171=CARTESIAN_POINT('Ctrl Pts',(-3.87112305634373,-5.55349359238805,
22.0034062260578));
#14172=CARTESIAN_POINT('Ctrl Pts',(-3.71567117316659,-5.65562346102522,
22.0121553713258));
#14173=CARTESIAN_POINT('Ctrl Pts',(-3.56021980457203,-5.7577529915883,22.0209044876319));
#14174=CARTESIAN_POINT('Ctrl Pts',(-3.40055544862266,-5.85346967275425,
22.0296536039381));
#14175=CARTESIAN_POINT('Ctrl Pts',(-3.23722036323256,-5.94244842803642,
22.0384027202443));
#14176=CARTESIAN_POINT('Ctrl Pts',(-3.07388580495894,-6.03142689616553,
22.0471518083152));
#14177=CARTESIAN_POINT('Ctrl Pts',(-2.9068807925755,-6.11366734484897,22.0559008963862));
#14178=CARTESIAN_POINT('Ctrl Pts',(-2.73677251094454,-6.18889046787373,
22.0646499844571));
#14179=CARTESIAN_POINT('Ctrl Pts',(-2.56666476416532,-6.26411335438315,
22.0733990450193));
#14180=CARTESIAN_POINT('Ctrl Pts',(-2.3934540297203,-6.33231884350313,22.0821481055815));
#14181=CARTESIAN_POINT('Ctrl Pts',(-2.21772856474027,-6.39327529621047,
22.0908971661437));
#14182=CARTESIAN_POINT('Ctrl Pts',(-2.04200363768254,-6.45423156232087,
22.0996461999237));
#14183=CARTESIAN_POINT('Ctrl Pts',(-1.86376426620073,-6.50793874252062,
22.1083952337037));
#14184=CARTESIAN_POINT('Ctrl Pts',(-1.68361578194663,-6.55421443796129,
22.1171442674837));
#14185=CARTESIAN_POINT('Ctrl Pts',(-1.50346783419832,-6.60048999558688,
22.125893275208));
#14186=CARTESIAN_POINT('Ctrl Pts',(-1.321411062572,-6.63933404145505,22.1346422829322));
#14187=CARTESIAN_POINT('Ctrl Pts',(-1.13806375958987,-6.6706146552704,22.1433912906564));
#14188=CARTESIAN_POINT('Ctrl Pts',(-0.95471698741806,-6.70189517852497,
22.1521402730514));
#14189=CARTESIAN_POINT('Ctrl Pts',(-0.770079973808261,-6.72561226535848,
22.1608892554463));
#14190=CARTESIAN_POINT('Ctrl Pts',(-0.584779770550317,-6.74168536939801,
22.1696382378412));
#14191=CARTESIAN_POINT('Ctrl Pts',(-0.391490647551807,-6.75845143942406,
22.1787644185172));
#14192=CARTESIAN_POINT('Ctrl Pts',(-0.197480213102271,-6.76689975924032,
22.1878905991933));
#14193=CARTESIAN_POINT('Ctrl Pts',(-0.00346532629577278,-6.76699911271708,
22.1970167798693));
#14194=CARTESIAN_POINT('Ctrl Pts',(0.18448659529802,-6.76709536139768,22.2058577673993));
#14195=CARTESIAN_POINT('Ctrl Pts',(0.37244237818713,-6.75935659726759,22.2146987549292));
#14196=CARTESIAN_POINT('Ctrl Pts',(0.559750217723924,-6.74380965729001,
22.2235397424591));
#14197=CARTESIAN_POINT('Ctrl Pts',(0.745129914459503,-6.72842275717234,
22.2322897210569));
#14198=CARTESIAN_POINT('Ctrl Pts',(0.929874656315842,-6.7053877227345,22.2410396996546));
#14199=CARTESIAN_POINT('Ctrl Pts',(1.11335688289934,-6.67478280180716,22.2497896782524));
#14200=CARTESIAN_POINT('Ctrl Pts',(1.29683723119004,-6.64417819417994,22.2585395672773));
#14201=CARTESIAN_POINT('Ctrl Pts',(1.47905480730373,-6.60600390230044,22.2672894563023));
#14202=CARTESIAN_POINT('Ctrl Pts',(1.65939064804936,-6.56038959797102,22.2760393453272));
#14203=CARTESIAN_POINT('Ctrl Pts',(1.83972470264396,-6.51477574543219,22.2847891476882));
#14204=CARTESIAN_POINT('Ctrl Pts',(2.01817678125981,-6.46172209820059,22.2935389500491));
#14205=CARTESIAN_POINT('Ctrl Pts',(2.19414072347814,-6.40140886723968,22.3022887524101));
#14206=CARTESIAN_POINT('Ctrl Pts',(2.37010298132226,-6.34109621361326,22.3110384710155));
#14207=CARTESIAN_POINT('Ctrl Pts',(2.54357687927037,-6.2735242082592,22.319788189621));
#14208=CARTESIAN_POINT('Ctrl Pts',(2.7139731779009,-6.19892237325444,22.3285379082265));
#14209=CARTESIAN_POINT('Ctrl Pts',(2.88436790207318,-6.12432122756908,22.3372875459848));
#14210=CARTESIAN_POINT('Ctrl Pts',(3.05168482126372,-6.04269049717358,22.346037183743));
#14211=CARTESIAN_POINT('Ctrl Pts',(3.21535561997503,-5.95430745234868,22.3547868215013));
#14212=CARTESIAN_POINT('Ctrl Pts',(3.37902496075387,-5.86592519481455,22.3635363813203));
#14213=CARTESIAN_POINT('Ctrl Pts',(3.53904799384974,-5.77079087940171,22.3722859411393));
#14214=CARTESIAN_POINT('Ctrl Pts',(3.69488118815077,-5.66922763746964,22.3810355009583));
#14215=CARTESIAN_POINT('Ctrl Pts',(3.85071304610924,-5.56766526648989,22.3897849857458));
#14216=CARTESIAN_POINT('Ctrl Pts',(4.00235489706057,-5.45967423580648,22.3985344705332));
#14217=CARTESIAN_POINT('Ctrl Pts',(4.14929168607742,-5.3456213393626,22.4072839553207));
#14218=CARTESIAN_POINT('Ctrl Pts',(4.29622726385834,-5.23156938308467,22.416033367984));
#14219=CARTESIAN_POINT('Ctrl Pts',(4.43845763092134,-5.11145583677144,22.4247827806472));
#14220=CARTESIAN_POINT('Ctrl Pts',(4.57549970661019,-4.98568866204159,22.4335321933105));
#14221=CARTESIAN_POINT('Ctrl Pts',(4.71254069815356,-4.85992248226102,22.4422815367569));
#14222=CARTESIAN_POINT('Ctrl Pts',(4.84439326931379,-4.72850295733935,22.4510308802032));
#14223=CARTESIAN_POINT('Ctrl Pts',(4.97060959434767,-4.59187644221607,22.4597802236495));
#14224=CARTESIAN_POINT('Ctrl Pts',(5.0968249628059,-4.45525096256579,22.4685295007858));
#14225=CARTESIAN_POINT('Ctrl Pts',(5.21740397615918,-4.3134187821823,22.4772787779221));
#14226=CARTESIAN_POINT('Ctrl Pts',(5.33193710452017,-4.1668616143857,22.4860280550584));
#14227=CARTESIAN_POINT('Ctrl Pts',(5.44646940289459,-4.02030550864411,22.4947772687914));
#14228=CARTESIAN_POINT('Ctrl Pts',(5.55495572749733,-3.86902470980035,22.5035264825243));
#14229=CARTESIAN_POINT('Ctrl Pts',(5.65702762491518,-3.71353301465688,22.5122756962573));
#14230=CARTESIAN_POINT('Ctrl Pts',(5.75909881655215,-3.55804239466794,22.5210248494934));
#14231=CARTESIAN_POINT('Ctrl Pts',(5.85475551250843,-3.39834117619448,22.5297740027295));
#14232=CARTESIAN_POINT('Ctrl Pts',(5.94367283728154,-3.2349717469186,22.5385231559657));
#14233=CARTESIAN_POINT('Ctrl Pts',(6.03258957676364,-3.07160339300861,22.5472722516112));
#14234=CARTESIAN_POINT('Ctrl Pts',(6.11476689685331,-2.90456712829405,22.5560213472567));
#14235=CARTESIAN_POINT('Ctrl Pts',(6.18992570525302,-2.73443024475811,22.5647704429022));
#14236=CARTESIAN_POINT('Ctrl Pts',(6.26508404388744,-2.56429442462916,22.5735194838633));
#14237=CARTESIAN_POINT('Ctrl Pts',(6.33322384283366,-2.39105828655859,22.5822685248243));
#14238=CARTESIAN_POINT('Ctrl Pts',(6.39411368720086,-2.21531017131926,22.5910175657854));
#14239=CARTESIAN_POINT('Ctrl Pts',(6.45500317120933,-2.03956309619376,22.5997665549678));
#14240=CARTESIAN_POINT('Ctrl Pts',(6.50864269270108,-1.86130434438511,22.6085155441501));
#14241=CARTESIAN_POINT('Ctrl Pts',(6.55485008446361,-1.68113930719839,22.6172645333325));
#14242=CARTESIAN_POINT('Ctrl Pts',(6.60199664749428,-1.49731239211733,22.6261913468619));
#14243=CARTESIAN_POINT('Ctrl Pts',(6.64140563640928,-1.31150116499564,22.6351181603913));
#14244=CARTESIAN_POINT('Ctrl Pts',(6.6729377228219,-1.12436255155552,22.6440449739206));
#14245=CARTESIAN_POINT('Ctrl Pts',(6.70384494949887,-0.940932395050242,
22.6527948880762));
#14246=CARTESIAN_POINT('Ctrl Pts',(6.72718449348943,-0.756227260505593,
22.6615448022317));
#14247=CARTESIAN_POINT('Ctrl Pts',(6.74287707373942,-0.570874564540552,
22.6702947163872));
#14248=CARTESIAN_POINT('Ctrl Pts',(6.75856934538677,-0.385525513631337,
22.6790444584712));
#14249=CARTESIAN_POINT('Ctrl Pts',(6.76661493004106,-0.199529212417095,
22.6877942005552));
#14250=CARTESIAN_POINT('Ctrl Pts',(6.76698649908907,-0.0135174385992982,
22.6965439426392));
#14251=CARTESIAN_POINT('Ctrl Pts',(6.76735806132386,0.172490924446901,22.7052935242851));
#14252=CARTESIAN_POINT('Ctrl Pts',(6.76005588896283,0.358514472902524,22.714043105931));
#14253=CARTESIAN_POINT('Ctrl Pts',(6.74510478454576,0.54392135966332,22.7227926875769));
#14254=CARTESIAN_POINT('Ctrl Pts',(6.73015393440676,0.729325093151587,22.7315421204159));
#14255=CARTESIAN_POINT('Ctrl Pts',(6.70755443556881,0.914111900257527,22.740291553255));
#14256=CARTESIAN_POINT('Ctrl Pts',(6.67738304682299,1.09765415591659,22.749040986094));
#14257=CARTESIAN_POINT('Ctrl Pts',(6.64721213111836,1.28119353391399,22.7577902817553));
#14258=CARTESIAN_POINT('Ctrl Pts',(6.60946960955465,1.46348811672784,22.7665395774166));
#14259=CARTESIAN_POINT('Ctrl Pts',(6.56428366991149,1.64391876348358,22.775288873078));
#14260=CARTESIAN_POINT('Ctrl Pts',(6.5190983786768,1.82434682109849,22.7840380431888));
#14261=CARTESIAN_POINT('Ctrl Pts',(6.46646995271881,2.00291071820576,22.7927872132996));
#14262=CARTESIAN_POINT('Ctrl Pts',(6.40657713281505,2.17900400212832,22.8015363834105));
#14263=CARTESIAN_POINT('Ctrl Pts',(6.34668509279012,2.35509499309786,22.8102854395962));
#14264=CARTESIAN_POINT('Ctrl Pts',(6.27952894037475,2.52871516398249,22.819034495782));
#14265=CARTESIAN_POINT('Ctrl Pts',(6.20533675061392,2.69927486771545,22.8277835519678));
#14266=CARTESIAN_POINT('Ctrl Pts',(6.12832117907861,2.87632521636041,22.83686555325));
#14267=CARTESIAN_POINT('Ctrl Pts',(6.04372366626024,3.05007728920107,22.8459475545323));
#14268=CARTESIAN_POINT('Ctrl Pts',(5.95185378007813,3.21989527478298,22.8550295558146));
#14269=CARTESIAN_POINT('Ctrl Pts',(5.86334450817313,3.38350129286852,22.8637793361217));
#14270=CARTESIAN_POINT('Ctrl Pts',(5.76808562057195,3.5434556712506,22.8725291164288));
#14271=CARTESIAN_POINT('Ctrl Pts',(5.66640068804421,3.69921508465406,22.8812788967359));
#14272=CARTESIAN_POINT('Ctrl Pts',(5.56471941107855,3.85496889852381,22.8900283624894));
#14273=CARTESIAN_POINT('Ctrl Pts',(5.45661270815041,4.00652780919736,22.8987778282429));
#14274=CARTESIAN_POINT('Ctrl Pts',(5.34244776449036,4.1533770456933,22.9075272939964));
#14275=CARTESIAN_POINT('Ctrl Pts',(5.22828631819518,4.30022178356343,22.916276491716));
#14276=CARTESIAN_POINT('Ctrl Pts',(5.10806717843994,4.44235690972765,22.9250256894356));
#14277=CARTESIAN_POINT('Ctrl Pts',(4.98219864544646,4.57929969070724,22.9337748871552));
#14278=CARTESIAN_POINT('Ctrl Pts',(4.8563332994395,4.71623900430078,22.9425238633454));
#14279=CARTESIAN_POINT('Ctrl Pts',(4.72481904033572,4.84798602483691,22.9512728395357));
#14280=CARTESIAN_POINT('Ctrl Pts',(4.5881025073712,4.97409332259198,22.9600218157259));
#14281=CARTESIAN_POINT('Ctrl Pts',(4.45137708685563,5.10020881822204,22.9687713606621));
#14282=CARTESIAN_POINT('Ctrl Pts',(4.30944892635971,5.22068366307999,22.9775209055982));
#14283=CARTESIAN_POINT('Ctrl Pts',(4.1628000946658,5.33510865604914,22.9862704505344));
#14284=CARTESIAN_POINT('Ctrl Pts',(4.01615988348696,5.4495269227296,22.9950194811427));
#14285=CARTESIAN_POINT('Ctrl Pts',(3.86479978232127,5.55789587288699,23.003768511751));
#14286=CARTESIAN_POINT('Ctrl Pts',(3.70923383580952,5.65984746713954,23.0125175423593));
#14287=CARTESIAN_POINT('Ctrl Pts',(3.55366577799422,5.76180044505456,23.0212666917073));
#14288=CARTESIAN_POINT('Ctrl Pts',(3.39389200026719,5.85733573571129,23.0300158410553));
#14289=CARTESIAN_POINT('Ctrl Pts',(3.23045513625917,5.94612887621995,23.0387649904033));
#14290=CARTESIAN_POINT('Ctrl Pts',(3.18695122151495,5.96976399206732,23.0410938545163));
#14291=CARTESIAN_POINT('Ctrl Pts',(3.14318791262623,5.99292165435354,23.0434227186292));
#14292=CARTESIAN_POINT('Ctrl Pts',(3.09917575053259,6.01559628526639,23.0457515827422));
#14293=CARTESIAN_POINT('Ctrl Pts',(3.09917575053256,6.01559628526641,21.0459192328109));
#14294=CARTESIAN_POINT('Ctrl Pts',(2.94414160813452,6.09546834313728,21.0541282552626));
#14295=CARTESIAN_POINT('Ctrl Pts',(2.78588209296763,6.16941313824782,21.0623372777142));
#14296=CARTESIAN_POINT('Ctrl Pts',(2.62489110093943,6.23716567907323,21.0705463001659));
#14297=CARTESIAN_POINT('Ctrl Pts',(2.46400520838181,6.30487398912472,21.0787499635357));
#14298=CARTESIAN_POINT('Ctrl Pts',(2.30039172030012,6.36639795900436,21.0869536269055));
#14299=CARTESIAN_POINT('Ctrl Pts',(2.1345674974083,6.42151933727588,21.0951572902753));
#14300=CARTESIAN_POINT('Ctrl Pts',(1.96416434180923,6.47816279161949,21.1035874828087));
#14301=CARTESIAN_POINT('Ctrl Pts',(1.7914269459188,6.52804479075767,21.1120176753421));
#14302=CARTESIAN_POINT('Ctrl Pts',(1.61693712927694,6.57098191444518,21.1204478678755));
#14303=CARTESIAN_POINT('Ctrl Pts',(1.44723353533284,6.61274128094362,21.1286468218208));
#14304=CARTESIAN_POINT('Ctrl Pts',(1.27587276456234,6.64793167648423,21.136845775766));
#14305=CARTESIAN_POINT('Ctrl Pts',(1.10340412986792,6.67643530083161,21.1450447297113));
#14306=CARTESIAN_POINT('Ctrl Pts',(0.930936761704805,6.70493871586132,21.1532436234472));
#14307=CARTESIAN_POINT('Ctrl Pts',(0.757361899396523,6.72675539869723,21.161442517183));
#14308=CARTESIAN_POINT('Ctrl Pts',(0.583237434654319,6.74181897523345,21.1696414109189));
#14309=CARTESIAN_POINT('Ctrl Pts',(0.409082661621966,6.75688517375188,21.1778417317629));
#14310=CARTESIAN_POINT('Ctrl Pts',(0.234378452688174,6.76519589389805,21.186042052607));
#14311=CARTESIAN_POINT('Ctrl Pts',(0.0596862445282713,6.76673677278894,
21.194242373451));
#14312=CARTESIAN_POINT('Ctrl Pts',(-0.123590555858885,6.76835337238363,
21.2028456682532));
#14313=CARTESIAN_POINT('Ctrl Pts',(-0.306853703567373,6.7625179702011,21.2114489630554));
#14314=CARTESIAN_POINT('Ctrl Pts',(-0.489457457335657,6.74927554612038,
21.2200522578576));
#14315=CARTESIAN_POINT('Ctrl Pts',(-0.663747179090622,6.73663605563477,
21.2282638407321));
#14316=CARTESIAN_POINT('Ctrl Pts',(-0.837435867117087,6.71724916567306,
21.2364754236065));
#14317=CARTESIAN_POINT('Ctrl Pts',(-1.00996988088243,6.6912069045659,21.2446870064809));
#14318=CARTESIAN_POINT('Ctrl Pts',(-1.18260814332675,6.66514890817699,21.2529035509664));
#14319=CARTESIAN_POINT('Ctrl Pts',(-1.35408998981319,6.63242759211696,21.2611200954519));
#14320=CARTESIAN_POINT('Ctrl Pts',(-1.52387379075133,6.59318569963422,21.2693366399373));
#14321=CARTESIAN_POINT('Ctrl Pts',(-1.69385881556009,6.55389729855966,21.2775629224831));
#14322=CARTESIAN_POINT('Ctrl Pts',(-1.86214143251141,6.5080729857557,21.2857892050288));
#14323=CARTESIAN_POINT('Ctrl Pts',(-2.02819624516931,6.45590497072882,21.2940154875745));
#14324=CARTESIAN_POINT('Ctrl Pts',(-2.05152052326467,6.44857738250242,21.2951709620755));
#14325=CARTESIAN_POINT('Ctrl Pts',(-2.07480088212925,6.44112471379489,21.2963264365764));
#14326=CARTESIAN_POINT('Ctrl Pts',(-2.0980359002287,6.43354757201278,21.2974819110774));
#14327=CARTESIAN_POINT('Ctrl Pts',(-2.27188951211167,6.37685239489128,21.3061276291298));
#14328=CARTESIAN_POINT('Ctrl Pts',(-2.44359915957589,6.31305534389745,21.3147733471822));
#14329=CARTESIAN_POINT('Ctrl Pts',(-2.61257843726977,6.24233313025771,21.3234190652346));
#14330=CARTESIAN_POINT('Ctrl Pts',(-2.78134078000741,6.1717017095278,21.3320536839469));
#14331=CARTESIAN_POINT('Ctrl Pts',(-2.94737946261302,6.09416297144666,21.3406883026592));
#14332=CARTESIAN_POINT('Ctrl Pts',(-3.11012465662858,6.00994289658654,21.3493229213716));
#14333=CARTESIAN_POINT('Ctrl Pts',(-3.27861737868219,5.92274849585121,21.358262481274));
#14334=CARTESIAN_POINT('Ctrl Pts',(-3.4435794258418,5.82839229969718,21.3672020411764));
#14335=CARTESIAN_POINT('Ctrl Pts',(-3.60439967688412,5.72718010623707,21.3761416010789));
#14336=CARTESIAN_POINT('Ctrl Pts',(-3.75930298708128,5.62969173833768,21.3847522543493));
#14337=CARTESIAN_POINT('Ctrl Pts',(-3.91036351788745,5.52584301566804,21.3933629076198));
#14338=CARTESIAN_POINT('Ctrl Pts',(-4.05705853589733,5.41595467450593,21.4019735608903));
#14339=CARTESIAN_POINT('Ctrl Pts',(-4.20361469726065,5.30617035000885,21.4105760636014));
#14340=CARTESIAN_POINT('Ctrl Pts',(-4.34581334112871,5.19035798723764,21.4191785663126));
#14341=CARTESIAN_POINT('Ctrl Pts',(-4.48316026112377,5.06888183656718,21.4277810690238));
#14342=CARTESIAN_POINT('Ctrl Pts',(-4.62035259992436,4.9475424048597,21.4363738897913));
#14343=CARTESIAN_POINT('Ctrl Pts',(-4.75270388045081,4.82055210377769,21.4449667105589));
#14344=CARTESIAN_POINT('Ctrl Pts',(-4.87975241417786,4.68831583581198,21.4535595313264));
#14345=CARTESIAN_POINT('Ctrl Pts',(-4.89472566096314,4.67273119098272,21.4545722342845));
#14346=CARTESIAN_POINT('Ctrl Pts',(-4.90962529197411,4.65707372729123,21.4555849372427));
#14347=CARTESIAN_POINT('Ctrl Pts',(-4.92445058217966,4.64134414406758,21.4565976402008));
#14348=CARTESIAN_POINT('Ctrl Pts',(-5.05027937497575,4.50784021660474,21.4651928979609));
#14349=CARTESIAN_POINT('Ctrl Pts',(-5.1706018550547,4.36929508541175,21.473788155721));
#14350=CARTESIAN_POINT('Ctrl Pts',(-5.28503583096103,4.22619039626211,21.482383413481));
#14351=CARTESIAN_POINT('Ctrl Pts',(-5.39957696943315,4.08295169563952,21.4909867203355));
#14352=CARTESIAN_POINT('Ctrl Pts',(-5.50821840620999,3.9351451527872,21.49959002719));
#14353=CARTESIAN_POINT('Ctrl Pts',(-5.61062040097536,3.78328266405764,21.5081933340445));
#14354=CARTESIAN_POINT('Ctrl Pts',(-5.71726801795294,3.62512390388505,21.5171533369844));
#14355=CARTESIAN_POINT('Ctrl Pts',(-5.81714758748002,3.46256603293383,21.5261133399244));
#14356=CARTESIAN_POINT('Ctrl Pts',(-5.90992806957095,3.29621589288345,21.5350733428644));
#14357=CARTESIAN_POINT('Ctrl Pts',(-5.9992586955561,3.13605114908684,21.5437001860691));
#14358=CARTESIAN_POINT('Ctrl Pts',(-6.0820085529776,2.97237135173396,21.5523270292738));
#14359=CARTESIAN_POINT('Ctrl Pts',(-6.15793115642692,2.80573927382902,21.5609538724786));
#14360=CARTESIAN_POINT('Ctrl Pts',(-6.23392632269387,2.63894793777788,21.5695889607647));
#14361=CARTESIAN_POINT('Ctrl Pts',(-6.30308109241908,2.46919897007563,21.5782240490509));
#14362=CARTESIAN_POINT('Ctrl Pts',(-6.36519788937159,2.29707310052151,21.5868591373371));
#14363=CARTESIAN_POINT('Ctrl Pts',(-6.4274069422329,2.12469158950962,21.5955070504622));
#14364=CARTESIAN_POINT('Ctrl Pts',(-6.4825570380835,1.94992641162066,21.6041549635874));
#14365=CARTESIAN_POINT('Ctrl Pts',(-6.53050058744835,1.77337279705559,21.6128028767125));
#14366=CARTESIAN_POINT('Ctrl Pts',(-6.53587912383372,1.75356616920917,21.6137730409164));
#14367=CARTESIAN_POINT('Ctrl Pts',(-6.54116701590315,1.73373704265969,21.6147432051203));
#14368=CARTESIAN_POINT('Ctrl Pts',(-6.54636409560635,1.71388626453336,21.6157133693242));
#14369=CARTESIAN_POINT('Ctrl Pts',(-6.60118239460743,1.50450215790442,21.6259465684371));
#14370=CARTESIAN_POINT('Ctrl Pts',(-6.64597801593179,1.29238336355856,21.6361797675501));
#14371=CARTESIAN_POINT('Ctrl Pts',(-6.68052239666622,1.07838282054242,21.646412966663));
#14372=CARTESIAN_POINT('Ctrl Pts',(-6.71463017949775,0.867086977576364,
21.6565168308979));
#14373=CARTESIAN_POINT('Ctrl Pts',(-6.73874421554605,0.653956575821893,
21.6666206951327));
#14374=CARTESIAN_POINT('Ctrl Pts',(-6.75269107268225,0.439832100826509,
21.6767245593675));
#14375=CARTESIAN_POINT('Ctrl Pts',(-6.76210285436492,0.29533411164576,21.683542967515));
#14376=CARTESIAN_POINT('Ctrl Pts',(-6.76688547413455,0.150383825806707,
21.6903613756625));
#14377=CARTESIAN_POINT('Ctrl Pts',(-6.76699796740266,0.0052449183330411,
21.69717978381));
#14378=CARTESIAN_POINT('',(-6.76699964607789,0.00218860269287247,21.3028202162152));
#14379=CARTESIAN_POINT('Ctrl Pts',(3.09917575053258,6.01559628526639,20.6513153324719));
#14380=CARTESIAN_POINT('Ctrl Pts',(3.06227820682817,6.03460553510302,20.6532782421475));
#14381=CARTESIAN_POINT('Ctrl Pts',(3.02521909496846,6.053268428723,20.6552411518232));
#14382=CARTESIAN_POINT('Ctrl Pts',(2.9880055900179,6.07158229739347,20.6572040614988));
#14383=CARTESIAN_POINT('Ctrl Pts',(2.83205033354915,6.14833250109595,20.6654302708357));
#14384=CARTESIAN_POINT('Ctrl Pts',(2.67291804970943,6.21917730927014,20.6736564801727));
#14385=CARTESIAN_POINT('Ctrl Pts',(2.51109534433012,6.28384350311842,20.6818826895097));
#14386=CARTESIAN_POINT('Ctrl Pts',(2.34945443982791,6.34843704726817,20.6900996570529));
#14387=CARTESIAN_POINT('Ctrl Pts',(2.18512946255633,6.40686566744847,20.6983166245961));
#14388=CARTESIAN_POINT('Ctrl Pts',(2.01863125158421,6.458902141241,20.7065335921393));
#14389=CARTESIAN_POINT('Ctrl Pts',(1.85228667669486,6.51089059842153,20.7147429774827));
#14390=CARTESIAN_POINT('Ctrl Pts',(1.68377320198984,6.55649854968249,20.722952362826));
#14391=CARTESIAN_POINT('Ctrl Pts',(1.51362135453083,6.59554693676789,20.7311617481694));
#14392=CARTESIAN_POINT('Ctrl Pts',(1.34359237466644,6.63456712679597,20.73936520547));
#14393=CARTESIAN_POINT('Ctrl Pts',(1.17192772666979,6.66703710744346,20.7475686627706));
#14394=CARTESIAN_POINT('Ctrl Pts',(0.999172888189012,6.69282769384571,20.7557721200712));
#14395=CARTESIAN_POINT('Ctrl Pts',(0.826508142741077,6.71860483025044,20.763971299203));
#14396=CARTESIAN_POINT('Ctrl Pts',(0.652754693309591,6.73770945905045,20.7721704783349));
#14397=CARTESIAN_POINT('Ctrl Pts',(0.478468085048685,6.75006350278202,20.7803696574667));
#14398=CARTESIAN_POINT('Ctrl Pts',(0.304214316140977,6.7624152187455,20.7885672916965));
#14399=CARTESIAN_POINT('Ctrl Pts',(0.129427945436976,6.76801885170962,20.7967649259264));
#14400=CARTESIAN_POINT('Ctrl Pts',(-0.0453301721559057,6.76684817145267,
20.8049625601562));
#14401=CARTESIAN_POINT('Ctrl Pts',(-0.220075675516464,6.7656775756967,20.8131596026718));
#14402=CARTESIAN_POINT('Ctrl Pts',(-0.394792571151051,6.75773364206391,
20.8213566451873));
#14403=CARTESIAN_POINT('Ctrl Pts',(-0.568919867081917,6.74304227962716,
20.8295536877029));
#14404=CARTESIAN_POINT('Ctrl Pts',(-0.743066241658224,6.72834930749853,
20.8377516283458));
#14405=CARTESIAN_POINT('Ctrl Pts',(-0.916622530342755,6.7069074638335,20.8459495689886));
#14406=CARTESIAN_POINT('Ctrl Pts',(-1.08903267064767,6.67879456505903,20.8541475096314));
#14407=CARTESIAN_POINT('Ctrl Pts',(-1.2614930368245,6.6506734765409,20.8623478384674));
#14408=CARTESIAN_POINT('Ctrl Pts',(-1.43280623563417,6.61587751963145,20.8705481673034));
#14409=CARTESIAN_POINT('Ctrl Pts',(-1.60242615208156,6.57453568148543,20.8787484961394));
#14410=CARTESIAN_POINT('Ctrl Pts',(-1.7722228168832,6.53315076407132,20.8869573699308));
#14411=CARTESIAN_POINT('Ctrl Pts',(-1.94032232529138,6.48520642318485,20.8951662437222));
#14412=CARTESIAN_POINT('Ctrl Pts',(-2.1061925268366,6.43088190218866,20.9033751175136));
#14413=CARTESIAN_POINT('Ctrl Pts',(-2.27215174908918,6.37652822582135,20.911588396917));
#14414=CARTESIAN_POINT('Ctrl Pts',(-2.43587894336696,6.31578766777315,20.9198016763204));
#14415=CARTESIAN_POINT('Ctrl Pts',(-2.59686182271381,6.24888771492427,20.9280149557239));
#14416=CARTESIAN_POINT('Ctrl Pts',(-2.75808016482367,6.18188991037957,20.9362402483393));
#14417=CARTESIAN_POINT('Ctrl Pts',(-2.9165458446842,6.10871485732904,20.9444655409547));
#14418=CARTESIAN_POINT('Ctrl Pts',(-3.07176992376616,6.02963668353622,20.9526908335702));
#14419=CARTESIAN_POINT('Ctrl Pts',(-3.21215145709171,5.95811997456119,20.9601296226823));
#14420=CARTESIAN_POINT('Ctrl Pts',(-3.34988184633226,5.88177577113918,20.9675684117943));
#14421=CARTESIAN_POINT('Ctrl Pts',(-3.48462051066236,5.80083691346957,20.9750072009064));
#14422=CARTESIAN_POINT('Ctrl Pts',(-3.63362155385508,5.7113305027629,20.9832334019253));
#14423=CARTESIAN_POINT('Ctrl Pts',(-3.77938003164929,5.61595440977538,20.9914596029441));
#14424=CARTESIAN_POINT('Ctrl Pts',(-3.92140267518536,5.51496963355639,20.999685803963));
#14425=CARTESIAN_POINT('Ctrl Pts',(-4.06326578621417,5.41409829244989,21.0079027645787));
#14426=CARTESIAN_POINT('Ctrl Pts',(-4.20140112957516,5.30763101940892,21.0161197251945));
#14427=CARTESIAN_POINT('Ctrl Pts',(-4.33534097028699,5.19587410079874,21.0243366858102));
#14428=CARTESIAN_POINT('Ctrl Pts',(-4.46915724060706,5.08422028703131,21.0325460656118));
#14429=CARTESIAN_POINT('Ctrl Pts',(-4.59878544326628,4.96728677497224,21.0407554454134));
#14430=CARTESIAN_POINT('Ctrl Pts',(-4.72378766162664,4.84542249219446,21.048964825215));
#14431=CARTESIAN_POINT('Ctrl Pts',(-4.84869963616683,4.72364618784269,21.0571682783554));
#14432=CARTESIAN_POINT('Ctrl Pts',(-4.96899202270647,4.59694645243934,21.0653717314959));
#14433=CARTESIAN_POINT('Ctrl Pts',(-5.08426072608249,4.46571179871868,21.0735751846363));
#14434=CARTESIAN_POINT('Ctrl Pts',(-5.19946933524446,4.33454556290452,21.0817743609864));
#14435=CARTESIAN_POINT('Ctrl Pts',(-5.30965924274331,4.19884938756544,21.0899735373366));
#14436=CARTESIAN_POINT('Ctrl Pts',(-5.41446385749655,4.0590479346595,21.0981727136867));
#14437=CARTESIAN_POINT('Ctrl Pts',(-5.5192487516799,3.91927278750669,21.1063703472381));
#14438=CARTESIAN_POINT('Ctrl Pts',(-5.61865015167468,3.7753941843924,21.1145679807895));
#14439=CARTESIAN_POINT('Ctrl Pts',(-5.71234216973286,3.62786933831577,21.1227656143408));
#14440=CARTESIAN_POINT('Ctrl Pts',(-5.8060274396663,3.48035511764871,21.1309626574614));
#14441=CARTESIAN_POINT('Ctrl Pts',(-5.89400395358346,3.32919547934301,21.139159700582));
#14442=CARTESIAN_POINT('Ctrl Pts',(-5.97598957491879,3.17487599765125,21.1473567437026));
#14443=CARTESIAN_POINT('Ctrl Pts',(-6.05798419202711,3.02053958344127,21.1555546862338));
#14444=CARTESIAN_POINT('Ctrl Pts',(-6.13398643861804,2.8630429519176,21.163752628765));
#14445=CARTESIAN_POINT('Ctrl Pts',(-6.20376047911267,2.70289565425669,21.1719505712962));
#14446=CARTESIAN_POINT('Ctrl Pts',(-6.27355485684178,2.54270167801562,21.1801509033046));
#14447=CARTESIAN_POINT('Ctrl Pts',(-6.33711726928226,2.37985582546049,21.188351235313));
#14448=CARTESIAN_POINT('Ctrl Pts',(-6.39426028112862,2.21488700776833,21.1965515673214));
#14449=CARTESIAN_POINT('Ctrl Pts',(-6.451462851438,2.04974624798018,21.2047604462921));
#14450=CARTESIAN_POINT('Ctrl Pts',(-6.50223253649237,1.88247844177856,21.2129693252629));
#14451=CARTESIAN_POINT('Ctrl Pts',(-6.54643170871449,1.7136279885487,21.2211782042337));
#14452=CARTESIAN_POINT('Ctrl Pts',(-6.59065460807742,1.5446868924792,21.229391489921));
#14453=CARTESIAN_POINT('Ctrl Pts',(-6.62829988576043,1.37416180557822,21.2376047756084));
#14454=CARTESIAN_POINT('Ctrl Pts',(-6.6592812259374,1.20260656653692,21.2458180612958));
#14455=CARTESIAN_POINT('Ctrl Pts',(-6.69030788799672,1.03080036332443,21.2540433620079));
#14456=CARTESIAN_POINT('Ctrl Pts',(-6.71465108074954,0.857961351510397,
21.26226866272));
#14457=CARTESIAN_POINT('Ctrl Pts',(-6.73227634093087,0.684649011788133,
21.2704939634321));
#14458=CARTESIAN_POINT('Ctrl Pts',(-6.74821626266822,0.52790890679864,21.2779327557261));
#14459=CARTESIAN_POINT('Ctrl Pts',(-6.75866224229275,0.37078189373866,21.2853715480201));
#14460=CARTESIAN_POINT('Ctrl Pts',(-6.76362548441819,0.213680384052582,
21.2928103403141));
#14461=CARTESIAN_POINT('Ctrl Pts',(-6.76585171665472,0.143213452069029,
21.2961469656061));
#14462=CARTESIAN_POINT('Ctrl Pts',(-6.76697683831429,0.0727085243909415,
21.299483590898));
#14463=CARTESIAN_POINT('Ctrl Pts',(-6.76699964607772,0.00218860322720043,
21.3028202161899));
#14464=CARTESIAN_POINT('Ctrl Pts',(-6.76699964607789,0.00218860269286346,
21.3028202162152));
#14465=CARTESIAN_POINT('Ctrl Pts',(-6.7670550866106,-0.169229474448601,
21.3109308023056));
#14466=CARTESIAN_POINT('Ctrl Pts',(-6.76059291480052,-0.340926580401995,
21.3190413883959));
#14467=CARTESIAN_POINT('Ctrl Pts',(-6.74757566434377,-0.512358911268055,
21.3271519744863));
#14468=CARTESIAN_POINT('Ctrl Pts',(-6.73457327164884,-0.683595570955248,
21.3352533032334));
#14469=CARTESIAN_POINT('Ctrl Pts',(-6.71503071894525,-0.854567692450595,
21.3433546319804));
#14470=CARTESIAN_POINT('Ctrl Pts',(-6.68896247809689,-1.0247292162381,21.3514559607275));
#14471=CARTESIAN_POINT('Ctrl Pts',(-6.66291838775061,-1.19473309662122,
21.3595497841289));
#14472=CARTESIAN_POINT('Ctrl Pts',(-6.63036069895213,-1.36392751142699,
21.3676436075304));
#14473=CARTESIAN_POINT('Ctrl Pts',(-6.59135583382869,-1.53176932723321,
21.3757374309319));
#14474=CARTESIAN_POINT('Ctrl Pts',(-6.55237872664589,-1.69949169785882,
21.3838254943373));
#14475=CARTESIAN_POINT('Ctrl Pts',(-6.50696366088859,-1.86586302745634,
21.3919135577427));
#14476=CARTESIAN_POINT('Ctrl Pts',(-6.45522849449401,-2.03034826664605,
21.4000016211481));
#14477=CARTESIAN_POINT('Ctrl Pts',(-6.40351904004577,-2.19475175804333,
21.4080856648534));
#14478=CARTESIAN_POINT('Ctrl Pts',(-6.34549585029914,-2.35727067388517,
21.4161697085587));
#14479=CARTESIAN_POINT('Ctrl Pts',(-6.28132718315745,-2.51738312899076,
21.4242537522641));
#14480=CARTESIAN_POINT('Ctrl Pts',(-6.217166373681,-2.67747597779737,21.4323368060515));
#14481=CARTESIAN_POINT('Ctrl Pts',(-6.14686171446634,-2.83516260657845,
21.440419859839));
#14482=CARTESIAN_POINT('Ctrl Pts',(-6.07063042492687,-2.98993900338321,
21.4485029136265));
#14483=CARTESIAN_POINT('Ctrl Pts',(-5.99440076094549,-3.14471209973189,
21.4565857950507));
#14484=CARTESIAN_POINT('Ctrl Pts',(-5.91224488069568,-3.29657475551216,
21.4646686764749));
#14485=CARTESIAN_POINT('Ctrl Pts',(-5.82442688351885,-3.44504578758293,
21.4727515578991));
#14486=CARTESIAN_POINT('Ctrl Pts',(-5.73659368802381,-3.59354251495607,
21.4808358381961));
#14487=CARTESIAN_POINT('Ctrl Pts',(-5.64309661274925,-3.738646131684,21.4889201184931));
#14488=CARTESIAN_POINT('Ctrl Pts',(-5.54424411578657,-3.87990285761977,
21.49700439879));
#14489=CARTESIAN_POINT('Ctrl Pts',(-5.44535529199878,-4.02121149330526,
21.50509164994));
#14490=CARTESIAN_POINT('Ctrl Pts',(-5.34110734030057,-4.15867012116083,
21.51317890109));
#14491=CARTESIAN_POINT('Ctrl Pts',(-5.23185009928415,-4.29185665401589,
21.5212661522399));
#14492=CARTESIAN_POINT('Ctrl Pts',(-5.12246746645082,-4.42519604174067,
21.5293626849268));
#14493=CARTESIAN_POINT('Ctrl Pts',(-5.00806429764822,-4.55425325694381,
21.5374592176137));
#14494=CARTESIAN_POINT('Ctrl Pts',(-4.88902910078328,-4.67864119715267,
21.5455557503006));
#14495=CARTESIAN_POINT('Ctrl Pts',(-4.76991955132648,-4.80310683342115,
21.5536573402999));
#14496=CARTESIAN_POINT('Ctrl Pts',(-4.64617247530951,-4.92289712879588,
21.5617589302993));
#14497=CARTESIAN_POINT('Ctrl Pts',(-4.51821047574782,-5.03766444861532,
21.5698605202987));
#14498=CARTESIAN_POINT('Ctrl Pts',(-4.39005486302091,-5.1526054173628,21.5779743684254));
#14499=CARTESIAN_POINT('Ctrl Pts',(-4.2576718730724,-5.26250799626261,21.5860882165521));
#14500=CARTESIAN_POINT('Ctrl Pts',(-4.12151497908504,-5.36706654301748,
21.5942020646789));
#14501=CARTESIAN_POINT('Ctrl Pts',(-4.02971606676951,-5.43756140070924,
21.5996725363598));
#14502=CARTESIAN_POINT('Ctrl Pts',(-3.93620226711389,-5.50562795751845,
21.6051430080408));
#14503=CARTESIAN_POINT('Ctrl Pts',(-3.84111885571986,-5.57118433874103,
21.6106134797217));
#14504=CARTESIAN_POINT('Ctrl Pts',(-3.69801849100092,-5.66984657566614,
21.6188465298537));
#14505=CARTESIAN_POINT('Ctrl Pts',(-3.55090515941149,-5.76313603609576,
21.6270795799858));
#14506=CARTESIAN_POINT('Ctrl Pts',(-3.40021895058611,-5.85070936622861,
21.6353126301178));
#14507=CARTESIAN_POINT('Ctrl Pts',(-3.24971218587267,-5.93817840998661,
21.6435358759526));
#14508=CARTESIAN_POINT('Ctrl Pts',(-3.09564132282225,-6.01994469972233,
21.6517591217875));
#14509=CARTESIAN_POINT('Ctrl Pts',(-2.93847736012107,-6.09570666978456,
21.6599823676223));
#14510=CARTESIAN_POINT('Ctrl Pts',(-2.78146909883463,-6.17139358290803,
21.6681974667358));
#14511=CARTESIAN_POINT('Ctrl Pts',(-2.62137416095189,-6.24108786829145,
21.6764125658494));
#14512=CARTESIAN_POINT('Ctrl Pts',(-2.45869029514056,-6.30453257843764,
21.6846276649629));
#14513=CARTESIAN_POINT('Ctrl Pts',(-2.29613504951535,-6.36792712829053,
21.6928362691018));
#14514=CARTESIAN_POINT('Ctrl Pts',(-2.1309952850655,-6.42508181484139,21.7010448732407));
#14515=CARTESIAN_POINT('Ctrl Pts',(-1.96379108229923,-6.47578671553364,
21.7092534773796));
#14516=CARTESIAN_POINT('Ctrl Pts',(-1.79668562806048,-6.52646167060134,
21.7174572336285));
#14517=CARTESIAN_POINT('Ctrl Pts',(-1.62751850622446,-6.57069432450043,
21.7256609898775));
#14518=CARTESIAN_POINT('Ctrl Pts',(-1.45682749523002,-6.60832373973475,
21.7338647461265));
#14519=CARTESIAN_POINT('Ctrl Pts',(-1.28618698740327,-6.6459420213736,21.7420660750907));
#14520=CARTESIAN_POINT('Ctrl Pts',(-1.11402383706335,-6.67696087532799,
21.750267404055));
#14521=CARTESIAN_POINT('Ctrl Pts',(-0.940888873299894,-6.70126981460234,
21.7584687330193));
#14522=CARTESIAN_POINT('Ctrl Pts',(-0.767777786500949,-6.72557540144188,
21.766668930942));
#14523=CARTESIAN_POINT('Ctrl Pts',(-0.593695507772916,-6.7431728660062,
21.7748691288647));
#14524=CARTESIAN_POINT('Ctrl Pts',(-0.419200923101633,-6.75400322668495,
21.7830693267874));
#14525=CARTESIAN_POINT('Ctrl Pts',(-0.244698780930254,-6.76483405643529,
21.7912698798672));
#14526=CARTESIAN_POINT('Ctrl Pts',(-0.069784654852228,-6.76889717613982,
21.7994704329471));
#14527=CARTESIAN_POINT('Ctrl Pts',(0.104979548719595,-6.76618565325772,
21.8076709860269));
#14528=CARTESIAN_POINT('Ctrl Pts',(0.279782992165525,-6.76347352155635,
21.8158733803801));
#14529=CARTESIAN_POINT('Ctrl Pts',(0.454436087892108,-6.75398372319741,
21.8240757747333));
#14530=CARTESIAN_POINT('Ctrl Pts',(0.628378974667604,-6.7377614134218,21.8322781690865));
#14531=CARTESIAN_POINT('Ctrl Pts',(0.802484528620172,-6.72152393293478,
21.8404882341204));
#14532=CARTESIAN_POINT('Ctrl Pts',(0.975878189466887,-6.69854139529803,
21.8486982991542));
#14533=CARTESIAN_POINT('Ctrl Pts',(1.14800630951264,-6.66891074414099,21.856908364188));
#14534=CARTESIAN_POINT('Ctrl Pts',(1.32021680702311,-6.63926591227996,21.8651223584133));
#14535=CARTESIAN_POINT('Ctrl Pts',(1.4911602058588,-6.60296669755028,21.8733363526387));
#14536=CARTESIAN_POINT('Ctrl Pts',(1.66029512134809,-6.56016075336784,21.881550346864));
#14537=CARTESIAN_POINT('Ctrl Pts',(1.82966062405915,-6.51729645042657,21.8897755394992));
#14538=CARTESIAN_POINT('Ctrl Pts',(1.99721237219837,-6.46790779087146,21.8980007321344));
#14539=CARTESIAN_POINT('Ctrl Pts',(2.16242499113894,-6.41219207117954,21.9062259247695));
#14540=CARTESIAN_POINT('Ctrl Pts',(2.3110003454966,-6.36208704379361,21.9136228228895));
#14541=CARTESIAN_POINT('Ctrl Pts',(2.4576840380658,-6.30686581396072,21.9210197210094));
#14542=CARTESIAN_POINT('Ctrl Pts',(2.60210982344173,-6.24670420836044,21.9284166191294));
#14543=CARTESIAN_POINT('Ctrl Pts',(2.77092389665618,-6.17638348504868,21.9370625856203));
#14544=CARTESIAN_POINT('Ctrl Pts',(2.93703609492105,-6.0991529668233,21.9457085521112));
#14545=CARTESIAN_POINT('Ctrl Pts',(3.09987589074755,-6.01523552838641,21.9543545186021));
#14546=CARTESIAN_POINT('Ctrl Pts',(3.26250739233755,-5.93142543176162,21.9629894257264));
#14547=CARTESIAN_POINT('Ctrl Pts',(3.421874568541,-5.8409456100945,21.9716243328508));
#14548=CARTESIAN_POINT('Ctrl Pts',(3.57742734294272,-5.74406673063308,21.9802592399751));
#14549=CARTESIAN_POINT('Ctrl Pts',(3.7381443439053,-5.64397155056613,21.9891808190466));
#14550=CARTESIAN_POINT('Ctrl Pts',(3.89478901331375,-5.53704522027752,21.9981023981181));
#14551=CARTESIAN_POINT('Ctrl Pts',(4.04678002526133,-5.4236390391642,22.0070239771897));
#14552=CARTESIAN_POINT('Ctrl Pts',(4.19348091275735,-5.31418001784657,22.0156350361653));
#14553=CARTESIAN_POINT('Ctrl Pts',(4.33584632806746,-5.19868478645936,22.024246095141));
#14554=CARTESIAN_POINT('Ctrl Pts',(4.47338062319848,-5.07751462824012,22.0328571541167));
#14555=CARTESIAN_POINT('Ctrl Pts',(4.61078521713796,-4.95645873907563,22.0414600924662));
#14556=CARTESIAN_POINT('Ctrl Pts',(4.74336754624104,-4.8297387939334,22.0500630308156));
#14557=CARTESIAN_POINT('Ctrl Pts',(4.8706638592181,-4.69775718513703,22.058665969165));
#14558=CARTESIAN_POINT('Ctrl Pts',(4.99781762977369,-4.56592336520955,22.0672592742137));
#14559=CARTESIAN_POINT('Ctrl Pts',(5.11969698141735,-4.42883985472765,22.0758525792624));
#14560=CARTESIAN_POINT('Ctrl Pts',(5.23587380683145,-4.28694698811827,22.0844458843111));
#14561=CARTESIAN_POINT('Ctrl Pts',(5.24881780680619,-4.27113780022508,22.0854033191518));
#14562=CARTESIAN_POINT('Ctrl Pts',(5.26169105482427,-4.25526894923221,22.0863607539925));
#14563=CARTESIAN_POINT('Ctrl Pts',(5.27449298695413,-4.23934107268708,22.0873181888332));
#14564=CARTESIAN_POINT('Ctrl Pts',(5.38942749743028,-4.09634213509955,22.0959139463808));
#14565=CARTESIAN_POINT('Ctrl Pts',(5.49847583092701,-3.94875035898457,22.1045097039283));
#14566=CARTESIAN_POINT('Ctrl Pts',(5.60129477837398,-3.79707595469993,22.1131054614759));
#14567=CARTESIAN_POINT('Ctrl Pts',(5.70420965939407,-3.64526003304019,22.1217092391574));
#14568=CARTESIAN_POINT('Ctrl Pts',(5.80088338163245,-3.48935413255895,22.1303130168389));
#14569=CARTESIAN_POINT('Ctrl Pts',(5.89101743056434,-3.32989528856196,22.1389167945205));
#14570=CARTESIAN_POINT('Ctrl Pts',(5.9846938264375,-3.16416957255617,22.1478587081885));
#14571=CARTESIAN_POINT('Ctrl Pts',(6.07130595035719,-2.99460633227664,22.1568006218566));
#14572=CARTESIAN_POINT('Ctrl Pts',(6.15057310451502,-2.82183264670613,22.1657425355246));
#14573=CARTESIAN_POINT('Ctrl Pts',(6.22705044510308,-2.65513974424968,22.1743697378554));
#14574=CARTESIAN_POINT('Ctrl Pts',(6.29669095046605,-2.48545882169553,22.1829969401861));
#14575=CARTESIAN_POINT('Ctrl Pts',(6.3592929618526,-2.31337027415241,22.1916241425168));
#14576=CARTESIAN_POINT('Ctrl Pts',(6.42195459207313,-2.14111783860764,22.2002595609373));
#14577=CARTESIAN_POINT('Ctrl Pts',(6.47756425296698,-1.96645349072783,22.2088949793578));
#14578=CARTESIAN_POINT('Ctrl Pts',(6.52597045002582,-1.78997169960584,22.2175303977782));
#14579=CARTESIAN_POINT('Ctrl Pts',(6.57444816034549,-1.61322918177679,22.2261785737993));
#14580=CARTESIAN_POINT('Ctrl Pts',(6.61570106750114,-1.43466415123393,22.2348267498204));
#14581=CARTESIAN_POINT('Ctrl Pts',(6.64962864642111,-1.25488161381691,22.2434749258415));
#14582=CARTESIAN_POINT('Ctrl Pts',(6.65321805562811,-1.23586130303719,22.2443898700734));
#14583=CARTESIAN_POINT('Ctrl Pts',(6.65672552145886,-1.21682736966386,22.2453048143052));
#14584=CARTESIAN_POINT('Ctrl Pts',(6.66015095884106,-1.19778053308965,22.2462197585371));
#14585=CARTESIAN_POINT('Ctrl Pts',(6.69094805157703,-1.02653606797389,22.2544457510784));
#14586=CARTESIAN_POINT('Ctrl Pts',(6.71517681990731,-0.853878309912253,
22.2626717436198));
#14587=CARTESIAN_POINT('Ctrl Pts',(6.73271195522136,-0.68035191483481,22.2708977361612));
#14588=CARTESIAN_POINT('Ctrl Pts',(6.75022870721254,-0.507007439753377,
22.2791151048126));
#14589=CARTESIAN_POINT('Ctrl Pts',(6.76106576472004,-0.332796494650787,
22.287332473464));
#14590=CARTESIAN_POINT('Ctrl Pts',(6.76514880467671,-0.158273973164549,
22.2955498421154));
#14591=CARTESIAN_POINT('Ctrl Pts',(6.76922838109235,0.0161005052164206,
22.3037602401778));
#14592=CARTESIAN_POINT('Ctrl Pts',(6.76656534222491,0.190785677408156,22.3119706382402));
#14593=CARTESIAN_POINT('Ctrl Pts',(6.75713714109871,0.365221379966116,22.3201810363026));
#14594=CARTESIAN_POINT('Ctrl Pts',(6.74771505166959,0.539544007064629,22.3283861120914));
#14595=CARTESIAN_POINT('Ctrl Pts',(6.73153655468924,0.713617130167781,22.3365911878803));
#14596=CARTESIAN_POINT('Ctrl Pts',(6.70863117675751,0.886880338172575,22.3447962636691));
#14597=CARTESIAN_POINT('Ctrl Pts',(6.68573606586565,1.06006588318192,22.3529976616386));
#14598=CARTESIAN_POINT('Ctrl Pts',(6.65612012811828,1.23244188190747,22.3611990596082));
#14599=CARTESIAN_POINT('Ctrl Pts',(6.61986476529523,1.40345270287342,22.3694004575777));
#14600=CARTESIAN_POINT('Ctrl Pts',(6.58361224229438,1.57445012884658,22.3776012131454));
#14601=CARTESIAN_POINT('Ctrl Pts',(6.54072139582365,1.7440822380292,22.3858019687131));
#14602=CARTESIAN_POINT('Ctrl Pts',(6.49132488253577,1.91180288454955,22.3940027242808));
#14603=CARTESIAN_POINT('Ctrl Pts',(6.4419286201587,2.07952267912875,22.4022034381926));
#14604=CARTESIAN_POINT('Ctrl Pts',(6.38602685701169,2.24533068631008,22.4104041521044));
#14605=CARTESIAN_POINT('Ctrl Pts',(6.32380231199367,2.40869535616763,22.4186048660161));
#14606=CARTESIAN_POINT('Ctrl Pts',(6.26156680640956,2.57208880195691,22.4268070244457));
#14607=CARTESIAN_POINT('Ctrl Pts',(6.1930064276042,2.73303771805244,22.4350091828754));
#14608=CARTESIAN_POINT('Ctrl Pts',(6.11835230166785,2.89102993977506,22.443211341305));
#14609=CARTESIAN_POINT('Ctrl Pts',(6.04367149642323,3.04907862352351,22.4514164309579));
#14610=CARTESIAN_POINT('Ctrl Pts',(5.96289275888009,3.20416818419458,22.4596215206108));
#14611=CARTESIAN_POINT('Ctrl Pts',(5.87629349793066,3.35581044252769,22.4678266102638));
#14612=CARTESIAN_POINT('Ctrl Pts',(5.78959530756407,3.50762593421255,22.4760410732615));
#14613=CARTESIAN_POINT('Ctrl Pts',(5.69706348763933,3.65598594434046,22.4842555362593));
#14614=CARTESIAN_POINT('Ctrl Pts',(5.59901975184601,3.80042982022274,22.4924699992571));
#14615=CARTESIAN_POINT('Ctrl Pts',(5.50091792823782,3.94495927453645,22.5006893290646));
#14616=CARTESIAN_POINT('Ctrl Pts',(5.39729789134114,4.08556768157093,22.5089086588721));
#14617=CARTESIAN_POINT('Ctrl Pts',(5.28852202658054,4.22182706590079,22.5171279886796));
#14618=CARTESIAN_POINT('Ctrl Pts',(5.17957762021267,4.35829757588515,22.5253600538403));
#14619=CARTESIAN_POINT('Ctrl Pts',(5.06546165565918,4.49040532590808,22.533592119001));
#14620=CARTESIAN_POINT('Ctrl Pts',(4.94657470504804,4.61775786365839,22.5418241841616));
#14621=CARTESIAN_POINT('Ctrl Pts',(4.83971057728852,4.73223146900103,22.5492237554227));
#14622=CARTESIAN_POINT('Ctrl Pts',(4.72899225507448,4.84286338617217,22.5566233266837));
#14623=CARTESIAN_POINT('Ctrl Pts',(4.61473302931236,4.94939673780286,22.5640228979448));
#14624=CARTESIAN_POINT('Ctrl Pts',(4.4888109016867,5.06680438003875,22.5721777734088));
#14625=CARTESIAN_POINT('Ctrl Pts',(4.35819986244688,5.17959482414312,22.5803326488729));
#14626=CARTESIAN_POINT('Ctrl Pts',(4.22327437086737,5.28736631872379,22.5884875243369));
#14627=CARTESIAN_POINT('Ctrl Pts',(4.08849295352132,5.39502273426872,22.596633691977));
#14628=CARTESIAN_POINT('Ctrl Pts',(3.94940653117599,5.49767063625115,22.6047798596171));
#14629=CARTESIAN_POINT('Ctrl Pts',(3.80642688585204,5.59494444678969,22.6129260272572));
#14630=CARTESIAN_POINT('Ctrl Pts',(3.66360947720701,5.69210788231693,22.6210629515733));
#14631=CARTESIAN_POINT('Ctrl Pts',(3.51690794436196,5.78390916785031,22.6291998758894));
#14632=CARTESIAN_POINT('Ctrl Pts',(3.36676732264903,5.87002272526629,22.6373368002054));
#14633=CARTESIAN_POINT('Ctrl Pts',(3.27872062325342,5.92052214652344,22.6421085223489));
#14634=CARTESIAN_POINT('Ctrl Pts',(3.18949186057883,5.96906631801721,22.6468802444924));
#14635=CARTESIAN_POINT('Ctrl Pts',(3.09917575053257,6.0155962852664,22.6516519666359));
#14636=CARTESIAN_POINT('Origin',(0.,0.,-3.69717978381041));
#14637=CARTESIAN_POINT('',(3.09917575053259,6.01559628526639,25.045602228898));
#14638=CARTESIAN_POINT('',(3.09917575053259,6.01559628526639,24.6513135168612));
#14639=CARTESIAN_POINT('',(3.09917575053259,6.01559628526639,-3.69717978381041));
#14640=CARTESIAN_POINT('',(-6.76701668052783,-0.00100310113704692,23.6971507773732));
#14641=CARTESIAN_POINT('Ctrl Pts',(-6.76699991253939,-0.00108797603646345,
23.69717978381));
#14642=CARTESIAN_POINT('Ctrl Pts',(-6.76696999291398,-0.187182242599655,
23.7058996157294));
#14643=CARTESIAN_POINT('Ctrl Pts',(-6.75925933188796,-0.373124448303,23.7146194476488));
#14644=CARTESIAN_POINT('Ctrl Pts',(-6.74393107196761,-0.558285497348596,
23.7233392795683));
#14645=CARTESIAN_POINT('Ctrl Pts',(-6.72858154856933,-0.743703403200013,
23.7320712077044));
#14646=CARTESIAN_POINT('Ctrl Pts',(-6.70559334447299,-0.928337704410554,
23.7408031358405));
#14647=CARTESIAN_POINT('Ctrl Pts',(-6.6750810980413,-1.11156706256156,23.7495350639766));
#14648=CARTESIAN_POINT('Ctrl Pts',(-6.64450122138508,-1.29520254756596,
23.7582863463829));
#14649=CARTESIAN_POINT('Ctrl Pts',(-6.60636399465147,-1.47742657928581,
23.7670376287892));
#14650=CARTESIAN_POINT('Ctrl Pts',(-6.56083512384141,-1.65762826887358,
23.7757889111954));
#14651=CARTESIAN_POINT('Ctrl Pts',(-6.51525403539874,-1.83803663403789,
23.7845502305572));
#14652=CARTESIAN_POINT('Ctrl Pts',(-6.46226445221919,-2.01641775159363,
23.7933115499189));
#14653=CARTESIAN_POINT('Ctrl Pts',(-6.40208151698484,-2.19217728523061,
23.8020728692807));
#14654=CARTESIAN_POINT('Ctrl Pts',(-6.34178547102113,-2.36826714986534,
23.8108506550913));
#14655=CARTESIAN_POINT('Ctrl Pts',(-6.2742691383388,-2.54172531063156,23.8196284409018));
#14656=CARTESIAN_POINT('Ctrl Pts',(-6.19979607302999,-2.7119767058074,23.8284062267124));
#14657=CARTESIAN_POINT('Ctrl Pts',(-6.1575802052052,-2.80848556261255,23.8333820101589));
#14658=CARTESIAN_POINT('Ctrl Pts',(-6.11312976889147,-2.90396441822418,
23.8383577936054));
#14659=CARTESIAN_POINT('Ctrl Pts',(-6.06649922755934,-2.9983122122324,23.8433335770519));
#14660=CARTESIAN_POINT('Ctrl Pts',(-5.98942166532854,-3.15426360709636,
23.8515582565707));
#14661=CARTESIAN_POINT('Ctrl Pts',(-5.90622510604941,-3.30744646288433,
23.8597829360895));
#14662=CARTESIAN_POINT('Ctrl Pts',(-5.81713249635009,-3.45734848112072,
23.8680076156083));
#14663=CARTESIAN_POINT('Ctrl Pts',(-5.72813353306276,-3.6070929353773,23.8762236500584));
#14664=CARTESIAN_POINT('Ctrl Pts',(-5.63325104221724,-3.75356311375887,
23.8844396845086));
#14665=CARTESIAN_POINT('Ctrl Pts',(-5.53275505583176,-3.89626879105743,
23.8926557189587));
#14666=CARTESIAN_POINT('Ctrl Pts',(-5.43234457257446,-4.03885305274271,
23.9008647631133));
#14667=CARTESIAN_POINT('Ctrl Pts',(-5.32633031100458,-4.17767890086226,
23.9090738072679));
#14668=CARTESIAN_POINT('Ctrl Pts',(-5.21502707051333,-4.31228265003735,
23.9172828514225));
#14669=CARTESIAN_POINT('Ctrl Pts',(-5.10379624014698,-4.44679883056443,
23.9254865550505));
#14670=CARTESIAN_POINT('Ctrl Pts',(-4.98728351227486,-4.57709810820803,
23.9336902586786));
#14671=CARTESIAN_POINT('Ctrl Pts',(-4.86584570656518,-4.70274755434536,
23.9418939623066));
#14672=CARTESIAN_POINT('Ctrl Pts',(-4.74446259179439,-4.82834041278217,
23.9500939713006));
#14673=CARTESIAN_POINT('Ctrl Pts',(-4.61815906675208,-4.94928735456051,
23.9582939802945));
#14674=CARTESIAN_POINT('Ctrl Pts',(-4.48733082216692,-5.06519013388745,
23.9664939892885));
#14675=CARTESIAN_POINT('Ctrl Pts',(-4.35651303888417,-5.18108364538367,
23.9746933425924));
#14676=CARTESIAN_POINT('Ctrl Pts',(-4.22117151899888,-5.29193355379242,
23.9828926958964));
#14677=CARTESIAN_POINT('Ctrl Pts',(-4.08173752687484,-5.39737971257365,
23.9910920492003));
#14678=CARTESIAN_POINT('Ctrl Pts',(-3.94230444381934,-5.50282518387701,
23.9992913490469));
#14679=CARTESIAN_POINT('Ctrl Pts',(-3.79877922696904,-5.60286675861065,
24.0074906488935));
#14680=CARTESIAN_POINT('Ctrl Pts',(-3.65162471579024,-5.69718579081197,
24.0156899487401));
#14681=CARTESIAN_POINT('Ctrl Pts',(-3.50444446874297,-5.7915213184791,24.0238906825631));
#14682=CARTESIAN_POINT('Ctrl Pts',(-3.35363396462095,-5.88013211618855,
24.0320914163861));
#14683=CARTESIAN_POINT('Ctrl Pts',(-3.19968343820939,-5.96274390656253,
24.0402921502092));
#14684=CARTESIAN_POINT('Ctrl Pts',(-3.04567805893446,-6.04538513167347,
24.0484958059691));
#14685=CARTESIAN_POINT('Ctrl Pts',(-2.88853074437985,-6.12202292211131,
24.0566994617291));
#14686=CARTESIAN_POINT('Ctrl Pts',(-2.72875467973028,-6.19242980564577,
24.0649031174891));
#14687=CARTESIAN_POINT('Ctrl Pts',(-2.56879558132745,-6.26291734479142,
24.0731161710641));
#14688=CARTESIAN_POINT('Ctrl Pts',(-2.40620204493545,-6.32715957189716,
24.0813292246391));
#14689=CARTESIAN_POINT('Ctrl Pts',(-2.24150651470688,-6.38497748974314,
24.0895422782141));
#14690=CARTESIAN_POINT('Ctrl Pts',(-2.076713530438,-6.44282961974831,24.0977601916372));
#14691=CARTESIAN_POINT('Ctrl Pts',(-1.90981641503736,-6.49424975748081,
24.1059781050603));
#14692=CARTESIAN_POINT('Ctrl Pts',(-1.74136087992587,-6.53910936488019,
24.1141960184834));
#14693=CARTESIAN_POINT('Ctrl Pts',(-1.5726426110025,-6.58403893813521,24.1224267490794));
#14694=CARTESIAN_POINT('Ctrl Pts',(-1.4023614145147,-6.62238745400381,24.1306574796754));
#14695=CARTESIAN_POINT('Ctrl Pts',(-1.23107259454728,-6.65407764208945,
24.1388882102714));
#14696=CARTESIAN_POINT('Ctrl Pts',(-1.07376429915945,-6.68318128977188,
24.1464471519472));
#14697=CARTESIAN_POINT('Ctrl Pts',(-0.915606438550584,-6.7066697315308,
24.154006093623));
#14698=CARTESIAN_POINT('Ctrl Pts',(-0.757030461101615,-6.72452183288628,
24.1615650352988));
#14699=CARTESIAN_POINT('Ctrl Pts',(-0.585973258148032,-6.74377904052793,
24.1697189274655));
#14700=CARTESIAN_POINT('Ctrl Pts',(-0.413900579235927,-6.75653654667477,
24.1778728196322));
#14701=CARTESIAN_POINT('Ctrl Pts',(-0.241352398616212,-6.76269458275932,
24.1860267117989));
#14702=CARTESIAN_POINT('Ctrl Pts',(-0.069014774984084,-6.76884510431939,
24.1941706539391));
#14703=CARTESIAN_POINT('Ctrl Pts',(0.103796833982148,-6.76841217302138,
24.2023145960794));
#14704=CARTESIAN_POINT('Ctrl Pts',(0.276534249552371,-6.76134733679794,
24.2104585382196));
#14705=CARTESIAN_POINT('Ctrl Pts',(0.449097234996015,-6.75428963464137,
24.2185942566125));
#14706=CARTESIAN_POINT('Ctrl Pts',(0.621585813597099,-6.74061337458658,
24.2267299750054));
#14707=CARTESIAN_POINT('Ctrl Pts',(0.79344869670889,-6.72032202842178,24.2348656933983));
#14708=CARTESIAN_POINT('Ctrl Pts',(0.965174184194921,-6.70004690415523,
24.2429949076985));
#14709=CARTESIAN_POINT('Ctrl Pts',(1.13627461073451,-6.67316726625826,24.2511241219987));
#14710=CARTESIAN_POINT('Ctrl Pts',(1.30620070905545,-6.63973860235951,24.2592533362989));
#14711=CARTESIAN_POINT('Ctrl Pts',(1.47602668918245,-6.60632963418431,24.2673777609743));
#14712=CARTESIAN_POINT('Ctrl Pts',(1.64467936110587,-6.56637939465361,24.2755021856497));
#14713=CARTESIAN_POINT('Ctrl Pts',(1.81161659440151,-6.5199949627963,24.2836266103252));
#14714=CARTESIAN_POINT('Ctrl Pts',(1.97956724357085,-6.47332894774386,24.2918003554593));
#14715=CARTESIAN_POINT('Ctrl Pts',(2.14578118558417,-6.420150409417,24.2999741005935));
#14716=CARTESIAN_POINT('Ctrl Pts',(2.30971819872949,-6.3606203189986,24.3081478457277));
#14717=CARTESIAN_POINT('Ctrl Pts',(2.472605407214,-6.3014714418595,24.3162692485899));
#14718=CARTESIAN_POINT('Ctrl Pts',(2.63324442302417,-6.2360522698325,24.324390651452));
#14719=CARTESIAN_POINT('Ctrl Pts',(2.79112226839095,-6.16457017827619,24.3325120543142));
#14720=CARTESIAN_POINT('Ctrl Pts',(2.9490123200416,-6.09308256010088,24.3406340850804));
#14721=CARTESIAN_POINT('Ctrl Pts',(3.10414044258936,-6.01553123959777,24.3487561158467));
#14722=CARTESIAN_POINT('Ctrl Pts',(3.25601552357071,-5.93217092726319,24.356878146613));
#14723=CARTESIAN_POINT('Ctrl Pts',(3.40793126725568,-5.84878829622001,24.3650023519541));
#14724=CARTESIAN_POINT('Ctrl Pts',(3.55659191443109,-5.75959375251632,24.3731265572952));
#14725=CARTESIAN_POINT('Ctrl Pts',(3.70153279346057,-5.66488693434706,24.3812507626363));
#14726=CARTESIAN_POINT('Ctrl Pts',(3.84804255721475,-5.56915498040281,24.3894629068787));
#14727=CARTESIAN_POINT('Ctrl Pts',(3.99075123289452,-5.46779093087044,24.3976750511212));
#14728=CARTESIAN_POINT('Ctrl Pts',(4.12921144831235,-5.36114743456345,24.4058871953636));
#14729=CARTESIAN_POINT('Ctrl Pts',(4.26640767456626,-5.25547747584145,24.41402437178));
#14730=CARTESIAN_POINT('Ctrl Pts',(4.39943244478516,-5.14462434278932,24.4221615481965));
#14731=CARTESIAN_POINT('Ctrl Pts',(4.52788638337047,-5.02896946692742,24.430298724613));
#14732=CARTESIAN_POINT('Ctrl Pts',(4.65811549162559,-4.91171629808941,24.4385483527684));
#14733=CARTESIAN_POINT('Ctrl Pts',(4.78364622864028,-4.78952797289121,24.4467979809238));
#14734=CARTESIAN_POINT('Ctrl Pts',(4.90410375787502,-4.66283769093415,24.4550476090793));
#14735=CARTESIAN_POINT('Ctrl Pts',(5.02456128710975,-4.53614740897711,24.4632972372347));
#14736=CARTESIAN_POINT('Ctrl Pts',(5.13994540195293,-4.40495550096769,24.4715468653901));
#14737=CARTESIAN_POINT('Ctrl Pts',(5.24992624777084,-4.26972638385258,24.4797964935456));
#14738=CARTESIAN_POINT('Ctrl Pts',(5.35957699649299,-4.13490314412902,24.4880213612232));
#14739=CARTESIAN_POINT('Ctrl Pts',(5.46418475736251,-3.99566400341141,24.4962462289007));
#14740=CARTESIAN_POINT('Ctrl Pts',(5.56337439598018,-3.85242187852683,24.5044710965783));
#14741=CARTESIAN_POINT('Ctrl Pts',(5.66245228636759,-3.7093411319291,24.5126866980219));
#14742=CARTESIAN_POINT('Ctrl Pts',(5.75612400697941,-3.5622666736126,24.5209022994654));
#14743=CARTESIAN_POINT('Ctrl Pts',(5.84405382074282,-3.41164534209833,24.529117900909));
#14744=CARTESIAN_POINT('Ctrl Pts',(5.93190223859301,-3.26116343952523,24.5373258972371));
#14745=CARTESIAN_POINT('Ctrl Pts',(6.01401915525824,-3.10714151042175,24.5455338935652));
#14746=CARTESIAN_POINT('Ctrl Pts',(6.0901113632285,-2.95005636954197,24.5537418898934));
#14747=CARTESIAN_POINT('Ctrl Pts',(6.16614841677648,-2.79308508973186,24.5619439367648));
#14748=CARTESIAN_POINT('Ctrl Pts',(6.23616930395717,-2.63305534219442,24.5701459836362));
#14749=CARTESIAN_POINT('Ctrl Pts',(6.29992607490795,-2.47046968220516,24.5783480305077));
#14750=CARTESIAN_POINT('Ctrl Pts',(6.36364943554375,-2.30796922160778,24.5865457792793));
#14751=CARTESIAN_POINT('Ctrl Pts',(6.42111508868612,-2.14291585001234,24.5947435280508));
#14752=CARTESIAN_POINT('Ctrl Pts',(6.47212263936009,-1.97583337887651,24.6029412768224));
#14753=CARTESIAN_POINT('Ctrl Pts',(6.52312046136822,-1.80878277536633,24.611137462038));
#14754=CARTESIAN_POINT('Ctrl Pts',(6.56766252380892,-1.63970418416487,24.6193336472536));
#14755=CARTESIAN_POINT('Ctrl Pts',(6.60559777384592,-1.46913819981712,24.6275298324693));
#14756=CARTESIAN_POINT('Ctrl Pts',(6.64353021751874,-1.29858483355591,24.6357254113496));
#14757=CARTESIAN_POINT('Ctrl Pts',(6.67485674338557,-1.12654464335548,24.64392099023));
#14758=CARTESIAN_POINT('Ctrl Pts',(6.69947708397811,-0.953570029548029,
24.6521165691103));
#14759=CARTESIAN_POINT('Ctrl Pts',(6.72410008259282,-0.780576741329532,
24.6603130327888));
#14760=CARTESIAN_POINT('Ctrl Pts',(6.74201540292445,-0.606649183840778,
24.6685094964672));
#14761=CARTESIAN_POINT('Ctrl Pts',(6.75317447147819,-0.432346571369847,
24.6767059601457));
#14762=CARTESIAN_POINT('Ctrl Pts',(6.76433677503846,-0.257993428687848,
24.6849047999734));
#14763=CARTESIAN_POINT('Ctrl Pts',(6.76873890255556,-0.0832653724586005,
24.6931036398012));
#14764=CARTESIAN_POINT('Ctrl Pts',(6.76638437996487,0.0912766266220258,
24.701302479629));
#14765=CARTESIAN_POINT('Ctrl Pts',(6.76402739800834,0.266000939786163,24.7095098833783));
#14766=CARTESIAN_POINT('Ctrl Pts',(6.75489967079978,0.440538448253572,24.7177172871275));
#14767=CARTESIAN_POINT('Ctrl Pts',(6.73905683212934,0.614330540776603,24.7259246908768));
#14768=CARTESIAN_POINT('Ctrl Pts',(6.72320550719611,0.788215725541392,24.7341364909458));
#14769=CARTESIAN_POINT('Ctrl Pts',(6.70063194649767,0.961354342896304,24.7423482910148));
#14770=CARTESIAN_POINT('Ctrl Pts',(6.6714432497719,1.13319634886146,24.7505600910838));
#14771=CARTESIAN_POINT('Ctrl Pts',(6.64221158320605,1.30529133027071,24.75878398007));
#14772=CARTESIAN_POINT('Ctrl Pts',(6.60634539242851,1.4760855344447,24.7670078690561));
#14773=CARTESIAN_POINT('Ctrl Pts',(6.56400246541083,1.64504122564772,24.7752317580423));
#14774=CARTESIAN_POINT('Ctrl Pts',(6.52487833286369,1.80115336344255,24.7828304892923));
#14775=CARTESIAN_POINT('Ctrl Pts',(6.48022534294035,1.95569583815561,24.7904292205423));
#14776=CARTESIAN_POINT('Ctrl Pts',(6.43020461554308,2.10825937736523,24.7980279517924));
#14777=CARTESIAN_POINT('Ctrl Pts',(6.37605374060706,2.27341989304355,24.8062541005711));
#14778=CARTESIAN_POINT('Ctrl Pts',(6.31545951335835,2.43672459867157,24.8144802493499));
#14779=CARTESIAN_POINT('Ctrl Pts',(6.24856658841284,2.59763442196371,24.8227063981287));
#14780=CARTESIAN_POINT('Ctrl Pts',(6.18175110838258,2.75835795279459,24.8309230231291));
#14781=CARTESIAN_POINT('Ctrl Pts',(6.10865158953743,2.91669179442607,24.8391396481294));
#14782=CARTESIAN_POINT('Ctrl Pts',(6.02946253448876,3.07211174035001,24.8473562731298));
#14783=CARTESIAN_POINT('Ctrl Pts',(5.94985305419825,3.22835683147,24.8556165212868));
#14784=CARTESIAN_POINT('Ctrl Pts',(5.8640892762609,3.38165663939372,24.8638767694438));
#14785=CARTESIAN_POINT('Ctrl Pts',(5.77241866115026,3.53149710468582,24.8721370176008));
#14786=CARTESIAN_POINT('Ctrl Pts',(5.68139864332798,3.68027413432529,24.8803386417915));
#14787=CARTESIAN_POINT('Ctrl Pts',(5.58455554029678,3.82564044827875,24.8885402659822));
#14788=CARTESIAN_POINT('Ctrl Pts',(5.48217835860883,3.96711601095821,24.8967418901729));
#14789=CARTESIAN_POINT('Ctrl Pts',(5.37985045323717,4.10852347843854,24.9049395667473));
#14790=CARTESIAN_POINT('Ctrl Pts',(5.27199398363578,4.24604363414918,24.9131372433217));
#14791=CARTESIAN_POINT('Ctrl Pts',(5.15894156231535,4.37922492646989,24.9213349198962));
#14792=CARTESIAN_POINT('Ctrl Pts',(5.04592298669535,4.51236634689694,24.9295301422454));
#14793=CARTESIAN_POINT('Ctrl Pts',(4.92771179009345,4.64117121842162,24.9377253645945));
#14794=CARTESIAN_POINT('Ctrl Pts',(4.80468123110802,4.76522058958852,24.9459205869437));
#14795=CARTESIAN_POINT('Ctrl Pts',(4.67997556310149,4.89095894130153,24.9542273904399));
#14796=CARTESIAN_POINT('Ctrl Pts',(4.5503185772531,5.01181105886853,24.9625341939361));
#14797=CARTESIAN_POINT('Ctrl Pts',(4.4161382224553,5.12737868702608,24.9708409974323));
#14798=CARTESIAN_POINT('Ctrl Pts',(4.28373757719628,5.24141347671026,24.9790376231201));
#14799=CARTESIAN_POINT('Ctrl Pts',(4.14693311670552,5.35030288602503,24.9872342488079));
#14800=CARTESIAN_POINT('Ctrl Pts',(4.00616969368798,5.45370455611376,24.9954308744957));
#14801=CARTESIAN_POINT('Ctrl Pts',(3.86256808956303,5.5591910907236,25.0037927668961));
#14802=CARTESIAN_POINT('Ctrl Pts',(3.71484648524175,5.65896599588524,25.0121546592965));
#14803=CARTESIAN_POINT('Ctrl Pts',(3.563508406535,5.75271212877495,25.0205165516968));
#14804=CARTESIAN_POINT('Ctrl Pts',(3.41217032782821,5.84645826166468,25.0288784440972));
#14805=CARTESIAN_POINT('Ctrl Pts',(3.25721612815034,5.93417544472269,25.0372403364976));
#14806=CARTESIAN_POINT('Ctrl Pts',(3.09917575053259,6.01559628526639,25.045602228898));
#14807=CARTESIAN_POINT('Ctrl Pts',(3.09917575053259,6.01559628526639,23.0457515827422));
#14808=CARTESIAN_POINT('Ctrl Pts',(2.93382384459267,6.10078395293758,23.0545010306546));
#14809=CARTESIAN_POINT('Ctrl Pts',(2.76495772122987,6.17915010267048,23.063250478567));
#14810=CARTESIAN_POINT('Ctrl Pts',(2.59315093316716,6.25042856433175,23.0719999264794));
#14811=CARTESIAN_POINT('Ctrl Pts',(2.42134553245622,6.32170645041449,23.0807493037394));
#14812=CARTESIAN_POINT('Ctrl Pts',(2.24659977927596,6.38589665313456,23.0894986809994));
#14813=CARTESIAN_POINT('Ctrl Pts',(2.06950718689924,6.44278115439073,23.0982480582594));
#14814=CARTESIAN_POINT('Ctrl Pts',(1.89241596572858,6.49966521519725,23.1069973677741));
#14815=CARTESIAN_POINT('Ctrl Pts',(1.71297821457185,6.5492436000955,23.1157466772887));
#14816=CARTESIAN_POINT('Ctrl Pts',(1.53180337335822,6.59134792173561,23.1244959868034));
#14817=CARTESIAN_POINT('Ctrl Pts',(1.35062987477754,6.63345193135311,23.1332452314795));
#14818=CARTESIAN_POINT('Ctrl Pts',(1.16771959102918,6.66808192368244,23.1419944761557));
#14819=CARTESIAN_POINT('Ctrl Pts',(0.983693746906448,6.69512028363174,23.1507437208318));
#14820=CARTESIAN_POINT('Ctrl Pts',(0.799669205419473,6.72215845218872,23.159492903576));
#14821=CARTESIAN_POINT('Ctrl Pts',(0.614529402873077,6.74160505424583,23.1682420863201));
#14822=CARTESIAN_POINT('Ctrl Pts',(0.428903127362849,6.75339404354125,23.1769912690643));
#14823=CARTESIAN_POINT('Ctrl Pts',(0.243278104163375,6.76518295330332,23.1857403927829));
#14824=CARTESIAN_POINT('Ctrl Pts',(0.0571669005385083,6.76931433552277,
23.1944895165015));
#14825=CARTESIAN_POINT('Ctrl Pts',(-0.128798404778226,6.76577415902472,
23.2032386402201));
#14826=CARTESIAN_POINT('Ctrl Pts',(-0.314762517259805,6.76223400523438,
23.2119877078194));
#14827=CARTESIAN_POINT('Ctrl Pts',(-0.500580446820209,6.75102239665084,
23.2207367754186));
#14828=CARTESIAN_POINT('Ctrl Pts',(-0.685621118843303,6.7321774101249,23.2294858430178));
#14829=CARTESIAN_POINT('Ctrl Pts',(-0.870660665415034,6.71333253821764,
23.2382348574035));
#14830=CARTESIAN_POINT('Ctrl Pts',(-1.05492267885527,6.68685441030605,23.2469838717893));
#14831=CARTESIAN_POINT('Ctrl Pts',(-1.23778137635278,6.65283295028172,23.2557328861751));
#14832=CARTESIAN_POINT('Ctrl Pts',(-1.42999922978873,6.6170701886186,23.2649296965425));
#14833=CARTESIAN_POINT('Ctrl Pts',(-1.62066601233722,6.57297172934407,23.2741265069099));
#14834=CARTESIAN_POINT('Ctrl Pts',(-1.80906628500412,6.52070304311287,23.2833233172773));
#14835=CARTESIAN_POINT('Ctrl Pts',(-1.98831342545551,6.47097374915023,23.292073315015));
#14836=CARTESIAN_POINT('Ctrl Pts',(-2.16550875896721,6.41384933989522,23.3008233127528));
#14837=CARTESIAN_POINT('Ctrl Pts',(-2.34005036714027,6.3495238624047,23.3095733104905));
#14838=CARTESIAN_POINT('Ctrl Pts',(-2.51458843547106,6.28519968948589,23.3183231307714));
#14839=CARTESIAN_POINT('Ctrl Pts',(-2.68647261718074,6.21367483971091,23.3270729510523));
#14840=CARTESIAN_POINT('Ctrl Pts',(-2.85511905908751,6.13519226743834,23.3358227713331));
#14841=CARTESIAN_POINT('Ctrl Pts',(-3.023762304889,6.05671118252929,23.3445724257917));
#14842=CARTESIAN_POINT('Ctrl Pts',(-3.18916767379916,5.97127275992626,23.3533220802502));
#14843=CARTESIAN_POINT('Ctrl Pts',(-3.35077334102795,5.87916720437992,23.3620717347087));
#14844=CARTESIAN_POINT('Ctrl Pts',(-3.5123761603737,5.78706327195642,23.3708212349772));
#14845=CARTESIAN_POINT('Ctrl Pts',(-3.67017916302295,5.68829258362301,23.3795707352456));
#14846=CARTESIAN_POINT('Ctrl Pts',(-3.82364636566452,5.58319061741049,23.3883202355141));
#14847=CARTESIAN_POINT('Ctrl Pts',(-3.97711106778796,5.47809036367704,23.3970695932225));
#14848=CARTESIAN_POINT('Ctrl Pts',(-4.12623987481933,5.36665920043221,23.4058189509309));
#14849=CARTESIAN_POINT('Ctrl Pts',(-4.27052628213943,5.24927559512324,23.4145683086394));
#14850=CARTESIAN_POINT('Ctrl Pts',(-4.41481053025014,5.13189374643006,23.4233175354159));
#14851=CARTESIAN_POINT('Ctrl Pts',(-4.55425230136587,5.00855981477302,23.4320667621924));
#14852=CARTESIAN_POINT('Ctrl Pts',(-4.68837800630624,4.87969268192003,23.440815988969));
#14853=CARTESIAN_POINT('Ctrl Pts',(-4.82250188228972,4.75082730631731,23.4495650964398));
#14854=CARTESIAN_POINT('Ctrl Pts',(-4.95130963053044,4.61642907903442,23.4583142039107));
#14855=CARTESIAN_POINT('Ctrl Pts',(-5.07436379033446,4.476954447316,23.4670633113815));
#14856=CARTESIAN_POINT('Ctrl Pts',(-5.19741643562872,4.33748153220506,23.4758123111713));
#14857=CARTESIAN_POINT('Ctrl Pts',(-5.31471544462827,4.1929325525452,23.484561310961));
#14858=CARTESIAN_POINT('Ctrl Pts',(-5.42586245275671,4.04379841779545,23.4933103107507));
#14859=CARTESIAN_POINT('Ctrl Pts',(-5.53702160019195,3.89464799484283,23.5020602660929));
#14860=CARTESIAN_POINT('Ctrl Pts',(-5.64202723081293,3.74091164443788,23.510810221435));
#14861=CARTESIAN_POINT('Ctrl Pts',(-5.74052265233007,3.58311159163169,23.5195601767772));
#14862=CARTESIAN_POINT('Ctrl Pts',(-5.83901427066957,3.42531763191717,23.5283097942597));
#14863=CARTESIAN_POINT('Ctrl Pts',(-5.93099603115777,3.26346052695544,23.5370594117421));
#14864=CARTESIAN_POINT('Ctrl Pts',(-6.0161555062279,3.09809004467005,23.5458090292246));
#14865=CARTESIAN_POINT('Ctrl Pts',(-6.10131214578841,2.93272506863742,23.5545583553757));
#14866=CARTESIAN_POINT('Ctrl Pts',(-6.17964682328794,2.76384720416793,23.5633076815268));
#14867=CARTESIAN_POINT('Ctrl Pts',(-6.25089348288613,2.59203002791476,23.5720570076779));
#14868=CARTESIAN_POINT('Ctrl Pts',(-6.32213814889384,2.4202176593689,23.5808060890094));
#14869=CARTESIAN_POINT('Ctrl Pts',(-6.38629508412642,2.24546640831757,23.589555170341));
#14870=CARTESIAN_POINT('Ctrl Pts',(-6.4431463981987,2.06836976659859,23.5983042516726));
#14871=CARTESIAN_POINT('Ctrl Pts',(-6.50000285283756,1.89125711158086,23.607054124107));
#14872=CARTESIAN_POINT('Ctrl Pts',(-6.54955227673301,1.71179891440059,23.6158039965414));
#14873=CARTESIAN_POINT('Ctrl Pts',(-6.59162635926432,1.53060476278229,23.6245538689758));
#14874=CARTESIAN_POINT('Ctrl Pts',(-6.63369752055239,1.34942319164485,23.6333031338983));
#14875=CARTESIAN_POINT('Ctrl Pts',(-6.66829431424292,1.16650618642485,23.6420523988208));
#14876=CARTESIAN_POINT('Ctrl Pts',(-6.69529923745451,0.982474997616288,
23.6508016637433));
#14877=CARTESIAN_POINT('Ctrl Pts',(-6.72230554731471,0.798434359175432,
23.659551377923));
#14878=CARTESIAN_POINT('Ctrl Pts',(-6.74171916496724,0.613279706237988,
23.6683010921027));
#14879=CARTESIAN_POINT('Ctrl Pts',(-6.7534741481729,0.427639953652993,23.6770508062824));
#14880=CARTESIAN_POINT('Ctrl Pts',(-6.7624883775875,0.285283364196907,23.6837604654583));
#14881=CARTESIAN_POINT('Ctrl Pts',(-6.76699999999997,0.142641701104177,
23.6904701246341));
#14882=CARTESIAN_POINT('Ctrl Pts',(-6.767,1.35195985046293E-12,23.69717978381));
#14883=CARTESIAN_POINT('',(-6.76699789935467,0.00533199113308135,23.302820216162));
#14884=CARTESIAN_POINT('Ctrl Pts',(3.09917575053257,6.0155962852664,22.6516519666359));
#14885=CARTESIAN_POINT('Ctrl Pts',(2.94533715167372,6.09485241092214,22.6597798083722));
#14886=CARTESIAN_POINT('Ctrl Pts',(2.78834244546162,6.16826210053875,22.6679076501086));
#14887=CARTESIAN_POINT('Ctrl Pts',(2.62868129189148,6.23556923349102,22.6760354918449));
#14888=CARTESIAN_POINT('Ctrl Pts',(2.46909412599147,6.30284517602633,22.6841595671042));
#14889=CARTESIAN_POINT('Ctrl Pts',(2.30684331009307,6.36402405269745,22.6922836423634));
#14890=CARTESIAN_POINT('Ctrl Pts',(2.14244081522303,6.41889681746533,22.7004077176227));
#14891=CARTESIAN_POINT('Ctrl Pts',(1.97805439270852,6.47376421774902,22.7085309986542));
#14892=CARTESIAN_POINT('Ctrl Pts',(1.81151705421439,6.5223266105014,22.7166542796857));
#14893=CARTESIAN_POINT('Ctrl Pts',(1.64335859477935,6.56442392971119,22.7247775607172));
#14894=CARTESIAN_POINT('Ctrl Pts',(1.47520027491876,6.60652121397947,22.7329008350062));
#14895=CARTESIAN_POINT('Ctrl Pts',(1.30542119148423,6.64215334585694,22.7410241092953));
#14896=CARTESIAN_POINT('Ctrl Pts',(1.13456388177708,6.67121081949648,22.7491473835843));
#14897=CARTESIAN_POINT('Ctrl Pts',(0.963674209275419,6.7002737970331,22.7572721965366));
#14898=CARTESIAN_POINT('Ctrl Pts',(0.791706264416511,6.72275957520087,22.7653970094888));
#14899=CARTESIAN_POINT('Ctrl Pts',(0.619210258008934,6.7386102169792,22.773521822441));
#14900=CARTESIAN_POINT('Ctrl Pts',(0.446648759875735,6.75446687678603,22.7816497201489));
#14901=CARTESIAN_POINT('Ctrl Pts',(0.273559164896786,6.76368335065464,22.7897776178567));
#14902=CARTESIAN_POINT('Ctrl Pts',(0.100494212842556,6.76625375767013,22.7979055155646));
#14903=CARTESIAN_POINT('Ctrl Pts',(-0.0727613266221251,6.76882699534089,
22.8060423641025));
#14904=CARTESIAN_POINT('Ctrl Pts',(-0.245991803204344,6.7647395454642,22.8141792126404));
#14905=CARTESIAN_POINT('Ctrl Pts',(-0.418646239134824,6.75403763140673,
22.8223160611783));
#14906=CARTESIAN_POINT('Ctrl Pts',(-0.591409460085532,6.74332897435462,
22.8304580365305));
#14907=CARTESIAN_POINT('Ctrl Pts',(-0.76359555454526,6.72599758616071,22.8386000118827));
#14908=CARTESIAN_POINT('Ctrl Pts',(-0.934661545511393,6.70214120974352,
22.846741987235));
#14909=CARTESIAN_POINT('Ctrl Pts',(-1.10596394295794,6.67825186475114,22.8548952144773));
#14910=CARTESIAN_POINT('Ctrl Pts',(-1.27614278741816,6.64781958978234,22.8630484417197));
#14911=CARTESIAN_POINT('Ctrl Pts',(-1.44466726065743,6.61099277763821,22.871201668962));
#14912=CARTESIAN_POINT('Ctrl Pts',(-1.51786797138082,6.59499659161958,22.8747431250922));
#14913=CARTESIAN_POINT('Ctrl Pts',(-1.59075676567098,6.5777945740722,22.8782845812223));
#14914=CARTESIAN_POINT('Ctrl Pts',(-1.66329124058518,6.5594017447472,22.8818260373524));
#14915=CARTESIAN_POINT('Ctrl Pts',(-1.83177667506952,6.51667828333269,22.8900522466894));
#14916=CARTESIAN_POINT('Ctrl Pts',(-1.9988504768118,6.46739932862912,22.8982784560264));
#14917=CARTESIAN_POINT('Ctrl Pts',(-2.16396505822729,6.41167249840253,22.9065046653633));
#14918=CARTESIAN_POINT('Ctrl Pts',(-2.32889414048451,6.35600827488222,22.9147216329066));
#14919=CARTESIAN_POINT('Ctrl Pts',(-2.49186804868475,6.2939107140796,22.9229386004498));
#14920=CARTESIAN_POINT('Ctrl Pts',(-2.65235058016763,6.2255381614672,22.931155567993));
#14921=CARTESIAN_POINT('Ctrl Pts',(-2.81268502653112,6.15722869956956,22.9393649533364));
#14922=CARTESIAN_POINT('Ctrl Pts',(-2.97053234668703,6.08265591703279,22.9475743386798));
#14923=CARTESIAN_POINT('Ctrl Pts',(-3.12537258853758,6.00202758930829,22.9557837240232));
#14924=CARTESIAN_POINT('Ctrl Pts',(-3.28010101938799,5.92145748374784,22.9639871813238));
#14925=CARTESIAN_POINT('Ctrl Pts',(-3.43182638023916,5.83484070771945,22.9721906386244));
#14926=CARTESIAN_POINT('Ctrl Pts',(-3.58004968407034,5.74243269525972,22.980394095925));
#14927=CARTESIAN_POINT('Ctrl Pts',(-3.72819568826127,5.65007287431871,22.9885932750569));
#14928=CARTESIAN_POINT('Ctrl Pts',(-3.87284297023566,5.55192802295851,22.9967924541887));
#14929=CARTESIAN_POINT('Ctrl Pts',(-4.01351802524722,5.44829900620512,23.0049916333206));
#14930=CARTESIAN_POINT('Ctrl Pts',(-4.15416657404645,5.34468951539199,23.0131892675504));
#14931=CARTESIAN_POINT('Ctrl Pts',(-4.29084409458544,5.23559812496321,23.0213869017803));
#14932=CARTESIAN_POINT('Ctrl Pts',(-4.42310666570275,5.12136860846941,23.0295845360101));
#14933=CARTESIAN_POINT('Ctrl Pts',(-4.55535968996264,5.00714733718738,23.0377815785257));
#14934=CARTESIAN_POINT('Ctrl Pts',(-4.6831981274305,4.88778891223321,23.0459786210413));
#14935=CARTESIAN_POINT('Ctrl Pts',(-4.80621176726464,4.76367688327062,23.0541756635569));
#14936=CARTESIAN_POINT('Ctrl Pts',(-4.9292388853625,4.63955125569686,23.0623736041997));
#14937=CARTESIAN_POINT('Ctrl Pts',(-5.04743990007538,4.51067124125496,23.0705715448425));
#14938=CARTESIAN_POINT('Ctrl Pts',(-5.16044201700532,4.377456703284,23.0787694854853));
#14939=CARTESIAN_POINT('Ctrl Pts',(-5.27347705328596,4.24420335775606,23.0869698143213));
#14940=CARTESIAN_POINT('Ctrl Pts',(-5.38130994307094,4.1066132469765,23.0951701431573));
#14941=CARTESIAN_POINT('Ctrl Pts',(-5.4836086502579,3.96513873285876,23.1033704719933));
#14942=CARTESIAN_POINT('Ctrl Pts',(-5.58601395535202,3.82351679862657,23.1115793457847));
#14943=CARTESIAN_POINT('Ctrl Pts',(-5.68287334628282,3.67800266550344,23.1197882195761));
#14944=CARTESIAN_POINT('Ctrl Pts',(-5.77389800980859,3.52907789264113,23.1279970933675));
#14945=CARTESIAN_POINT('Ctrl Pts',(-5.86497152526677,3.3800731934967,23.1362103727709));
#14946=CARTESIAN_POINT('Ctrl Pts',(-5.95020389580566,3.22765451829543,23.1444236521743));
#14947=CARTESIAN_POINT('Ctrl Pts',(-6.02935271589693,3.07232726565812,23.1526369315777));
#14948=CARTESIAN_POINT('Ctrl Pts',(-6.10861730357792,2.91677282250004,23.1608622241931));
#14949=CARTESIAN_POINT('Ctrl Pts',(-6.181780408104,2.75830162568904,23.1690875168086));
#14950=CARTESIAN_POINT('Ctrl Pts',(-6.24864764491561,2.59743943330554,23.177312809424));
#14951=CARTESIAN_POINT('Ctrl Pts',(-6.30912102822251,2.45195890377503,23.184751598536));
#14952=CARTESIAN_POINT('Ctrl Pts',(-6.36444557725428,2.304523182898,23.192190387648));
#14953=CARTESIAN_POINT('Ctrl Pts',(-6.41451305705658,2.15553038504463,23.1996291767601));
#14954=CARTESIAN_POINT('Ctrl Pts',(-6.47963464030889,1.96173898736063,23.2093046332913));
#14955=CARTESIAN_POINT('Ctrl Pts',(-6.53601141367244,1.764872190024,23.2189800898225));
#14956=CARTESIAN_POINT('Ctrl Pts',(-6.58338801998961,1.56565998168735,23.2286555463537));
#14957=CARTESIAN_POINT('Ctrl Pts',(-6.6305625635036,1.36729742005137,23.2382897367407));
#14958=CARTESIAN_POINT('Ctrl Pts',(-6.66881347663304,1.16660948169976,23.2479239271277));
#14959=CARTESIAN_POINT('Ctrl Pts',(-6.69793560061278,0.964337954269142,
23.2575581175147));
#14960=CARTESIAN_POINT('Ctrl Pts',(-6.72681638638656,0.763742672966011,
23.2671124683191));
#14961=CARTESIAN_POINT('Ctrl Pts',(-6.74671899741591,0.561590026758002,
23.2766668191235));
#14962=CARTESIAN_POINT('Ctrl Pts',(-6.75749054399143,0.358623127902209,
23.2862211699278));
#14963=CARTESIAN_POINT('Ctrl Pts',(-6.76372844904924,0.241083066587632,
23.2917541853392));
#14964=CARTESIAN_POINT('Ctrl Pts',(-6.76690497100265,0.123270289833604,
23.2972872007506));
#14965=CARTESIAN_POINT('Ctrl Pts',(-6.76699789935467,0.00533199113308068,
23.302820216162));
#14966=CARTESIAN_POINT('Ctrl Pts',(-6.76699789935514,0.00533199053770156,
23.3028202161899));
#14967=CARTESIAN_POINT('Ctrl Pts',(-6.76713557607511,-0.169397890966532,
23.3110175798778));
#14968=CARTESIAN_POINT('Ctrl Pts',(-6.76050144710687,-0.344207078147022,
23.3192149435658));
#14969=CARTESIAN_POINT('Ctrl Pts',(-6.74710394238392,-0.518533885746455,
23.3274123072538));
#14970=CARTESIAN_POINT('Ctrl Pts',(-6.73370718007129,-0.692851033187286,
23.3356092166924));
#14971=CARTESIAN_POINT('Ctrl Pts',(-6.71354780721192,-0.866685496773059,
23.343806126131));
#14972=CARTESIAN_POINT('Ctrl Pts',(-6.68668630651549,-1.03947834910508,
23.3520030355696));
#14973=CARTESIAN_POINT('Ctrl Pts',(-6.6598244339166,-1.21227359378621,23.360200058496));
#14974=CARTESIAN_POINT('Ctrl Pts',(-6.62626030277704,-1.38402684436315,
23.3683970814224));
#14975=CARTESIAN_POINT('Ctrl Pts',(-6.58610592683122,-1.55418715750668,
23.3765941043487));
#14976=CARTESIAN_POINT('Ctrl Pts',(-6.54594372530683,-1.72438063273699,
23.3847927247709));
#14977=CARTESIAN_POINT('Ctrl Pts',(-6.49918880253525,-1.89298020342746,
23.3929913451931));
#14978=CARTESIAN_POINT('Ctrl Pts',(-6.44600368172677,-2.05944787143666,
23.4011899656152));
#14979=CARTESIAN_POINT('Ctrl Pts',(-6.39279856696449,-2.22597811985954,
23.4093916681558));
#14980=CARTESIAN_POINT('Ctrl Pts',(-6.33315854772807,-2.39037452811281,
23.4175933706963));
#14981=CARTESIAN_POINT('Ctrl Pts',(-6.26729514571851,-2.55211687750645,
23.4257950732368));
#14982=CARTESIAN_POINT('Ctrl Pts',(-6.20135727800738,-2.71404209412457,
23.4340060486894));
#14983=CARTESIAN_POINT('Ctrl Pts',(-6.12918210721176,-2.87330692569047,
23.442217024142));
#14984=CARTESIAN_POINT('Ctrl Pts',(-6.05102862629684,-3.02941274238691,
23.4504279995946));
#14985=CARTESIAN_POINT('Ctrl Pts',(-5.97282751887836,-3.18561368951322,
23.4586439787917));
#14986=CARTESIAN_POINT('Ctrl Pts',(-5.88864101160007,-3.33865147122337,
23.4668599579887));
#14987=CARTESIAN_POINT('Ctrl Pts',(-5.79877265229455,-3.48805457626466,
23.4750759371858));
#14988=CARTESIAN_POINT('Ctrl Pts',(-5.70877164640232,-3.63767820176588,
23.4833040432494));
#14989=CARTESIAN_POINT('Ctrl Pts',(-5.6130722286129,-3.78365613277414,23.4915321493131));
#14990=CARTESIAN_POINT('Ctrl Pts',(-5.51202031121251,-3.92554723430768,
23.4997602553767));
#14991=CARTESIAN_POINT('Ctrl Pts',(-5.43967496168524,-4.02713027794834,
23.505650942307));
#14992=CARTESIAN_POINT('Ctrl Pts',(-5.36458708274533,-4.12661930799459,
23.5115416292374));
#14993=CARTESIAN_POINT('Ctrl Pts',(-5.28689545463958,-4.22386380600883,
23.5174323161678));
#14994=CARTESIAN_POINT('Ctrl Pts',(-5.17937227900346,-4.35844764077412,
23.525584872381));
#14995=CARTESIAN_POINT('Ctrl Pts',(-5.0665385954702,-4.48913361742515,23.5337374285943));
#14996=CARTESIAN_POINT('Ctrl Pts',(-4.94870871398186,-4.61547083883757,
23.5418899848075));
#14997=CARTESIAN_POINT('Ctrl Pts',(-4.83101534125174,-4.74166169553339,
23.5500330960879));
#14998=CARTESIAN_POINT('Ctrl Pts',(-4.70833753934842,-4.86351356128222,
23.5581762073682));
#14999=CARTESIAN_POINT('Ctrl Pts',(-4.58103149679524,-4.98060633109765,
23.5663193186486));
#15000=CARTESIAN_POINT('Ctrl Pts',(-4.45384617685171,-5.09758806341274,
23.5744547079259));
#15001=CARTESIAN_POINT('Ctrl Pts',(-4.32204162120189,-5.20981943880274,
23.5825900972033));
#15002=CARTESIAN_POINT('Ctrl Pts',(-4.18601269475671,-5.31691515066168,
23.5907254864806));
#15003=CARTESIAN_POINT('Ctrl Pts',(-4.05008417975476,-5.42393180848944,
23.5988548705192));
#15004=CARTESIAN_POINT('Ctrl Pts',(-3.90993778899949,-5.52582012606068,
23.6069842545578));
#15005=CARTESIAN_POINT('Ctrl Pts',(-3.76600347417976,-5.62223326023263,
23.6151136385964));
#15006=CARTESIAN_POINT('Ctrl Pts',(-3.6221451731738,-5.71859547722034,23.6232387293886));
#15007=CARTESIAN_POINT('Ctrl Pts',(-3.47450323514168,-5.80948806641062,
23.6313638201807));
#15008=CARTESIAN_POINT('Ctrl Pts',(-3.32353875816129,-5.89460593449636,
23.6394889109729));
#15009=CARTESIAN_POINT('Ctrl Pts',(-3.17199801704549,-5.98004871593683,
23.647645016998));
#15010=CARTESIAN_POINT('Ctrl Pts',(-3.0171096184973,-6.05967237844505,23.6558011230231));
#15011=CARTESIAN_POINT('Ctrl Pts',(-2.85936768841479,-6.13321330319185,
23.6639572290482));
#15012=CARTESIAN_POINT('Ctrl Pts',(-2.70226064107286,-6.2064582390166,23.6720805082216));
#15013=CARTESIAN_POINT('Ctrl Pts',(-2.54232333238472,-6.27366917390214,
23.680203787395));
#15014=CARTESIAN_POINT('Ctrl Pts',(-2.38006652956413,-6.33463276874426,
23.6883270665684));
#15015=CARTESIAN_POINT('Ctrl Pts',(-2.21778812087925,-6.39560448140415,
23.6964514274251));
#15016=CARTESIAN_POINT('Ctrl Pts',(-2.05318994535597,-6.45032706837799,
23.7045757882818));
#15017=CARTESIAN_POINT('Ctrl Pts',(-1.88680045021287,-6.49863624625017,
23.7127001491384));
#15018=CARTESIAN_POINT('Ctrl Pts',(-1.72035714244404,-6.54696104796751,
23.7208271375239));
#15019=CARTESIAN_POINT('Ctrl Pts',(-1.552121712547,-6.58886820827906,23.7289541259094));
#15020=CARTESIAN_POINT('Ctrl Pts',(-1.38263534055174,-6.62424399573698,
23.7370811142948));
#15021=CARTESIAN_POINT('Ctrl Pts',(-1.21205325845893,-6.65984848363298,
23.7452606427349));
#15022=CARTESIAN_POINT('Ctrl Pts',(-1.04020437169081,-6.68883677994144,
23.7534401711749));
#15023=CARTESIAN_POINT('Ctrl Pts',(-0.867647383137596,-6.7111457306882,
23.761619699615));
#15024=CARTESIAN_POINT('Ctrl Pts',(-0.695903021073178,-6.73334962139384,
23.7697607080187));
#15025=CARTESIAN_POINT('Ctrl Pts',(-0.523457581893076,-6.7489369726926,
23.7779017164223));
#15026=CARTESIAN_POINT('Ctrl Pts',(-0.350863250401583,-6.75789789649989,
23.786042724826));
#15027=CARTESIAN_POINT('Ctrl Pts',(-0.177043946597487,-6.76692241963553,
23.7942415132843));
#15028=CARTESIAN_POINT('Ctrl Pts',(-0.00307400670362995,-6.76922610362182,
23.8024403017425));
#15029=CARTESIAN_POINT('Ctrl Pts',(0.17048681583121,-6.76485204905678,23.8106390902007));
#15030=CARTESIAN_POINT('Ctrl Pts',(0.34404763836605,-6.76047799449174,23.818837878659));
#15031=CARTESIAN_POINT('Ctrl Pts',(0.517198977055867,-6.74942628968219,
23.8270366671172));
#15032=CARTESIAN_POINT('Ctrl Pts',(0.689390928840013,-6.73179241712288,
23.8352354555755));
#15033=CARTESIAN_POINT('Ctrl Pts',(0.862302448461131,-6.71408485489688,
23.8434685057075));
#15034=CARTESIAN_POINT('Ctrl Pts',(1.03478406018257,-6.68968507259293,23.8517015558395));
#15035=CARTESIAN_POINT('Ctrl Pts',(1.20627809779211,-6.65861713502038,23.8599346059715));
#15036=CARTESIAN_POINT('Ctrl Pts',(1.3775679123646,-6.62758619458578,23.8681578518063));
#15037=CARTESIAN_POINT('Ctrl Pts',(1.54787214564144,-6.58990297409811,23.8763810976412));
#15038=CARTESIAN_POINT('Ctrl Pts',(1.71663670563642,-6.54564339242994,23.8846043434761));
#15039=CARTESIAN_POINT('Ctrl Pts',(1.88523407157315,-6.50142765846935,23.8928194425896));
#15040=CARTESIAN_POINT('Ctrl Pts',(2.05229445788805,-6.45064862859255,23.9010345417031));
#15041=CARTESIAN_POINT('Ctrl Pts',(2.21727234799183,-6.39343353252623,23.9092496408166));
#15042=CARTESIAN_POINT('Ctrl Pts',(2.38211980422056,-6.33626367153163,23.9174582449555));
#15043=CARTESIAN_POINT('Ctrl Pts',(2.54488770675343,-6.2726679963467,23.9256668490944));
#15044=CARTESIAN_POINT('Ctrl Pts',(2.70504403829243,-6.20282401418085,23.9338754532333));
#15045=CARTESIAN_POINT('Ctrl Pts',(2.86510578368002,-6.13302128092104,23.9420792094822));
#15046=CARTESIAN_POINT('Ctrl Pts',(3.02255870322167,-6.05697773478686,23.9502829657311));
#15047=CARTESIAN_POINT('Ctrl Pts',(3.17688907735988,-5.97491964717112,23.95848672198));
#15048=CARTESIAN_POINT('Ctrl Pts',(3.33117378903145,-5.89288583847462,23.9666880509443));
#15049=CARTESIAN_POINT('Ctrl Pts',(3.48233747797266,-5.80484119763091,23.9748893799086));
#15050=CARTESIAN_POINT('Ctrl Pts',(3.62988921017095,-5.71105886170722,23.9830907088729));
#15051=CARTESIAN_POINT('Ctrl Pts',(3.77742059357683,-5.6172894592629,23.9912909067956));
#15052=CARTESIAN_POINT('Ctrl Pts',(3.92134070962703,-5.51778412914224,23.9994911047183));
#15053=CARTESIAN_POINT('Ctrl Pts',(4.06118589512329,-5.41286043836821,24.007691302641));
#15054=CARTESIAN_POINT('Ctrl Pts',(4.20103713742628,-5.30793220326529,24.0158918557209));
#15055=CARTESIAN_POINT('Ctrl Pts',(4.33681281092668,-5.19758535496905,24.0240924088007));
#15056=CARTESIAN_POINT('Ctrl Pts',(4.46808070948705,-5.08217903792357,24.0322929618806));
#15057=CARTESIAN_POINT('Ctrl Pts',(4.59937808167961,-4.96674680865295,24.0404953562338));
#15058=CARTESIAN_POINT('Ctrl Pts',(4.72616539402512,-4.84625308455035,24.048697750587));
#15059=CARTESIAN_POINT('Ctrl Pts',(4.8480457783765,-4.72109533167525,24.0569001449402));
#15060=CARTESIAN_POINT('Ctrl Pts',(4.97004014231265,-4.59582053429968,24.065110209974));
#15061=CARTESIAN_POINT('Ctrl Pts',(5.08711815984872,-4.46587325088116,24.0733202750079));
#15062=CARTESIAN_POINT('Ctrl Pts',(5.19892127951334,-4.33168633783927,24.0815303400417));
#15063=CARTESIAN_POINT('Ctrl Pts',(5.3107779061677,-4.19743520532121,24.089744334267));
#15064=CARTESIAN_POINT('Ctrl Pts',(5.41735438318175,-4.05894068144835,24.0979583284923));
#15065=CARTESIAN_POINT('Ctrl Pts',(5.51833438096683,-3.91666626863197,24.1061723227177));
#15066=CARTESIAN_POINT('Ctrl Pts',(5.61945204812114,-3.77419788840521,24.1143975153528));
#15067=CARTESIAN_POINT('Ctrl Pts',(5.7149577917135,-3.62793962047484,24.122622707988));
#15068=CARTESIAN_POINT('Ctrl Pts',(5.80457966436447,-3.47838237116717,24.1308479006232));
#15069=CARTESIAN_POINT('Ctrl Pts',(5.88517642248584,-3.34388585718901,24.1382447987432));
#15070=CARTESIAN_POINT('Ctrl Pts',(5.96101520657425,-3.20672183596591,24.1456416968632));
#15071=CARTESIAN_POINT('Ctrl Pts',(6.03193127058848,-3.06726166912717,24.1530385949831));
#15072=CARTESIAN_POINT('Ctrl Pts',(6.11482249109594,-2.90425172769677,24.161684561474));
#15073=CARTESIAN_POINT('Ctrl Pts',(6.19117579758961,-2.7377344975215,24.1703305279649));
#15074=CARTESIAN_POINT('Ctrl Pts',(6.26070146200113,-2.56824963811873,24.1789764944558));
#15075=CARTESIAN_POINT('Ctrl Pts',(6.3301381936358,-2.39898157289271,24.1876114015801));
#15076=CARTESIAN_POINT('Ctrl Pts',(6.3927645830851,-2.22675372867375,24.1962463087045));
#15077=CARTESIAN_POINT('Ctrl Pts',(6.44833746475606,-2.0521288801202,24.2048812158288));
#15078=CARTESIAN_POINT('Ctrl Pts',(6.50575532124491,-1.87170662753666,24.2138027949003));
#15079=CARTESIAN_POINT('Ctrl Pts',(6.55564310865245,-1.68872575085632,24.2227243739718));
#15080=CARTESIAN_POINT('Ctrl Pts',(6.59778616853993,-1.50383066673852,24.2316459530433));
#15081=CARTESIAN_POINT('Ctrl Pts',(6.63846241780019,-1.32537095003421,24.2402570120191));
#15082=CARTESIAN_POINT('Ctrl Pts',(6.67192385554868,-1.14512835758297,24.2488680709948));
#15083=CARTESIAN_POINT('Ctrl Pts',(6.69802751434444,-0.963699339568564,
24.2574791299705));
#15084=CARTESIAN_POINT('Ctrl Pts',(6.72410655618508,-0.782441417492405,
24.2660820683201));
#15085=CARTESIAN_POINT('Ctrl Pts',(6.74284160978644,-0.599999601410085,
24.2746850066698));
#15086=CARTESIAN_POINT('Ctrl Pts',(6.75414064780855,-0.416980946351574,
24.2832879450194));
#15087=CARTESIAN_POINT('Ctrl Pts',(6.76542703352186,-0.234167229849509,
24.2918812500682));
#15088=CARTESIAN_POINT('Ctrl Pts',(6.76929399627383,-0.0507782667061611,
24.3004745551169));
#15089=CARTESIAN_POINT('Ctrl Pts',(6.76570124722964,0.132573124106202,24.3090678601657));
#15090=CARTESIAN_POINT('Ctrl Pts',(6.76530095617885,0.15300147019735,24.3100252950061));
#15091=CARTESIAN_POINT('Ctrl Pts',(6.76480811620918,0.17342934465578,24.3109827298466));
#15092=CARTESIAN_POINT('Ctrl Pts',(6.76422271154694,0.193855896460541,24.311940164687));
#15093=CARTESIAN_POINT('Ctrl Pts',(6.75896700501599,0.377243506179835,24.3205359222346));
#15094=CARTESIAN_POINT('Ctrl Pts',(6.74625221732102,0.560309629723236,24.3291316797821));
#15095=CARTESIAN_POINT('Ctrl Pts',(6.72614799984899,0.742443320481379,24.3377274373297));
#15096=CARTESIAN_POINT('Ctrl Pts',(6.70602502445856,0.924746948165146,24.3463312150113));
#15097=CARTESIAN_POINT('Ctrl Pts',(6.67849889093654,1.10611610306767,24.3549349926929));
#15098=CARTESIAN_POINT('Ctrl Pts',(6.64369066829049,1.2859484064572,24.3635387703745));
#15099=CARTESIAN_POINT('Ctrl Pts',(6.60751445205653,1.4728482766237,24.3724806840425));
#15100=CARTESIAN_POINT('Ctrl Pts',(6.56347227113019,1.65808768593789,24.3814225977106));
#15101=CARTESIAN_POINT('Ctrl Pts',(6.51175715352324,1.84100727145195,24.3903645113786));
#15102=CARTESIAN_POINT('Ctrl Pts',(6.46186215344655,2.01748898812556,24.3989917137093));
#15103=CARTESIAN_POINT('Ctrl Pts',(6.40482524950864,2.19181112399806,24.40761891604));
#15104=CARTESIAN_POINT('Ctrl Pts',(6.34086935583955,2.36340111114786,24.4162461183707));
#15105=CARTESIAN_POINT('Ctrl Pts',(6.2768525539714,2.53515451149533,24.4248815367911));
#15106=CARTESIAN_POINT('Ctrl Pts',(6.2059037247145,2.70417028718337,24.4335169552115));
#15107=CARTESIAN_POINT('Ctrl Pts',(6.1282930936579,2.869897691247,24.4421523736319));
#15108=CARTESIAN_POINT('Ctrl Pts',(6.05056780394805,3.03586993394548,24.450800549653));
#15109=CARTESIAN_POINT('Ctrl Pts',(5.96616118165986,3.19854382427801,24.4594487256742));
#15110=CARTESIAN_POINT('Ctrl Pts',(5.87538908268016,3.35739365090286,24.4680969016953));
#15111=CARTESIAN_POINT('Ctrl Pts',(5.86578573878774,3.37419936025052,24.4690118459272));
#15112=CARTESIAN_POINT('Ctrl Pts',(5.85611118664697,3.39096229487044,24.469926790159));
#15113=CARTESIAN_POINT('Ctrl Pts',(5.84636582806103,3.40768185200442,24.4708417343908));
#15114=CARTESIAN_POINT('Ctrl Pts',(5.75875476621719,3.55799116501222,24.4790671100886));
#15115=CARTESIAN_POINT('Ctrl Pts',(5.66522835322318,3.70511687059272,24.4872924857864));
#15116=CARTESIAN_POINT('Ctrl Pts',(5.56604438093354,3.84856323184096,24.4955178614842));
#15117=CARTESIAN_POINT('Ctrl Pts',(5.46695943896388,3.99186636895002,24.5037350245488));
#15118=CARTESIAN_POINT('Ctrl Pts',(5.36222838635197,4.13149718368364,24.5119521876134));
#15119=CARTESIAN_POINT('Ctrl Pts',(5.25215449663794,4.26698513513298,24.5201693506779));
#15120=CARTESIAN_POINT('Ctrl Pts',(5.14217055389574,4.40236237248852,24.5283797990808));
#15121=CARTESIAN_POINT('Ctrl Pts',(5.02685269264245,4.53360321139852,24.5365902474836));
#15122=CARTESIAN_POINT('Ctrl Pts',(4.90654704385762,4.66026663469078,24.5448006958865));
#15123=CARTESIAN_POINT('Ctrl Pts',(4.78631789509974,4.78684951517067,24.5530059234245));
#15124=CARTESIAN_POINT('Ctrl Pts',(4.66110752185817,4.90886051858895,24.5612111509626));
#15125=CARTESIAN_POINT('Ctrl Pts',(4.53130186876925,5.0258921968232,24.5694163785007));
#15126=CARTESIAN_POINT('Ctrl Pts',(4.40155390317331,5.14287186450201,24.577617959518));
#15127=CARTESIAN_POINT('Ctrl Pts',(4.26721499183724,5.25487637611436,24.5858195405353));
#15128=CARTESIAN_POINT('Ctrl Pts',(4.1287074736729,5.36153556332862,24.5940211215526));
#15129=CARTESIAN_POINT('Ctrl Pts',(3.99023523451358,5.46816758356992,24.6022206135598));
#15130=CARTESIAN_POINT('Ctrl Pts',(3.84759678834175,5.56945677466129,24.6104201055669));
#15131=CARTESIAN_POINT('Ctrl Pts',(3.7012470958779,5.66507360369267,24.618619597574));
#15132=CARTESIAN_POINT('Ctrl Pts',(3.55489272125638,5.760693491788,24.626819351907));
#15133=CARTESIAN_POINT('Ctrl Pts',(3.40482716178231,5.85064045758079,24.63501910624));
#15134=CARTESIAN_POINT('Ctrl Pts',(3.25153405582535,5.93462848742935,24.6432188605731));
#15135=CARTESIAN_POINT('Ctrl Pts',(3.20109128426322,5.96226566639547,24.6459170793358));
#15136=CARTESIAN_POINT('Ctrl Pts',(3.15029924130007,5.98925796810617,24.6486152980985));
#15137=CARTESIAN_POINT('Ctrl Pts',(3.0991757505326,6.01559628526638,24.6513135168612));
#15138=CARTESIAN_POINT('Origin',(0.,0.,-3.69717978381041));
#15139=CARTESIAN_POINT('',(3.09917575053259,6.01559628526639,27.0457515827422));
#15140=CARTESIAN_POINT('',(3.09917575053263,6.01559628526637,26.6512724846455));
#15141=CARTESIAN_POINT('',(3.09917575053259,6.01559628526639,-3.69717978381041));
#15142=CARTESIAN_POINT('',(-6.767,1.30221998277929E-12,25.69717978381));
#15143=CARTESIAN_POINT('Ctrl Pts',(-6.767,1.30221998655608E-12,25.69717978381));
#15144=CARTESIAN_POINT('Ctrl Pts',(-6.76700000000004,-0.186007249414475,
25.705929295616));
#15145=CARTESIAN_POINT('Ctrl Pts',(-6.75932637295444,-0.372014355526427,
25.7146788074219));
#15146=CARTESIAN_POINT('Ctrl Pts',(-6.74400518266936,-0.557389537154042,
25.7234283192279));
#15147=CARTESIAN_POINT('Ctrl Pts',(-6.72868405709656,-0.742763935810438,
25.7321777940784));
#15148=CARTESIAN_POINT('Ctrl Pts',(-6.70571545653004,-0.927506129694126,
25.740927268929));
#15149=CARTESIAN_POINT('Ctrl Pts',(-6.67517739415664,-1.1109886392489,25.7496767437795));
#15150=CARTESIAN_POINT('Ctrl Pts',(-6.64463945823084,-1.29447038906585,
25.7584261824015));
#15151=CARTESIAN_POINT('Ctrl Pts',(-6.60653217027138,-1.47669218228305,
25.7671756210235));
#15152=CARTESIAN_POINT('Ctrl Pts',(-6.56098496116688,-1.65703510504214,
25.7759250596455));
#15153=CARTESIAN_POINT('Ctrl Pts',(-6.51543793687485,-1.83737729604137,
25.7846744627657));
#15154=CARTESIAN_POINT('Ctrl Pts',(-6.46245112202596,-2.01584035397192,
25.7934238658859));
#15155=CARTESIAN_POINT('Ctrl Pts',(-6.40220448416187,-2.19181813638304,
25.8021732690062));
#15156=CARTESIAN_POINT('Ctrl Pts',(-6.34195808575128,-2.36779521936102,
25.8109226373515));
#15157=CARTESIAN_POINT('Ctrl Pts',(-6.27445201489171,-2.54128677544984,
25.8196720056967));
#15158=CARTESIAN_POINT('Ctrl Pts',(-6.19991555136116,-2.71170355237995,
25.828421374042));
#15159=CARTESIAN_POINT('Ctrl Pts',(-6.12537937788965,-2.88211966613227,
25.8371707083391));
#15160=CARTESIAN_POINT('Ctrl Pts',(-6.04381298133538,-3.04946076210601,
25.8459200426361));
#15161=CARTESIAN_POINT('Ctrl Pts',(-5.95549339426221,-3.21315848207012,
25.8546693769332));
#15162=CARTESIAN_POINT('Ctrl Pts',(-5.86717414355083,-3.3768555785977,25.8634186779087));
#15163=CARTESIAN_POINT('Ctrl Pts',(-5.77210188986169,-3.53690907467423,
25.8721679788843));
#15164=CARTESIAN_POINT('Ctrl Pts',(-5.67059953467009,-3.69277536784996,
25.8809172798598));
#15165=CARTESIAN_POINT('Ctrl Pts',(-5.56909755761702,-3.84864108035884,
25.8896665482406));
#15166=CARTESIAN_POINT('Ctrl Pts',(-5.46116568338003,-4.00031938104371,
25.8984158166213));
#15167=CARTESIAN_POINT('Ctrl Pts',(-5.34717048686043,-4.1472951166331,25.9071650850021));
#15168=CARTESIAN_POINT('Ctrl Pts',(-5.2331757055546,-4.29427031688109,25.9159143215147));
#15169=CARTESIAN_POINT('Ctrl Pts',(-5.11311782178764,-4.43654275987176,
25.9246635580273));
#15170=CARTESIAN_POINT('Ctrl Pts',(-4.98740459171991,-4.57362924147675,
25.9334127945399));
#15171=CARTESIAN_POINT('Ctrl Pts',(-4.86169180910809,-4.71071523514457,
25.9421619999111));
#15172=CARTESIAN_POINT('Ctrl Pts',(-4.73032391415414,-4.8426150931654,25.9509112052822));
#15173=CARTESIAN_POINT('Ctrl Pts',(-4.59374707237279,-4.96888084331536,
25.9596604106533));
#15174=CARTESIAN_POINT('Ctrl Pts',(-4.45717070537384,-5.0951461545274,25.9684095856095));
#15175=CARTESIAN_POINT('Ctrl Pts',(-4.31538563819486,-5.21577720253652,
25.9771587605657));
#15176=CARTESIAN_POINT('Ctrl Pts',(-4.1688734129062,-5.33036429028672,25.985907935522));
#15177=CARTESIAN_POINT('Ctrl Pts',(-4.02236168477306,-5.444950989212,25.9946570807899));
#15178=CARTESIAN_POINT('Ctrl Pts',(-3.87112305634402,-5.55349359238785,
26.0034062260578));
#15179=CARTESIAN_POINT('Ctrl Pts',(-3.71567117316691,-5.65562346102501,
26.0121553713257));
#15180=CARTESIAN_POINT('Ctrl Pts',(-3.56021980457252,-5.75775299158799,
26.0209044876319));
#15181=CARTESIAN_POINT('Ctrl Pts',(-3.40055544862332,-5.85346967275385,
26.0296536039381));
#15182=CARTESIAN_POINT('Ctrl Pts',(-3.2372203632334,-5.94244842803596,26.0384027202442));
#15183=CARTESIAN_POINT('Ctrl Pts',(-3.07388580496,-6.03142689616498,26.0471518083152));
#15184=CARTESIAN_POINT('Ctrl Pts',(-2.90688079257678,-6.11366734484836,
26.0559008963861));
#15185=CARTESIAN_POINT('Ctrl Pts',(-2.73677251094603,-6.18889046787307,
26.064649984457));
#15186=CARTESIAN_POINT('Ctrl Pts',(-2.56666476416654,-6.26411335438266,
26.0733990450193));
#15187=CARTESIAN_POINT('Ctrl Pts',(-2.39345402972124,-6.33231884350278,
26.0821481055815));
#15188=CARTESIAN_POINT('Ctrl Pts',(-2.21772856474091,-6.39327529621025,
26.0908971661437));
#15189=CARTESIAN_POINT('Ctrl Pts',(-2.04200363768364,-6.4542315623205,26.0996461999237));
#15190=CARTESIAN_POINT('Ctrl Pts',(-1.8637642662023,-6.50793874252015,26.1083952337037));
#15191=CARTESIAN_POINT('Ctrl Pts',(-1.68361578194868,-6.55421443796076,
26.1171442674836));
#15192=CARTESIAN_POINT('Ctrl Pts',(-1.50346783420026,-6.60048999558644,
26.1258932752079));
#15193=CARTESIAN_POINT('Ctrl Pts',(-1.32141106257383,-6.63933404145469,
26.1346422829321));
#15194=CARTESIAN_POINT('Ctrl Pts',(-1.13806375959158,-6.6706146552701,26.1433912906564));
#15195=CARTESIAN_POINT('Ctrl Pts',(-0.954716987419779,-6.70189517852473,
26.1521402730513));
#15196=CARTESIAN_POINT('Ctrl Pts',(-0.770079973809986,-6.72561226535828,
26.1608892554462));
#15197=CARTESIAN_POINT('Ctrl Pts',(-0.584779770552046,-6.74168536939786,
26.1696382378411));
#15198=CARTESIAN_POINT('Ctrl Pts',(-0.391490647553508,-6.75845143942396,
26.1787644185171));
#15199=CARTESIAN_POINT('Ctrl Pts',(-0.197480213103939,-6.76689975924028,
26.1878905991932));
#15200=CARTESIAN_POINT('Ctrl Pts',(-0.00346532629740909,-6.76699911271707,
26.1970167798692));
#15201=CARTESIAN_POINT('Ctrl Pts',(0.184486595296416,-6.76709536139772,
26.2058577673992));
#15202=CARTESIAN_POINT('Ctrl Pts',(0.37244237818556,-6.75935659726768,26.2146987549291));
#15203=CARTESIAN_POINT('Ctrl Pts',(0.559750217722389,-6.74380965729014,
26.223539742459));
#15204=CARTESIAN_POINT('Ctrl Pts',(0.745129914458067,-6.7284227571725,26.2322897210568));
#15205=CARTESIAN_POINT('Ctrl Pts',(0.929874656314509,-6.70538772273468,
26.2410396996546));
#15206=CARTESIAN_POINT('Ctrl Pts',(1.11335688289811,-6.67478280180737,26.2497896782523));
#15207=CARTESIAN_POINT('Ctrl Pts',(1.29683723118884,-6.64417819418018,26.2585395672773));
#15208=CARTESIAN_POINT('Ctrl Pts',(1.47905480730257,-6.6060039023007,26.2672894563022));
#15209=CARTESIAN_POINT('Ctrl Pts',(1.65939064804824,-6.5603895979713,26.2760393453271));
#15210=CARTESIAN_POINT('Ctrl Pts',(1.83972470264284,-6.51477574543251,26.2847891476881));
#15211=CARTESIAN_POINT('Ctrl Pts',(2.0181767812587,-6.46172209820093,26.2935389500491));
#15212=CARTESIAN_POINT('Ctrl Pts',(2.19414072347705,-6.40140886724006,26.30228875241));
#15213=CARTESIAN_POINT('Ctrl Pts',(2.37010298132121,-6.34109621361365,26.3110384710155));
#15214=CARTESIAN_POINT('Ctrl Pts',(2.54357687926936,-6.27352420825962,26.319788189621));
#15215=CARTESIAN_POINT('Ctrl Pts',(2.71397317789993,-6.19892237325487,26.3285379082265));
#15216=CARTESIAN_POINT('Ctrl Pts',(2.88436790207219,-6.12432122756955,26.3372875459847));
#15217=CARTESIAN_POINT('Ctrl Pts',(3.05168482126272,-6.04269049717409,26.346037183743));
#15218=CARTESIAN_POINT('Ctrl Pts',(3.21535561997401,-5.95430745234923,26.3547868215012));
#15219=CARTESIAN_POINT('Ctrl Pts',(3.3790249607529,-5.86592519481511,26.3635363813203));
#15220=CARTESIAN_POINT('Ctrl Pts',(3.53904799384881,-5.77079087940228,26.3722859411393));
#15221=CARTESIAN_POINT('Ctrl Pts',(3.69488118814988,-5.66922763747022,26.3810355009583));
#15222=CARTESIAN_POINT('Ctrl Pts',(3.85071304610837,-5.56766526649049,26.3897849857457));
#15223=CARTESIAN_POINT('Ctrl Pts',(4.00235489705972,-5.45967423580711,26.3985344705332));
#15224=CARTESIAN_POINT('Ctrl Pts',(4.14929168607658,-5.34562133936325,26.4072839553206));
#15225=CARTESIAN_POINT('Ctrl Pts',(4.29622726385752,-5.23156938308534,26.4160333679839));
#15226=CARTESIAN_POINT('Ctrl Pts',(4.43845763092054,-5.11145583677213,26.4247827806472));
#15227=CARTESIAN_POINT('Ctrl Pts',(4.57549970660941,-4.98568866204231,26.4335321933105));
#15228=CARTESIAN_POINT('Ctrl Pts',(4.71254069815276,-4.8599224822618,26.4422815367568));
#15229=CARTESIAN_POINT('Ctrl Pts',(4.84439326931296,-4.7285029573402,26.4510308802031));
#15230=CARTESIAN_POINT('Ctrl Pts',(4.97060959434682,-4.59187644221699,26.4597802236495));
#15231=CARTESIAN_POINT('Ctrl Pts',(5.09682496280503,-4.45525096256678,26.4685295007858));
#15232=CARTESIAN_POINT('Ctrl Pts',(5.2174039761583,-4.31341878218337,26.4772787779221));
#15233=CARTESIAN_POINT('Ctrl Pts',(5.33193710451928,-4.16686161438684,26.4860280550584));
#15234=CARTESIAN_POINT('Ctrl Pts',(5.44646940289381,-4.02030550864517,26.4947772687913));
#15235=CARTESIAN_POINT('Ctrl Pts',(5.55495572749666,-3.86902470980132,26.5035264825243));
#15236=CARTESIAN_POINT('Ctrl Pts',(5.65702762491459,-3.71353301465776,26.5122756962572));
#15237=CARTESIAN_POINT('Ctrl Pts',(5.75909881655154,-3.55804239466892,26.5210248494934));
#15238=CARTESIAN_POINT('Ctrl Pts',(5.8547555125078,-3.39834117619557,26.5297740027295));
#15239=CARTESIAN_POINT('Ctrl Pts',(5.9436728372809,-3.23497174691978,26.5385231559656));
#15240=CARTESIAN_POINT('Ctrl Pts',(6.032589576763,-3.07160339300987,26.5472722516111));
#15241=CARTESIAN_POINT('Ctrl Pts',(6.11476689685268,-2.90456712829538,26.5560213472566));
#15242=CARTESIAN_POINT('Ctrl Pts',(6.1899257052524,-2.73443024475952,26.5647704429022));
#15243=CARTESIAN_POINT('Ctrl Pts',(6.26508404388683,-2.56429442463065,26.5735194838632));
#15244=CARTESIAN_POINT('Ctrl Pts',(6.33322384283307,-2.39105828656015,26.5822685248242));
#15245=CARTESIAN_POINT('Ctrl Pts',(6.3941136872003,-2.2153101713209,26.5910175657853));
#15246=CARTESIAN_POINT('Ctrl Pts',(6.45500317120886,-2.03956309619526,26.5997665549677));
#15247=CARTESIAN_POINT('Ctrl Pts',(6.50864269270069,-1.86130434438647,26.6085155441501));
#15248=CARTESIAN_POINT('Ctrl Pts',(6.55485008446329,-1.6811393071996,26.6172645333325));
#15249=CARTESIAN_POINT('Ctrl Pts',(6.601996647494,-1.49731239211855,26.6261913468618));
#15250=CARTESIAN_POINT('Ctrl Pts',(6.64140563640904,-1.31150116499687,26.6351181603912));
#15251=CARTESIAN_POINT('Ctrl Pts',(6.6729377228217,-1.12436255155675,26.6440449739206));
#15252=CARTESIAN_POINT('Ctrl Pts',(6.70384494949869,-0.940932395051482,
26.6527948880761));
#15253=CARTESIAN_POINT('Ctrl Pts',(6.72718449348929,-0.756227260506838,
26.6615448022316));
#15254=CARTESIAN_POINT('Ctrl Pts',(6.74287707373931,-0.5708745645418,26.6702947163872));
#15255=CARTESIAN_POINT('Ctrl Pts',(6.75856934538669,-0.385525513632588,
26.6790444584711));
#15256=CARTESIAN_POINT('Ctrl Pts',(6.76661493004103,-0.199529212418346,
26.6877942005551));
#15257=CARTESIAN_POINT('Ctrl Pts',(6.76698649908907,-0.0135174386005491,
26.6965439426391));
#15258=CARTESIAN_POINT('Ctrl Pts',(6.7673580613239,0.172490924445683,26.705293524285));
#15259=CARTESIAN_POINT('Ctrl Pts',(6.7600558889629,0.358514472901337,26.7140431059309));
#15260=CARTESIAN_POINT('Ctrl Pts',(6.74510478454585,0.543921359662168,26.7227926875768));
#15261=CARTESIAN_POINT('Ctrl Pts',(6.73015393440688,0.729325093150405,26.7315421204158));
#15262=CARTESIAN_POINT('Ctrl Pts',(6.70755443556898,0.914111900256317,26.7402915532549));
#15263=CARTESIAN_POINT('Ctrl Pts',(6.67738304682319,1.09765415591535,26.7490409860939));
#15264=CARTESIAN_POINT('Ctrl Pts',(6.64721213111861,1.28119353391273,26.7577902817553));
#15265=CARTESIAN_POINT('Ctrl Pts',(6.60946960955494,1.46348811672655,26.7665395774166));
#15266=CARTESIAN_POINT('Ctrl Pts',(6.56428366991182,1.64391876348227,26.7752888730779));
#15267=CARTESIAN_POINT('Ctrl Pts',(6.51909837867718,1.82434682109713,26.7840380431887));
#15268=CARTESIAN_POINT('Ctrl Pts',(6.46646995271924,2.00291071820435,26.7927872132996));
#15269=CARTESIAN_POINT('Ctrl Pts',(6.40657713281555,2.17900400212687,26.8015363834104));
#15270=CARTESIAN_POINT('Ctrl Pts',(6.34668509279064,2.35509499309648,26.8102854395962));
#15271=CARTESIAN_POINT('Ctrl Pts',(6.27952894037528,2.52871516398118,26.8190344957819));
#15272=CARTESIAN_POINT('Ctrl Pts',(6.20533675061446,2.69927486771422,26.8277835519677));
#15273=CARTESIAN_POINT('Ctrl Pts',(6.12832117907917,2.87632521635922,26.83686555325));
#15274=CARTESIAN_POINT('Ctrl Pts',(6.04372366626082,3.05007728919992,26.8459475545322));
#15275=CARTESIAN_POINT('Ctrl Pts',(5.95185378007872,3.21989527478188,26.8550295558145));
#15276=CARTESIAN_POINT('Ctrl Pts',(5.86334450817376,3.38350129286744,26.8637793361216));
#15277=CARTESIAN_POINT('Ctrl Pts',(5.76808562057261,3.54345567124954,26.8725291164288));
#15278=CARTESIAN_POINT('Ctrl Pts',(5.66640068804489,3.69921508465301,26.8812788967359));
#15279=CARTESIAN_POINT('Ctrl Pts',(5.56471941107929,3.85496889852276,26.8900283624894));
#15280=CARTESIAN_POINT('Ctrl Pts',(5.45661270815119,4.0065278091963,26.8987778282429));
#15281=CARTESIAN_POINT('Ctrl Pts',(5.34244776449119,4.15337704569223,26.9075272939963));
#15282=CARTESIAN_POINT('Ctrl Pts',(5.22828631819598,4.30022178356246,26.9162764917159));
#15283=CARTESIAN_POINT('Ctrl Pts',(5.1080671784407,4.44235690972678,26.9250256894355));
#15284=CARTESIAN_POINT('Ctrl Pts',(4.98219864544718,4.57929969070646,26.9337748871551));
#15285=CARTESIAN_POINT('Ctrl Pts',(4.85633329944022,4.71623900430004,26.9425238633454));
#15286=CARTESIAN_POINT('Ctrl Pts',(4.72481904033643,4.84798602483622,26.9512728395356));
#15287=CARTESIAN_POINT('Ctrl Pts',(4.58810250737191,4.97409332259132,26.9600218157258));
#15288=CARTESIAN_POINT('Ctrl Pts',(4.45137708685635,5.10020881822141,26.968771360662));
#15289=CARTESIAN_POINT('Ctrl Pts',(4.30944892636045,5.22068366307938,26.9775209055982));
#15290=CARTESIAN_POINT('Ctrl Pts',(4.16280009466656,5.33510865604855,26.9862704505344));
#15291=CARTESIAN_POINT('Ctrl Pts',(4.01615988348789,5.44952692272891,26.9950194811427));
#15292=CARTESIAN_POINT('Ctrl Pts',(3.86479978232237,5.55789587288621,27.0037685117509));
#15293=CARTESIAN_POINT('Ctrl Pts',(3.7092338358108,5.65984746713869,27.0125175423592));
#15294=CARTESIAN_POINT('Ctrl Pts',(3.5536657779955,5.76180044505377,27.0212666917072));
#15295=CARTESIAN_POINT('Ctrl Pts',(3.39389200026846,5.85733573571056,27.0300158410552));
#15296=CARTESIAN_POINT('Ctrl Pts',(3.23045513626044,5.94612887621926,27.0387649904033));
#15297=CARTESIAN_POINT('Ctrl Pts',(3.18695122151581,5.96976399206687,27.0410938545162));
#15298=CARTESIAN_POINT('Ctrl Pts',(3.14318791262666,5.99292165435332,27.0434227186292));
#15299=CARTESIAN_POINT('Ctrl Pts',(3.09917575053259,6.01559628526639,27.0457515827422));
#15300=CARTESIAN_POINT('Ctrl Pts',(3.09917575053259,6.01559628526639,25.045602228898));
#15301=CARTESIAN_POINT('Ctrl Pts',(2.94396618243902,6.09555872072177,25.0538143435959));
#15302=CARTESIAN_POINT('Ctrl Pts',(2.78578041257525,6.16944837392768,25.0620264582939));
#15303=CARTESIAN_POINT('Ctrl Pts',(2.62514014159034,6.23706086526427,25.0702385729919));
#15304=CARTESIAN_POINT('Ctrl Pts',(2.46426588794036,6.30477183844988,25.0784626491517));
#15305=CARTESIAN_POINT('Ctrl Pts',(2.30093032461335,6.36618725259255,25.0866867253116));
#15306=CARTESIAN_POINT('Ctrl Pts',(2.1356718718031,6.4211521283948,25.0949108014715));
#15307=CARTESIAN_POINT('Ctrl Pts',(1.99267554601726,6.46871263228031,25.1020270043274));
#15308=CARTESIAN_POINT('Ctrl Pts',(1.84823986788398,6.51144423155273,25.1091432071833));
#15309=CARTESIAN_POINT('Ctrl Pts',(1.70271931047384,6.54927751356892,25.1162594100391));
#15310=CARTESIAN_POINT('Ctrl Pts',(1.53603835808051,6.59261219830938,25.1244103922134));
#15311=CARTESIAN_POINT('Ctrl Pts',(1.36744016728447,6.62964768602582,25.1325613743877));
#15312=CARTESIAN_POINT('Ctrl Pts',(1.19744625096259,6.66021106843136,25.140712356562));
#15313=CARTESIAN_POINT('Ctrl Pts',(1.02764979832998,6.69073894863555,25.148853870615));
#15314=CARTESIAN_POINT('Ctrl Pts',(0.856461203662327,6.71480962453299,25.1569953846681));
#15315=CARTESIAN_POINT('Ctrl Pts',(0.684417091352962,6.73229992239383,25.1651368987211));
#15316=CARTESIAN_POINT('Ctrl Pts',(0.51253661983395,6.74977358425285,25.1732706689242));
#15317=CARTESIAN_POINT('Ctrl Pts',(0.339802612011201,6.76067929202203,25.1814044391272));
#15318=CARTESIAN_POINT('Ctrl Pts',(0.166761838490786,6.76494489920082,25.1895382093303));
#15319=CARTESIAN_POINT('Ctrl Pts',(-0.00615074029530097,6.76920734626672,
25.1976659537483));
#15320=CARTESIAN_POINT('Ctrl Pts',(-0.179369268211578,6.76683947870447,
25.2057936981662));
#15321=CARTESIAN_POINT('Ctrl Pts',(-0.352341899948757,6.75782096430059,
25.2139214425842));
#15322=CARTESIAN_POINT('Ctrl Pts',(-0.525222753625955,6.74880723505692,
25.2220448744783));
#15323=CARTESIAN_POINT('Ctrl Pts',(-0.697857606560665,6.7331499056229,25.2301683063723));
#15324=CARTESIAN_POINT('Ctrl Pts',(-0.869694664559225,6.71088073135242,
25.2382917382664));
#15325=CARTESIAN_POINT('Ctrl Pts',(-1.04262178926545,6.68847029019945,25.2464667020172));
#15326=CARTESIAN_POINT('Ctrl Pts',(-1.21474058701269,6.65936382531185,25.254641665768));
#15327=CARTESIAN_POINT('Ctrl Pts',(-1.38549346493782,6.6236467945245,25.2628166295188));
#15328=CARTESIAN_POINT('Ctrl Pts',(-1.55513149232127,6.58816296127738,25.2709382186919));
#15329=CARTESIAN_POINT('Ctrl Pts',(-1.72342102622658,6.54615472808624,25.2790598078649));
#15330=CARTESIAN_POINT('Ctrl Pts',(-1.88982546590237,6.49775720602324,25.2871813970379));
#15331=CARTESIAN_POINT('Ctrl Pts',(-2.05625187437702,6.44935329449473,25.2953040584273));
#15332=CARTESIAN_POINT('Ctrl Pts',(-2.22079234145552,6.39455851617661,25.3034267198166));
#15333=CARTESIAN_POINT('Ctrl Pts',(-2.38292549598552,6.33355785325927,25.311549381206));
#15334=CARTESIAN_POINT('Ctrl Pts',(-2.54511093036561,6.27253752067276,25.3196746617483));
#15335=CARTESIAN_POINT('Ctrl Pts',(-2.70488716410205,6.20530744751755,25.3277999422905));
#15336=CARTESIAN_POINT('Ctrl Pts',(-2.86175291536794,6.13210072090985,25.3359252228328));
#15337=CARTESIAN_POINT('Ctrl Pts',(-3.02032768644431,6.05809642220611,25.3441390266205));
#15338=CARTESIAN_POINT('Ctrl Pts',(-3.17592783722615,5.97798464071692,25.3523528304083));
#15339=CARTESIAN_POINT('Ctrl Pts',(-3.32806199135273,5.89205332475134,25.3605666341961));
#15340=CARTESIAN_POINT('Ctrl Pts',(-3.4788169604441,5.80690102639503,25.3687059750512));
#15341=CARTESIAN_POINT('Ctrl Pts',(-3.62616824026076,5.71603452094295,25.3768453159064));
#15342=CARTESIAN_POINT('Ctrl Pts',(-3.76966808797646,5.61977681998955,25.3849846567616));
#15343=CARTESIAN_POINT('Ctrl Pts',(-3.91513715279711,5.52219819560511,25.3932356920156));
#15344=CARTESIAN_POINT('Ctrl Pts',(-4.05664799702019,5.41907956952353,25.4014867272697));
#15345=CARTESIAN_POINT('Ctrl Pts',(-4.19377033464324,5.31079837503424,25.4097377625238));
#15346=CARTESIAN_POINT('Ctrl Pts',(-4.33089267226627,5.20251718054497,25.4179887977779));
#15347=CARTESIAN_POINT('Ctrl Pts',(-4.46362625504326,5.0890737180381,25.4262398330319));
#15348=CARTESIAN_POINT('Ctrl Pts',(-4.59158115548176,4.97088236559917,25.434490868286));
#15349=CARTESIAN_POINT('Ctrl Pts',(-4.71781145313423,4.85428402081374,25.4426306943692));
#15350=CARTESIAN_POINT('Ctrl Pts',(-4.83980275031117,4.73268470718957,25.4507705204524));
#15351=CARTESIAN_POINT('Ctrl Pts',(-4.95712802364735,4.60642711406249,25.4589103465356));
#15352=CARTESIAN_POINT('Ctrl Pts',(-5.07431167281898,4.48032192736615,25.4670403469773));
#15353=CARTESIAN_POINT('Ctrl Pts',(-5.18684026234713,4.3495699206802,25.4751703474191));
#15354=CARTESIAN_POINT('Ctrl Pts',(-5.29432033801962,4.21455349455098,25.4833003478608));
#15355=CARTESIAN_POINT('Ctrl Pts',(-5.40169352152022,4.07967134632338,25.4914222627723));
#15356=CARTESIAN_POINT('Ctrl Pts',(-5.50402796004642,3.9405335077515,25.4995441776838));
#15357=CARTESIAN_POINT('Ctrl Pts',(-5.60096756501489,3.79755860200356,25.5076660925953));
#15358=CARTESIAN_POINT('Ctrl Pts',(-5.69782189370204,3.65470946908383,25.515780862783));
#15359=CARTESIAN_POINT('Ctrl Pts',(-5.78929063807354,3.5080302962892,25.5238956329707));
#15360=CARTESIAN_POINT('Ctrl Pts',(-5.8750585907684,3.35797194077593,25.5320104031585));
#15361=CARTESIAN_POINT('Ctrl Pts',(-5.96078454882321,3.20798705847063,25.5401212001039));
#15362=CARTESIAN_POINT('Ctrl Pts',(-6.04081508903707,3.05462660479748,25.5482319970494));
#15363=CARTESIAN_POINT('Ctrl Pts',(-6.11487873275084,2.89836972861496,25.5563427939948));
#15364=CARTESIAN_POINT('Ctrl Pts',(-6.18892035088505,2.74215932122717,25.5644511788931));
#15365=CARTESIAN_POINT('Ctrl Pts',(-6.25699844812174,2.58305453792936,25.5725595637914));
#15366=CARTESIAN_POINT('Ctrl Pts',(-6.31888789351101,2.42155833901229,25.5806679486897));
#15367=CARTESIAN_POINT('Ctrl Pts',(-6.38077083111304,2.26007912171298,25.5887754809766));
#15368=CARTESIAN_POINT('Ctrl Pts',(-6.43646628214497,2.09620933294143,25.5968830132635));
#15369=CARTESIAN_POINT('Ctrl Pts',(-6.48579761055905,1.93047101891392,25.6049905455504));
#15370=CARTESIAN_POINT('Ctrl Pts',(-6.53515040741879,1.76466057741481,25.6131016061453));
#15371=CARTESIAN_POINT('Ctrl Pts',(-6.57813344044233,1.5969803377804,25.6212126667401));
#15372=CARTESIAN_POINT('Ctrl Pts',(-6.61462009762341,1.42796707389088,25.6293237273349));
#15373=CARTESIAN_POINT('Ctrl Pts',(-6.65111460209694,1.25891745982261,25.6374365323994));
#15374=CARTESIAN_POINT('Ctrl Pts',(-6.68110987827748,1.0885346114493,25.6455493374638));
#15375=CARTESIAN_POINT('Ctrl Pts',(-6.70453068608186,0.917364311158205,
25.6536621425283));
#15376=CARTESIAN_POINT('Ctrl Pts',(-6.72797283468183,0.746038042276231,
25.661782339896));
#15377=CARTESIAN_POINT('Ctrl Pts',(-6.74482850646066,0.573923253531824,
25.6699025372637));
#15378=CARTESIAN_POINT('Ctrl Pts',(-6.75507440440881,0.401570405907753,
25.6780227346314));
#15379=CARTESIAN_POINT('Ctrl Pts',(-6.76302860803167,0.267767624353762,
25.6843266919466));
#15380=CARTESIAN_POINT('Ctrl Pts',(-6.76700022310181,0.133821483113563,
25.6906306492618));
#15381=CARTESIAN_POINT('Ctrl Pts',(-6.7669999999906,-1.12811956310505E-5,
25.6969346065769));
#15382=CARTESIAN_POINT('',(-6.76699880620097,-0.00401956150071273,25.3028202162185));
#15383=CARTESIAN_POINT('Ctrl Pts',(3.0991757505326,6.01559628526638,24.6513135168612));
#15384=CARTESIAN_POINT('Ctrl Pts',(2.94375327653849,6.09566840773745,24.6595164746245));
#15385=CARTESIAN_POINT('Ctrl Pts',(2.78526591770003,6.16969254101118,24.6677194323877));
#15386=CARTESIAN_POINT('Ctrl Pts',(2.62422874726044,6.23744438709091,24.675922390151));
#15387=CARTESIAN_POINT('Ctrl Pts',(2.46312443454218,6.30522448139009,24.684128768027));
#15388=CARTESIAN_POINT('Ctrl Pts',(2.29946852245279,6.36672694014881,24.692335145903));
#15389=CARTESIAN_POINT('Ctrl Pts',(2.1337942026006,6.42177633532561,24.700541523779));
#15390=CARTESIAN_POINT('Ctrl Pts',(1.96792736579282,6.476889699028,24.7087574376343));
#15391=CARTESIAN_POINT('Ctrl Pts',(1.80003777664869,6.52553490838256,24.7169733514896));
#15392=CARTESIAN_POINT('Ctrl Pts',(1.63067283231014,6.56758670395493,24.7251892653449));
#15393=CARTESIAN_POINT('Ctrl Pts',(1.46119849244701,6.60966566145421,24.7334104859903));
#15394=CARTESIAN_POINT('Ctrl Pts',(1.29024724786503,6.64514264390263,24.7416317066357));
#15395=CARTESIAN_POINT('Ctrl Pts',(1.11837460373133,6.67394390489827,24.7498529272811));
#15396=CARTESIAN_POINT('Ctrl Pts',(0.946251757426406,6.70278709308991,24.7580861159));
#15397=CARTESIAN_POINT('Ctrl Pts',(0.773205186618674,6.72493510158126,24.7663193045189));
#15398=CARTESIAN_POINT('Ctrl Pts',(0.599794505029058,6.7403661289085,24.7745524931378));
#15399=CARTESIAN_POINT('Ctrl Pts',(0.500854736219013,6.74917032863982,24.779249953358));
#15400=CARTESIAN_POINT('Ctrl Pts',(0.401796439857815,6.75578891228401,24.7839474135782));
#15401=CARTESIAN_POINT('Ctrl Pts',(0.302723114336111,6.7602254190261,24.7886448737984));
#15402=CARTESIAN_POINT('Ctrl Pts',(0.130717743851077,6.76792782511588,24.7968003322052));
#15403=CARTESIAN_POINT('Ctrl Pts',(-0.0418623406125811,6.76907382164679,
24.804955790612));
#15404=CARTESIAN_POINT('Ctrl Pts',(-0.214471438378831,6.76360044666446,
24.8131112490188));
#15405=CARTESIAN_POINT('Ctrl Pts',(-0.386870448183795,6.75813373349896,
24.8212567811607));
#15406=CARTESIAN_POINT('Ctrl Pts',(-0.559298039694058,6.74606369739774,
24.8294023133026));
#15407=CARTESIAN_POINT('Ctrl Pts',(-0.731203809171472,6.72737913228124,
24.8375478454444));
#15408=CARTESIAN_POINT('Ctrl Pts',(-0.90293649506536,6.70871337974735,24.845685176245));
#15409=CARTESIAN_POINT('Ctrl Pts',(-1.07414804425433,6.68344639597504,24.8538225070455));
#15410=CARTESIAN_POINT('Ctrl Pts',(-1.24428847192027,6.65161899079061,24.8619598378461));
#15411=CARTESIAN_POINT('Ctrl Pts',(-1.41429334897801,6.61981694244929,24.8700906856481));
#15412=CARTESIAN_POINT('Ctrl Pts',(-1.58322844606182,6.58146494655465,24.8782215334501));
#15413=CARTESIAN_POINT('Ctrl Pts',(-1.75054932089481,6.53665557262387,24.8863523812522));
#15414=CARTESIAN_POINT('Ctrl Pts',(-1.91777204009729,6.49187248526586,24.8944784592459));
#15415=CARTESIAN_POINT('Ctrl Pts',(-2.08338207071149,6.44063965811015,24.9026045372397));
#15416=CARTESIAN_POINT('Ctrl Pts',(-2.24684558583775,6.38310065042072,24.9107306152335));
#15417=CARTESIAN_POINT('Ctrl Pts',(-2.41088871273391,6.32535761991887,24.9188855068157));
#15418=CARTESIAN_POINT('Ctrl Pts',(-2.57276970953988,6.26126368008906,24.9270403983979));
#15419=CARTESIAN_POINT('Ctrl Pts',(-2.73196424635951,6.19101448525307,24.9351952899801));
#15420=CARTESIAN_POINT('Ctrl Pts',(-2.89053798014637,6.12103923771499,24.9433183803364));
#15421=CARTESIAN_POINT('Ctrl Pts',(-3.0464458387807,6.04495682005173,24.9514414706927));
#15422=CARTESIAN_POINT('Ctrl Pts',(-3.19918981210989,5.96300876622635,24.959564561049));
#15423=CARTESIAN_POINT('Ctrl Pts',(-3.35194577959302,5.88105427746576,24.9676882892674));
#15424=CARTESIAN_POINT('Ctrl Pts',(-3.50153704451353,5.79323340800121,24.9758120174858));
#15425=CARTESIAN_POINT('Ctrl Pts',(-3.64749060145182,5.69983344601583,24.9839357457043));
#15426=CARTESIAN_POINT('Ctrl Pts',(-3.79348338682098,5.60640838060694,24.9920616573646));
#15427=CARTESIAN_POINT('Ctrl Pts',(-3.93583620938079,5.50740143397097,25.0001875690249));
#15428=CARTESIAN_POINT('Ctrl Pts',(-4.07410546947808,5.40314293939822,25.0083134806852));
#15429=CARTESIAN_POINT('Ctrl Pts',(-4.21325897586662,5.29821770091512,25.0164913583953));
#15430=CARTESIAN_POINT('Ctrl Pts',(-4.34827620899244,5.18797373909642,25.0246692361054));
#15431=CARTESIAN_POINT('Ctrl Pts',(-4.47873984375709,5.07278803144215,25.0328471138155));
#15432=CARTESIAN_POINT('Ctrl Pts',(-4.6085808038887,4.95815208018838,25.0409859602889));
#15433=CARTESIAN_POINT('Ctrl Pts',(-4.73391131479579,4.83862174851114,25.0491248067623));
#15434=CARTESIAN_POINT('Ctrl Pts',(-4.85435825669402,4.714604428334,25.0572636532357));
#15435=CARTESIAN_POINT('Ctrl Pts',(-4.97567163459911,4.58969498860628,25.0654610465641));
#15436=CARTESIAN_POINT('Ctrl Pts',(-5.09203066609562,4.46023404357679,25.0736584398925));
#15437=CARTESIAN_POINT('Ctrl Pts',(-5.20309674407,4.32666999802946,25.0818558332209));
#15438=CARTESIAN_POINT('Ctrl Pts',(-5.31416282204437,4.19310595248212,25.0900532265493));
#15439=CARTESIAN_POINT('Ctrl Pts',(-5.41993576816953,4.05543913881916,25.0982506198777));
#15440=CARTESIAN_POINT('Ctrl Pts',(-5.52012270626552,3.91414541219049,25.1064480132061));
#15441=CARTESIAN_POINT('Ctrl Pts',(-5.62195064967377,3.7705373743313,25.1147796751952));
#15442=CARTESIAN_POINT('Ctrl Pts',(-5.71830642439719,3.62276230979212,25.1231113371843));
#15443=CARTESIAN_POINT('Ctrl Pts',(-5.80883672877185,3.47126847974501,25.1314429991735));
#15444=CARTESIAN_POINT('Ctrl Pts',(-5.89926017322852,3.31995346957887,25.1397648266577));
#15445=CARTESIAN_POINT('Ctrl Pts',(-5.98387166682184,3.16492873101086,25.148086654142));
#15446=CARTESIAN_POINT('Ctrl Pts',(-6.06235947374681,3.00667367884716,25.1564084816262));
#15447=CARTESIAN_POINT('Ctrl Pts',(-6.14076752079736,2.84857944660672,25.1647218524095));
#15448=CARTESIAN_POINT('Ctrl Pts',(-6.21306412428561,2.68726174791271,25.1730352231928));
#15449=CARTESIAN_POINT('Ctrl Pts',(-6.27898191581495,2.52322712034981,25.181348593976));
#15450=CARTESIAN_POINT('Ctrl Pts',(-6.34484353585997,2.35933227399465,25.189654880566));
#15451=CARTESIAN_POINT('Ctrl Pts',(-6.40433704480477,2.19272543122517,25.197961167156));
#15452=CARTESIAN_POINT('Ctrl Pts',(-6.45724184116955,2.02393596851515,25.206267453746));
#15453=CARTESIAN_POINT('Ctrl Pts',(-6.51010470651423,1.85528028411708,25.2145671569807));
#15454=CARTESIAN_POINT('Ctrl Pts',(-6.55638916665807,1.68444575796112,25.2228668602154));
#15455=CARTESIAN_POINT('Ctrl Pts',(-6.59592341309155,1.5119799365834,25.2311665634501));
#15456=CARTESIAN_POINT('Ctrl Pts',(-6.6354389109427,1.33959590479173,25.2394623306626));
#15457=CARTESIAN_POINT('Ctrl Pts',(-6.66821049592097,1.16558245606088,25.2477580978752));
#15458=CARTESIAN_POINT('Ctrl Pts',(-6.69411659456468,0.99050089266686,25.2560538650878));
#15459=CARTESIAN_POINT('Ctrl Pts',(-6.72001635095464,0.815462192218633,
25.2643476013554));
#15460=CARTESIAN_POINT('Ctrl Pts',(-6.73905391639905,0.639356240041771,
25.272641337623));
#15461=CARTESIAN_POINT('Ctrl Pts',(-6.75115903176224,0.462753420144147,
25.2809350738906));
#15462=CARTESIAN_POINT('Ctrl Pts',(-6.76180651172889,0.307416198606293,
25.2882301213237));
#15463=CARTESIAN_POINT('Ctrl Pts',(-6.76709129972569,0.15169485322347,25.2955251687568));
#15464=CARTESIAN_POINT('Ctrl Pts',(-6.76699880620133,-0.00401956088942276,
25.3028202161899));
#15465=CARTESIAN_POINT('Ctrl Pts',(-6.76699880620097,-0.00401956150070087,
25.3028202162186));
#15466=CARTESIAN_POINT('Ctrl Pts',(-6.76688334084871,-0.198407407234547,
25.3119270709894));
#15467=CARTESIAN_POINT('Ctrl Pts',(-6.75838791804712,-0.392497961171036,
25.3210339257603));
#15468=CARTESIAN_POINT('Ctrl Pts',(-6.74161346978387,-0.585608080569804,
25.3301407805311));
#15469=CARTESIAN_POINT('Ctrl Pts',(-6.72474577620206,-0.7797916549233,25.3392982582233));
#15470=CARTESIAN_POINT('Ctrl Pts',(-6.69950683604764,-0.972983664605142,
25.3484557359154));
#15471=CARTESIAN_POINT('Ctrl Pts',(-6.66604947769159,-1.16450562942723,
25.3576132136076));
#15472=CARTESIAN_POINT('Ctrl Pts',(-6.63249811463724,-1.35656571098672,
25.366796420944));
#15473=CARTESIAN_POINT('Ctrl Pts',(-6.59068219033038,-1.54694616423987,
25.3759796282803));
#15474=CARTESIAN_POINT('Ctrl Pts',(-6.54080477051408,-1.73498183103464,
25.3851628356167));
#15475=CARTESIAN_POINT('Ctrl Pts',(-6.49074514784345,-1.92370439453197,
25.3943795893273));
#15476=CARTESIAN_POINT('Ctrl Pts',(-6.43256512569696,-2.11006482645954,
25.4035963430379));
#15477=CARTESIAN_POINT('Ctrl Pts',(-6.36651770178052,-2.29341259979867,
25.4128130967484));
#15478=CARTESIAN_POINT('Ctrl Pts',(-6.33919592999244,-2.36925788980367,
25.4166257820369));
#15479=CARTESIAN_POINT('Ctrl Pts',(-6.31052842599154,-2.44458792191119,
25.4204384673254));
#15480=CARTESIAN_POINT('Ctrl Pts',(-6.2805354090269,-2.51935784992116,25.4242511526138));
#15481=CARTESIAN_POINT('Ctrl Pts',(-6.21582285919771,-2.68068049038025,
25.4324773536327));
#15482=CARTESIAN_POINT('Ctrl Pts',(-6.14480023546957,-2.83973368865429,
25.4407035546515));
#15483=CARTESIAN_POINT('Ctrl Pts',(-6.06764690463886,-2.99598899207365,
25.4489297556703));
#15484=CARTESIAN_POINT('Ctrl Pts',(-5.99058023931446,-3.15206877559208,
25.4571467162861));
#15485=CARTESIAN_POINT('Ctrl Pts',(-5.90739673723445,-3.30535660386273,
25.4653636769019));
#15486=CARTESIAN_POINT('Ctrl Pts',(-5.81832453226442,-3.45534204345244,
25.4735806375176));
#15487=CARTESIAN_POINT('Ctrl Pts',(-5.72933450364474,-3.60518910928082,
25.4817900173192));
#15488=CARTESIAN_POINT('Ctrl Pts',(-5.63446677374864,-3.75173954766778,
25.4899993971208));
#15489=CARTESIAN_POINT('Ctrl Pts',(-5.53399631125849,-3.89450559467789,
25.4982087769224));
#15490=CARTESIAN_POINT('Ctrl Pts',(-5.43359838218822,-4.03716857348891,
25.5064122300627));
#15491=CARTESIAN_POINT('Ctrl Pts',(-5.32760598268406,-4.17605231068577,
25.5146156832031));
#15492=CARTESIAN_POINT('Ctrl Pts',(-5.21633853458503,-4.31069614941755,
25.5228191363435));
#15493=CARTESIAN_POINT('Ctrl Pts',(-5.10512909468399,-4.44526979289827,
25.5310183126936));
#15494=CARTESIAN_POINT('Ctrl Pts',(-4.98865031278193,-4.5756076656865,25.5392174890438));
#15495=CARTESIAN_POINT('Ctrl Pts',(-4.86726325624927,-4.70128039946202,
25.547416665394));
#15496=CARTESIAN_POINT('Ctrl Pts',(-4.74589904052343,-4.82692948601586,
25.5556142989453));
#15497=CARTESIAN_POINT('Ctrl Pts',(-4.61962863423834,-4.94791492006309,
25.5638119324967));
#15498=CARTESIAN_POINT('Ctrl Pts',(-4.48885170573719,-5.06384235180168,
25.5720095660481));
#15499=CARTESIAN_POINT('Ctrl Pts',(-4.35808419638442,-5.17976143392009,
25.5802066091687));
#15500=CARTESIAN_POINT('Ctrl Pts',(-4.22281107905283,-5.29062300066486,
25.5884036522892));
#15501=CARTESIAN_POINT('Ctrl Pts',(-4.08346697035957,-5.39607139518951,
25.5966006954098));
#15502=CARTESIAN_POINT('Ctrl Pts',(-3.94410757230295,-5.50153135991139,
25.604798637941));
#15503=CARTESIAN_POINT('Ctrl Pts',(-3.80067657903412,-5.6015767525989,25.6129965804722));
#15504=CARTESIAN_POINT('Ctrl Pts',(-3.6536396315922,-5.69589382296219,25.6211945230034));
#15505=CARTESIAN_POINT('Ctrl Pts',(-3.50655982687992,-5.7902383841858,25.6293948550118));
#15506=CARTESIAN_POINT('Ctrl Pts',(-3.35587227628556,-5.87885110373377,
25.6375951870202));
#15507=CARTESIAN_POINT('Ctrl Pts',(-3.20206942024186,-5.96146294360302,
25.6457955190286));
#15508=CARTESIAN_POINT('Ctrl Pts',(-3.0481062600525,-6.04416088733765,25.6540043979994));
#15509=CARTESIAN_POINT('Ctrl Pts',(-2.89102162381837,-6.12084528582415,
25.6622132769702));
#15510=CARTESIAN_POINT('Ctrl Pts',(-2.73133115216674,-6.19129381770915,
25.6704221559409));
#15511=CARTESIAN_POINT('Ctrl Pts',(-2.57155495496598,-6.26178016800009,
25.6786354416283));
#15512=CARTESIAN_POINT('Ctrl Pts',(-2.40917046684931,-6.32602384639378,
25.6868487273157));
#15513=CARTESIAN_POINT('Ctrl Pts',(-2.24471079528138,-6.38385169357397,
25.6950620130031));
#15514=CARTESIAN_POINT('Ctrl Pts',(-2.0800105394831,-6.44176413576747,25.7032873137152));
#15515=CARTESIAN_POINT('Ctrl Pts',(-1.91322937621344,-6.49324188452043,
25.7115126144273));
#15516=CARTESIAN_POINT('Ctrl Pts',(-1.74491421651305,-6.53816207943874,
25.7197379151393));
#15517=CARTESIAN_POINT('Ctrl Pts',(-1.59269345805365,-6.57878697711747,
25.7271767074334));
#15518=CARTESIAN_POINT('Ctrl Pts',(-1.43921837185263,-6.61404906212829,
25.7346154997274));
#15519=CARTESIAN_POINT('Ctrl Pts',(-1.28489791656797,-6.64389391426438,
25.7420542920215));
#15520=CARTESIAN_POINT('Ctrl Pts',(-1.11577016883261,-6.67660242729955,
25.7502068482347));
#15521=CARTESIAN_POINT('Ctrl Pts',(-0.945128120729877,-6.70289988064057,
25.758359404448));
#15522=CARTESIAN_POINT('Ctrl Pts',(-0.773503444533528,-6.72264690589166,
25.7665119606613));
#15523=CARTESIAN_POINT('Ctrl Pts',(-0.60207759966208,-6.74237105373794,
25.7746550719416));
#15524=CARTESIAN_POINT('Ctrl Pts',(-0.429671752241763,-6.75555983842487,
25.7827981832219));
#15525=CARTESIAN_POINT('Ctrl Pts',(-0.2568294814744,-6.76212448993995,25.7909412945023));
#15526=CARTESIAN_POINT('Ctrl Pts',(-0.0841511147097744,-6.76868291628421,
25.7990766837796));
#15527=CARTESIAN_POINT('Ctrl Pts',(0.088962488684636,-6.76862970149317,
25.807212073057));
#15528=CARTESIAN_POINT('Ctrl Pts',(0.261960878240891,-6.7619276466309,25.8153474623343));
#15529=CARTESIAN_POINT('Ctrl Pts',(0.434831566884902,-6.75523053897376,
25.8234768463729));
#15530=CARTESIAN_POINT('Ctrl Pts',(0.60758684728569,-6.74189437787547,25.8316062304115));
#15531=CARTESIAN_POINT('Ctrl Pts',(0.779674507005852,-6.72193399723065,
25.8397356144501));
#15532=CARTESIAN_POINT('Ctrl Pts',(0.951671284719478,-6.70198415795438,
25.8478607052422));
#15533=CARTESIAN_POINT('Ctrl Pts',(1.12300078161399,-6.6754171082616,25.8559857960344));
#15534=CARTESIAN_POINT('Ctrl Pts',(1.29311415397371,-6.64229966086994,25.8641108868265));
#15535=CARTESIAN_POINT('Ctrl Pts',(1.46387688595396,-6.60905579700217,25.8722669928516));
#15536=CARTESIAN_POINT('Ctrl Pts',(1.6334138190361,-6.56921145038738,25.8804230988767));
#15537=CARTESIAN_POINT('Ctrl Pts',(1.80117786754283,-6.52288642316221,25.8885792049018));
#15538=CARTESIAN_POINT('Ctrl Pts',(1.96826669609484,-6.47674784579363,25.8967024840752));
#15539=CARTESIAN_POINT('Ctrl Pts',(2.13359653534583,-6.42418077690206,25.9048257632487));
#15540=CARTESIAN_POINT('Ctrl Pts',(2.29664024127731,-6.36535408301422,25.9129490424221));
#15541=CARTESIAN_POINT('Ctrl Pts',(2.45970565785597,-6.30651955585499,25.9210734032787));
#15542=CARTESIAN_POINT('Ctrl Pts',(2.62048399062375,-6.24142386764794,25.9291977641354));
#15543=CARTESIAN_POINT('Ctrl Pts',(2.77846645275301,-6.17028469123801,25.9373221249921));
#15544=CARTESIAN_POINT('Ctrl Pts',(2.93650000855845,-6.09912250745122,25.9454491133775));
#15545=CARTESIAN_POINT('Ctrl Pts',(3.09173555973837,-6.02191309346784,25.9535761017629));
#15546=CARTESIAN_POINT('Ctrl Pts',(3.2436874127479,-5.9389208589087,25.9617030901484));
#15547=CARTESIAN_POINT('Ctrl Pts',(3.39662161718698,-5.85539208900204,25.9698826185884));
#15548=CARTESIAN_POINT('Ctrl Pts',(3.54622918895365,-5.76600564888686,25.9780621470285));
#15549=CARTESIAN_POINT('Ctrl Pts',(3.69204389825408,-5.67107581093436,25.9862416754686));
#15550=CARTESIAN_POINT('Ctrl Pts',(3.83717191907995,-5.57659302819273,25.9943826838722));
#15551=CARTESIAN_POINT('Ctrl Pts',(3.97854246301319,-5.47661921000716,26.0025236922759));
#15552=CARTESIAN_POINT('Ctrl Pts',(4.11572880697669,-5.37150494623455,26.0106647006796));
#15553=CARTESIAN_POINT('Ctrl Pts',(4.25388881833464,-5.26564464369182,26.0188634891379));
#15554=CARTESIAN_POINT('Ctrl Pts',(4.38780472688166,-5.15457090068877,26.0270622775961));
#15555=CARTESIAN_POINT('Ctrl Pts',(4.51707841398514,-5.03867954943649,26.0352610660544));
#15556=CARTESIAN_POINT('Ctrl Pts',(4.64635210108859,-4.92278819818424,26.0434598545126));
#15557=CARTESIAN_POINT('Ctrl Pts',(4.77098334505881,-4.80207954358236,26.0516586429709));
#15558=CARTESIAN_POINT('Ctrl Pts',(4.89061549714208,-4.67698290130654,26.0598574314291));
#15559=CARTESIAN_POINT('Ctrl Pts',(5.01074757647513,-4.55136349638505,26.0680904815612));
#15560=CARTESIAN_POINT('Ctrl Pts',(5.12621221717435,-4.42092894380504,26.0763235316931));
#15561=CARTESIAN_POINT('Ctrl Pts',(5.23660054380631,-4.28605923251271,26.0845565818252));
#15562=CARTESIAN_POINT('Ctrl Pts',(5.3468574149097,-4.15135013031492,26.09277982766));
#15563=CARTESIAN_POINT('Ctrl Pts',(5.45204978461543,-4.01221666081912,26.1010030734949));
#15564=CARTESIAN_POINT('Ctrl Pts',(5.55180512777695,-3.86907596503216,26.1092263193297));
#15565=CARTESIAN_POINT('Ctrl Pts',(5.65146164390596,-3.72607707789172,26.1174414184432));
#15566=CARTESIAN_POINT('Ctrl Pts',(5.7456916572478,-3.57907916247656,26.1256565175568));
#15567=CARTESIAN_POINT('Ctrl Pts',(5.83416244742233,-3.42853285489392,26.1338716166703));
#15568=CARTESIAN_POINT('Ctrl Pts',(5.92256329132739,-3.27810557137085,26.1420802208092));
#15569=CARTESIAN_POINT('Ctrl Pts',(6.00521380071724,-3.12413579091115,26.150288824948));
#15570=CARTESIAN_POINT('Ctrl Pts',(6.08182413774452,-2.96710366477954,26.1584974290869));
#15571=CARTESIAN_POINT('Ctrl Pts',(6.15838922974909,-2.81016427968508,26.1667011853359));
#15572=CARTESIAN_POINT('Ctrl Pts',(6.22892109919551,-2.65016647290736,26.1749049415849));
#15573=CARTESIAN_POINT('Ctrl Pts',(6.29317546179498,-2.48761564697233,26.1831086978339));
#15574=CARTESIAN_POINT('Ctrl Pts',(6.35741081314813,-2.32511291572949,26.1913100267981));
#15575=CARTESIAN_POINT('Ctrl Pts',(6.41537222234622,-2.16005900126699,26.1995113557624));
#15576=CARTESIAN_POINT('Ctrl Pts',(6.4668631434036,-1.99298020173009,26.2077126847267));
#15577=CARTESIAN_POINT('Ctrl Pts',(6.51834696337138,-1.82592444395474,26.2159128826494));
#15578=CARTESIAN_POINT('Ctrl Pts',(6.56336196618395,-1.65684469931315,26.2241130805721));
#15579=CARTESIAN_POINT('Ctrl Pts',(6.60176117856937,-1.48628339866069,26.2323132784949));
#15580=CARTESIAN_POINT('Ctrl Pts',(6.6401620540554,-1.31571471086187,26.2405138315747));
#15581=CARTESIAN_POINT('Ctrl Pts',(6.67194648951085,-1.14366468875732,26.2487143846546));
#15582=CARTESIAN_POINT('Ctrl Pts',(6.69701842085514,-0.970687009662231,
26.2569149377344));
#15583=CARTESIAN_POINT('Ctrl Pts',(6.7220959816099,-0.797670491821714,26.2651173320876));
#15584=CARTESIAN_POINT('Ctrl Pts',(6.7404579850306,-0.623726256647637,26.2733197264408));
#15585=CARTESIAN_POINT('Ctrl Pts',(6.75206011876615,-0.449414232715902,
26.281522120794));
#15586=CARTESIAN_POINT('Ctrl Pts',(6.76367310253629,-0.274939196399476,
26.2897321858279));
#15587=CARTESIAN_POINT('Ctrl Pts',(6.7685135626335,-0.100096042103787,26.2979422508617));
#15588=CARTESIAN_POINT('Ctrl Pts',(6.76658930469254,0.0745532133478711,
26.3061523158955));
#15589=CARTESIAN_POINT('Ctrl Pts',(6.76466412583587,0.249286052834895,26.3143663101209));
#15590=CARTESIAN_POINT('Ctrl Pts',(6.75596779176654,0.423824450814262,26.3225803043462));
#15591=CARTESIAN_POINT('Ctrl Pts',(6.74056012172359,0.597610446218733,26.3307942985715));
#15592=CARTESIAN_POINT('Ctrl Pts',(6.72513144589468,0.771633369816078,26.3390194912067));
#15593=CARTESIAN_POINT('Ctrl Pts',(6.70297319358434,0.944901485324106,26.3472446838419));
#15594=CARTESIAN_POINT('Ctrl Pts',(6.67419673939501,1.11686475629284,26.3554698764771));
#15595=CARTESIAN_POINT('Ctrl Pts',(6.64831813577658,1.27151095756032,26.362866774597));
#15596=CARTESIAN_POINT('Ctrl Pts',(6.6170878758833,1.42510184517037,26.3702636727169));
#15597=CARTESIAN_POINT('Ctrl Pts',(6.58062140342001,1.57724790215442,26.3776605708368));
#15598=CARTESIAN_POINT('Ctrl Pts',(6.53799706361612,1.75508592142644,26.3863065373277));
#15599=CARTESIAN_POINT('Ctrl Pts',(6.48812158297308,1.93135347881673,26.3949525038186));
#15600=CARTESIAN_POINT('Ctrl Pts',(6.43112442046256,2.10545189651299,26.4035984703095));
#15601=CARTESIAN_POINT('Ctrl Pts',(6.37420016507141,2.27932761866508,26.4122333774339));
#15602=CARTESIAN_POINT('Ctrl Pts',(6.31017248731797,2.45103944546087,26.4208682845582));
#15603=CARTESIAN_POINT('Ctrl Pts',(6.23922127964424,2.62000130221999,26.4295031916826));
#15604=CARTESIAN_POINT('Ctrl Pts',(6.16591454914174,2.79457255625137,26.4384247707541));
#15605=CARTESIAN_POINT('Ctrl Pts',(6.08521672373981,2.96620779021715,26.4473463498256));
#15606=CARTESIAN_POINT('Ctrl Pts',(5.99738234333584,3.13427727360608,26.4562679288971));
#15607=CARTESIAN_POINT('Ctrl Pts',(5.91260508320171,3.29649701316977,26.4648789878728));
#15608=CARTESIAN_POINT('Ctrl Pts',(5.8211798022406,3.45539470966287,26.4734900468485));
#15609=CARTESIAN_POINT('Ctrl Pts',(5.72338450147232,3.61042363834308,26.4821011058242));
#15610=CARTESIAN_POINT('Ctrl Pts',(5.62568142618739,3.76530636758661,26.4907040441737));
#15611=CARTESIAN_POINT('Ctrl Pts',(5.52162047009277,3.9163273459469,26.4993069825233));
#15612=CARTESIAN_POINT('Ctrl Pts',(5.41152528634193,4.06296481344373,26.5079099208728));
#15613=CARTESIAN_POINT('Ctrl Pts',(5.301553383728,4.20943808089938,26.5165032259216));
#15614=CARTESIAN_POINT('Ctrl Pts',(5.18556091607221,4.35153738649489,26.5250965309703));
#15615=CARTESIAN_POINT('Ctrl Pts',(5.06391465684653,4.48877013759614,26.5336898360191));
#15616=CARTESIAN_POINT('Ctrl Pts',(5.05036127242228,4.50406011234023,26.5346472708596));
#15617=CARTESIAN_POINT('Ctrl Pts',(5.03673774779103,4.519289705993,26.5356047057001));
#15618=CARTESIAN_POINT('Ctrl Pts',(5.02304462287122,4.53445826054718,26.5365621405406));
#15619=CARTESIAN_POINT('Ctrl Pts',(4.90014406771514,4.67060130945246,26.5451554509876));
#15620=CARTESIAN_POINT('Ctrl Pts',(4.77177744694847,4.80166499942981,26.5537487614345));
#15621=CARTESIAN_POINT('Ctrl Pts',(4.63839361530321,4.92722981699803,26.5623420718815));
#15622=CARTESIAN_POINT('Ctrl Pts',(4.50480522001602,5.05298720660488,26.5709485614286));
#15623=CARTESIAN_POINT('Ctrl Pts',(4.36618445496601,5.17322865585952,26.5795550509758));
#15624=CARTESIAN_POINT('Ctrl Pts',(4.22301459726595,5.28757380196993,26.5881615405229));
#15625=CARTESIAN_POINT('Ctrl Pts',(4.07972726804998,5.40201276879,26.5967750917337));
#15626=CARTESIAN_POINT('Ctrl Pts',(3.93188363982436,5.51054559246033,26.6053886429444));
#15627=CARTESIAN_POINT('Ctrl Pts',(3.77999676986812,5.61283470447746,26.6140021941552));
#15628=CARTESIAN_POINT('Ctrl Pts',(3.62789099708477,5.71527123789981,26.6226281594128));
#15629=CARTESIAN_POINT('Ctrl Pts',(3.47173059280552,5.81144590923214,26.6312541246703));
#15630=CARTESIAN_POINT('Ctrl Pts',(3.31205548077479,5.90106579291146,26.6398800899279));
#15631=CARTESIAN_POINT('Ctrl Pts',(3.2417606655077,5.94051973840976,26.6436775548337));
#15632=CARTESIAN_POINT('Ctrl Pts',(3.17078496699069,5.97870392470271,26.6474750197396));
#15633=CARTESIAN_POINT('Ctrl Pts',(3.09917575053263,6.01559628526637,26.6512724846455));
#15634=CARTESIAN_POINT('Origin',(0.,0.,-3.69717978381041));
#15635=CARTESIAN_POINT('',(3.09917575053261,6.01559628526638,29.0458547647091));
#15636=CARTESIAN_POINT('',(3.09917575053261,6.01559628526638,28.6513920151221));
#15637=CARTESIAN_POINT('',(3.09917575053259,6.01559628526639,-3.69717978381041));
#15638=CARTESIAN_POINT('',(-6.76699999999596,7.3958191851709E-6,27.697339049466));
#15639=CARTESIAN_POINT('Ctrl Pts',(-6.76699999999596,7.39581918517091E-6,
27.6973390494661));
#15640=CARTESIAN_POINT('Ctrl Pts',(-6.7670001871494,-0.171233584460114,
27.7054383317461));
#15641=CARTESIAN_POINT('Ctrl Pts',(-6.76049611965891,-0.342743673478981,
27.7135376140262));
#15642=CARTESIAN_POINT('Ctrl Pts',(-6.74745237752025,-0.513979973439041,
27.7216368963063));
#15643=CARTESIAN_POINT('Ctrl Pts',(-6.73442294962769,-0.685028358112737,
27.729727290407));
#15644=CARTESIAN_POINT('Ctrl Pts',(-6.71486815859784,-0.855803185644681,
27.7378176845078));
#15645=CARTESIAN_POINT('Ctrl Pts',(-6.68880455166524,-1.02575955741215,
27.7459080786085));
#15646=CARTESIAN_POINT('Ctrl Pts',(-6.66276391060138,-1.19556617263457,
27.7539913438828));
#15647=CARTESIAN_POINT('Ctrl Pts',(-6.63022592605018,-1.36455540354692,
27.7620746091571));
#15648=CARTESIAN_POINT('Ctrl Pts',(-6.59125909384202,-1.53218554941786,
27.7701578744315));
#15649=CARTESIAN_POINT('Ctrl Pts',(-6.55231817769273,-1.69970420783952,
27.7782357636881));
#15650=CARTESIAN_POINT('Ctrl Pts',(-6.50695701034635,-1.8658652211098,27.7863136529448));
#15651=CARTESIAN_POINT('Ctrl Pts',(-6.45529548783639,-2.03013525774001,
27.7943915422014));
#15652=CARTESIAN_POINT('Ctrl Pts',(-6.40365324082806,-2.19434400335125,
27.8024664175057));
#15653=CARTESIAN_POINT('Ctrl Pts',(-6.34571542684727,-2.35666282306734,
27.81054129281));
#15654=CARTESIAN_POINT('Ctrl Pts',(-6.28165231030984,-2.51657172605493,
27.8186161681143));
#15655=CARTESIAN_POINT('Ctrl Pts',(-6.21760043702092,-2.67645256460179,
27.8266896262563));
#15656=CARTESIAN_POINT('Ctrl Pts',(-6.14742553805268,-2.83392398395428,
27.8347630843984));
#15657=CARTESIAN_POINT('Ctrl Pts',(-6.07134667402418,-2.98848432550943,
27.8428365425405));
#15658=CARTESIAN_POINT('Ctrl Pts',(-5.99526628605105,-3.14304776308088,
27.8509101624029));
#15659=CARTESIAN_POINT('Ctrl Pts',(-5.91328186144791,-3.29469967410902,
27.8589837822653));
#15660=CARTESIAN_POINT('Ctrl Pts',(-5.8256591765079,-3.44296153901975,27.8670574021278));
#15661=CARTESIAN_POINT('Ctrl Pts',(-5.73801760162649,-3.59125536663447,
27.8751327625236));
#15662=CARTESIAN_POINT('Ctrl Pts',(-5.64473553593836,-3.73615737450748,
27.8832081229194));
#15663=CARTESIAN_POINT('Ctrl Pts',(-5.54612290580404,-3.87721674835387,
27.8912834833152));
#15664=CARTESIAN_POINT('Ctrl Pts',(-5.44741973880581,-4.01840562968135,
27.8993662577492));
#15665=CARTESIAN_POINT('Ctrl Pts',(-5.34337644596035,-4.15574452702552,
27.9074490321831));
#15666=CARTESIAN_POINT('Ctrl Pts',(-5.23434462480224,-4.28881397927259,
27.9155318066171));
#15667=CARTESIAN_POINT('Ctrl Pts',(-5.12525870432285,-4.42194945781337,
27.9236185915556));
#15668=CARTESIAN_POINT('Ctrl Pts',(-5.01117956973517,-4.55081099376952,
27.9317053764941));
#15669=CARTESIAN_POINT('Ctrl Pts',(-4.89249644265667,-4.67501524688335,
27.9397921614326));
#15670=CARTESIAN_POINT('Ctrl Pts',(-4.77365744848353,-4.79938261801195,
27.9478895667828));
#15671=CARTESIAN_POINT('Ctrl Pts',(-4.65020265096941,-4.91908023243594,
27.955986972133));
#15672=CARTESIAN_POINT('Ctrl Pts',(-4.52255582591572,-5.0337637808578,27.9640843774833));
#15673=CARTESIAN_POINT('Ctrl Pts',(-4.43712508178286,-5.11051853662517,
27.9695037630757));
#15674=CARTESIAN_POINT('Ctrl Pts',(-4.3498172885982,-5.18502819536259,27.9749231486681));
#15675=CARTESIAN_POINT('Ctrl Pts',(-4.26076671589499,-5.25720039495561,
27.9803425342605));
#15676=CARTESIAN_POINT('Ctrl Pts',(-4.1187015074195,-5.3723389984488,27.9889882523129));
#15677=CARTESIAN_POINT('Ctrl Pts',(-3.97183944392423,-5.48181868174055,
27.9976339703653));
#15678=CARTESIAN_POINT('Ctrl Pts',(-3.82064751921616,-5.58524319380163,
28.0062796884177));
#15679=CARTESIAN_POINT('Ctrl Pts',(-3.66964969412752,-5.68853492986644,
28.01491430713));
#15680=CARTESIAN_POINT('Ctrl Pts',(-3.51433334259644,-5.78578682430486,
28.0235489258424));
#15681=CARTESIAN_POINT('Ctrl Pts',(-3.35519781121756,-5.87664331464833,
28.0321835445547));
#15682=CARTESIAN_POINT('Ctrl Pts',(-3.19044223106302,-5.97070850328118,
28.0411231044572));
#15683=CARTESIAN_POINT('Ctrl Pts',(-3.02159302174582,-6.05791809718382,
28.0500626643596));
#15684=CARTESIAN_POINT('Ctrl Pts',(-2.84923897316472,-6.13792524178971,
28.059002224262));
#15685=CARTESIAN_POINT('Ctrl Pts',(-2.68322621993108,-6.214988742553,28.0676128775325));
#15686=CARTESIAN_POINT('Ctrl Pts',(-2.51396222508625,-6.28537014078503,
28.076223530803));
#15687=CARTESIAN_POINT('Ctrl Pts',(-2.3420002894792,-6.34880489888289,28.0848341840735));
#15688=CARTESIAN_POINT('Ctrl Pts',(-2.17020112735028,-6.41217961173775,
28.0934366867846));
#15689=CARTESIAN_POINT('Ctrl Pts',(-1.99570940121295,-6.46862068895084,
28.1020391894956));
#15690=CARTESIAN_POINT('Ctrl Pts',(-1.81909943967783,-6.51791118599846,
28.1106416922067));
#15691=CARTESIAN_POINT('Ctrl Pts',(-1.64268824909843,-6.56714620758409,
28.1192345129741));
#15692=CARTESIAN_POINT('Ctrl Pts',(-1.46416387233321,-6.60924662238,28.1278273337415));
#15693=CARTESIAN_POINT('Ctrl Pts',(-1.28411709459676,-6.64404487397281,
28.136420154509));
#15694=CARTESIAN_POINT('Ctrl Pts',(-1.26289776402047,-6.64814600598588,
28.1374328574673));
#15695=CARTESIAN_POINT('Ctrl Pts',(-1.24165730587066,-6.6521457698848,28.1384455604256));
#15696=CARTESIAN_POINT('Ctrl Pts',(-1.22039670119667,-6.65604393703259,
28.1394582633839));
#15697=CARTESIAN_POINT('Ctrl Pts',(-1.0399485492394,-6.68912940513782,28.148053521144));
#15698=CARTESIAN_POINT('Ctrl Pts',(-0.858260506854818,-6.71485308769088,
28.1566487789041));
#15699=CARTESIAN_POINT('Ctrl Pts',(-0.675944585442873,-6.73315586611587,
28.1652440366641));
#15700=CARTESIAN_POINT('Ctrl Pts',(-0.49345793290357,-6.75147578431653,
28.1738473435185));
#15701=CARTESIAN_POINT('Ctrl Pts',(-0.310342531523026,-6.76236089669446,
28.1824506503729));
#15702=CARTESIAN_POINT('Ctrl Pts',(-0.127212719760841,-6.76580415944262,
28.1910539572273));
#15703=CARTESIAN_POINT('Ctrl Pts',(0.0635097175020141,-6.76939018105836,
28.2000139601673));
#15704=CARTESIAN_POINT('Ctrl Pts',(0.254247404219202,-6.76490412677074,
28.2089739631073));
#15705=CARTESIAN_POINT('Ctrl Pts',(0.444311025072017,-6.75239784913474,
28.2179339660473));
#15706=CARTESIAN_POINT('Ctrl Pts',(0.627307511456925,-6.74035659234465,
28.226560809252));
#15707=CARTESIAN_POINT('Ctrl Pts',(0.809678866323325,-6.72088086671166,
28.2351876524568));
#15708=CARTESIAN_POINT('Ctrl Pts',(0.990818715418065,-6.69406955992969,
28.2438144956615));
#15709=CARTESIAN_POINT('Ctrl Pts',(1.17213168842088,-6.66723262831568,28.2524495839477));
#15710=CARTESIAN_POINT('Ctrl Pts',(1.35221050620472,-6.63304617489905,28.2610846722338));
#15711=CARTESIAN_POINT('Ctrl Pts',(1.53046029707631,-6.59165990317106,28.26971976052));
#15712=CARTESIAN_POINT('Ctrl Pts',(1.70897482465772,-6.55021216452434,28.2783676736451));
#15713=CARTESIAN_POINT('Ctrl Pts',(1.88565460173273,-6.50154331568327,28.2870155867703));
#15714=CARTESIAN_POINT('Ctrl Pts',(2.05991974628415,-6.44585290236045,28.2956634998954));
#15715=CARTESIAN_POINT('Ctrl Pts',(2.07946964263483,-6.43960528577028,28.2966336640994));
#15716=CARTESIAN_POINT('Ctrl Pts',(2.09898917067941,-6.43326934959204,28.2976038283034));
#15717=CARTESIAN_POINT('Ctrl Pts',(2.11847752795635,-6.42684541307351,28.2985739925073));
#15718=CARTESIAN_POINT('Ctrl Pts',(2.2836923362251,-6.37238574645526,28.3067986720261));
#15719=CARTESIAN_POINT('Ctrl Pts',(2.44702352994461,-6.31147945826268,28.3150233515449));
#15720=CARTESIAN_POINT('Ctrl Pts',(2.60793262039289,-6.24427549420193,28.3232480310637));
#15721=CARTESIAN_POINT('Ctrl Pts',(2.76867257718289,-6.17714216911042,28.3314640655139));
#15722=CARTESIAN_POINT('Ctrl Pts',(2.92699517249097,-6.1037244870511,28.339680099964));
#15723=CARTESIAN_POINT('Ctrl Pts',(3.08237717381573,-6.02422110802216,28.3478961344141));
#15724=CARTESIAN_POINT('Ctrl Pts',(3.2376269743666,-5.94478537137229,28.3561051785687));
#15725=CARTESIAN_POINT('Ctrl Pts',(3.38994084646355,-5.85927441225564,28.3643142227233));
#15726=CARTESIAN_POINT('Ctrl Pts',(3.53881556117961,-5.76793493582869,28.3725232668779));
#15727=CARTESIAN_POINT('Ctrl Pts',(3.68759342304055,-5.6766548817764,28.3807269705059));
#15728=CARTESIAN_POINT('Ctrl Pts',(3.83293627981061,-5.57955405018017,28.3889306741339));
#15729=CARTESIAN_POINT('Ctrl Pts',(3.97436546645699,-5.47692506238986,28.397134377762));
#15730=CARTESIAN_POINT('Ctrl Pts',(4.11573095881104,-5.37434229476742,28.4053343867559));
#15731=CARTESIAN_POINT('Ctrl Pts',(4.25318600307345,-5.26623654112658,28.4135343957499));
#15732=CARTESIAN_POINT('Ctrl Pts',(4.38628082680189,-5.15294377113026,28.4217344047438));
#15733=CARTESIAN_POINT('Ctrl Pts',(4.5193650079878,-5.03966006026253,28.4299337580477));
#15734=CARTESIAN_POINT('Ctrl Pts',(4.64808938472012,-4.92119038467458,28.4381331113517));
#15735=CARTESIAN_POINT('Ctrl Pts',(4.77203692199466,-4.79791127628677,28.4463324646556));
#15736=CARTESIAN_POINT('Ctrl Pts',(4.895983651168,-4.67463297164222,28.4545317645022));
#15737=CARTESIAN_POINT('Ctrl Pts',(5.01515334795759,-4.54654554870679,28.4627310643488));
#15738=CARTESIAN_POINT('Ctrl Pts',(5.12916564295834,-4.41406261929934,28.4709303641954));
#15739=CARTESIAN_POINT('Ctrl Pts',(5.24319787758171,-4.28155651993802,28.4791310980184));
#15740=CARTESIAN_POINT('Ctrl Pts',(5.3520706795134,-4.14465365428574,28.4873318318415));
#15741=CARTESIAN_POINT('Ctrl Pts',(5.45544377045798,-4.00380097749267,28.4955325656645));
#15742=CARTESIAN_POINT('Ctrl Pts',(5.55885369343053,-3.86289811462424,28.5037362214245));
#15743=CARTESIAN_POINT('Ctrl Pts',(5.65675978988914,-3.71804292599986,28.5119398771845));
#15744=CARTESIAN_POINT('Ctrl Pts',(5.74886490813213,-3.56971165054643,28.5201435329445));
#15745=CARTESIAN_POINT('Ctrl Pts',(5.84107553870865,-3.42121045208214,28.5283565865195));
#15746=CARTESIAN_POINT('Ctrl Pts',(5.92747172529262,-3.2692255161059,28.5365696400945));
#15747=CARTESIAN_POINT('Ctrl Pts',(6.00780161352396,-3.11425894436203,28.5447826936696));
#15748=CARTESIAN_POINT('Ctrl Pts',(6.08817903475258,-2.95920067542058,28.5530006070927));
#15749=CARTESIAN_POINT('Ctrl Pts',(6.16248284999782,-2.80115757771115,28.5612185205158));
#15750=CARTESIAN_POINT('Ctrl Pts',(6.2305093065635,-2.64065196132048,28.5694364339389));
#15751=CARTESIAN_POINT('Ctrl Pts',(6.29864186145479,-2.47989601030985,28.5776671645348));
#15752=CARTESIAN_POINT('Ctrl Pts',(6.36047736501064,-2.31667020032072,28.5858978951308));
#15753=CARTESIAN_POINT('Ctrl Pts',(6.41586148173165,-2.15151352476162,28.5941286257268));
#15754=CARTESIAN_POINT('Ctrl Pts',(6.46672516912585,-1.99983687062231,28.6016875674026));
#15755=CARTESIAN_POINT('Ctrl Pts',(6.51214814331083,-1.8465320462207,28.6092465090784));
#15756=CARTESIAN_POINT('Ctrl Pts',(6.55204900943375,-1.69202327938424,28.6168054507542));
#15757=CARTESIAN_POINT('Ctrl Pts',(6.59509039983991,-1.5253534097605,28.6249593429209));
#15758=CARTESIAN_POINT('Ctrl Pts',(6.63183856457751,-1.35676713161329,28.6331132350877));
#15759=CARTESIAN_POINT('Ctrl Pts',(6.66211904056673,-1.18678510662979,28.6412671272544));
#15760=CARTESIAN_POINT('Ctrl Pts',(6.69236256591543,-1.01701050720664,28.6494110693946));
#15761=CARTESIAN_POINT('Ctrl Pts',(6.71615404910189,-0.845843907220032,
28.6575550115349));
#15762=CARTESIAN_POINT('Ctrl Pts',(6.73336868715609,-0.67382128404045,28.6656989536751));
#15763=CARTESIAN_POINT('Ctrl Pts',(6.75056594188028,-0.501972369190823,
28.673834672068));
#15764=CARTESIAN_POINT('Ctrl Pts',(6.7611995368463,-0.32926951311978,28.6819703904609));
#15765=CARTESIAN_POINT('Ctrl Pts',(6.76519564457517,-0.156259049725841,
28.6901061088538));
#15766=CARTESIAN_POINT('Ctrl Pts',(6.76918855761934,0.016613100610356,28.6982353231541));
#15767=CARTESIAN_POINT('Ctrl Pts',(6.76655454048679,0.189792004779849,28.7063645374543));
#15768=CARTESIAN_POINT('Ctrl Pts',(6.7572715514346,0.362726040108322,28.7144937517545));
#15769=CARTESIAN_POINT('Ctrl Pts',(6.7479940317959,0.535558185006852,28.72261817643));
#15770=CARTESIAN_POINT('Ctrl Pts',(6.7320753613025,0.708145384171316,28.7307426011054));
#15771=CARTESIAN_POINT('Ctrl Pts',(6.7095455806479,0.879935850621083,28.7388670257809));
#15772=CARTESIAN_POINT('Ctrl Pts',(6.68687902980205,1.05276919517562,28.747040770915));
#15773=CARTESIAN_POINT('Ctrl Pts',(6.65752083013231,1.22479572676368,28.7552145160492));
#15774=CARTESIAN_POINT('Ctrl Pts',(6.6215546500722,1.39545799510671,28.7633882611834));
#15775=CARTESIAN_POINT('Ctrl Pts',(6.58581878690473,1.56502739222267,28.7715096640455));
#15776=CARTESIAN_POINT('Ctrl Pts',(6.54355942600176,1.73324959017862,28.7796310669077));
#15777=CARTESIAN_POINT('Ctrl Pts',(6.49491000028617,1.89958761003085,28.7877524697698));
#15778=CARTESIAN_POINT('Ctrl Pts',(6.4462568132529,2.06593849026376,28.7958745005361));
#15779=CARTESIAN_POINT('Ctrl Pts',(6.39121268000612,2.23040455093347,28.8039965313024));
#15780=CARTESIAN_POINT('Ctrl Pts',(6.32996096589675,2.39246382840441,28.8121185620687));
#15781=CARTESIAN_POINT('Ctrl Pts',(6.26869285238683,2.5545664952734,28.8202427674098));
#15782=CARTESIAN_POINT('Ctrl Pts',(6.20121397800711,2.71426075364746,28.8283669727509));
#15783=CARTESIAN_POINT('Ctrl Pts',(6.12775589813451,2.8710445229703,28.836491178092));
#15784=CARTESIAN_POINT('Ctrl Pts',(6.05350268537644,3.02952536810989,28.8447033223344));
#15785=CARTESIAN_POINT('Ctrl Pts',(5.97314023139421,3.1850320002565,28.8529154665768));
#15786=CARTESIAN_POINT('Ctrl Pts',(5.88695500353489,3.33707203793319,28.8611276108192));
#15787=CARTESIAN_POINT('Ctrl Pts',(5.80155655181722,3.48772411763622,28.8692647872357));
#15788=CARTESIAN_POINT('Ctrl Pts',(5.71044144084553,3.63497235413459,28.8774019636521));
#15789=CARTESIAN_POINT('Ctrl Pts',(5.61393136346961,3.77836785480878,28.8855391400686));
#15790=CARTESIAN_POINT('Ctrl Pts',(5.5160875647302,3.92374501012336,28.893788768224));
#15791=CARTESIAN_POINT('Ctrl Pts',(5.41269882774057,4.06516184721682,28.9020383963794));
#15792=CARTESIAN_POINT('Ctrl Pts',(5.30414154170348,4.20218651484861,28.9102880245348));
#15793=CARTESIAN_POINT('Ctrl Pts',(5.19558425566639,4.3392111824804,28.9185376526901));
#15794=CARTESIAN_POINT('Ctrl Pts',(5.08185871906685,4.47184342972856,28.9267872808455));
#15795=CARTESIAN_POINT('Ctrl Pts',(4.96337853470024,4.59969156805942,28.9350369090009));
#15796=CARTESIAN_POINT('Ctrl Pts',(4.84522764745455,4.72718437250814,28.9432636086066));
#15797=CARTESIAN_POINT('Ctrl Pts',(4.72199538861972,4.85030091817577,28.9514903082122));
#15798=CARTESIAN_POINT('Ctrl Pts',(4.59403826583033,4.9686116181572,28.9597170078178));
#15799=CARTESIAN_POINT('Ctrl Pts',(4.46626343348551,5.0867537701936,28.9679319874919));
#15800=CARTESIAN_POINT('Ctrl Pts',(4.33377741238652,5.20010347884628,28.9761469671659));
#15801=CARTESIAN_POINT('Ctrl Pts',(4.19697549336839,5.30826579101548,28.9843619468399));
#15802=CARTESIAN_POINT('Ctrl Pts',(4.06028604074079,5.41633918173585,28.9925701728871));
#15803=CARTESIAN_POINT('Ctrl Pts',(3.91928803241086,5.51923344367897,29.0007783989343));
#15804=CARTESIAN_POINT('Ctrl Pts',(3.77441252464447,5.61659141239658,29.0089866249815));
#15805=CARTESIAN_POINT('Ctrl Pts',(3.62965041303379,5.71387317762368,29.0171884263315));
#15806=CARTESIAN_POINT('Ctrl Pts',(3.4810171454555,5.80562708406218,29.0253902276814));
#15807=CARTESIAN_POINT('Ctrl Pts',(3.32897552920618,5.89153722944585,29.0335920290313));
#15808=CARTESIAN_POINT('Ctrl Pts',(3.25320168097652,5.93435275902437,29.0376796075906));
#15809=CARTESIAN_POINT('Ctrl Pts',(3.17658175697615,5.97571747579524,29.0417671861499));
#15810=CARTESIAN_POINT('Ctrl Pts',(3.09917575053261,6.01559628526638,29.0458547647091));
#15811=CARTESIAN_POINT('Ctrl Pts',(3.09917575053259,6.01559628526639,27.0457515827422));
#15812=CARTESIAN_POINT('Ctrl Pts',(2.93382384459261,6.10078395293761,27.0545010306546));
#15813=CARTESIAN_POINT('Ctrl Pts',(2.76495772122976,6.17915010267053,27.063250478567));
#15814=CARTESIAN_POINT('Ctrl Pts',(2.59315093316698,6.25042856433183,27.0719999264794));
#15815=CARTESIAN_POINT('Ctrl Pts',(2.42134553245604,6.32170645041456,27.0807493037394));
#15816=CARTESIAN_POINT('Ctrl Pts',(2.24659977927578,6.38589665313462,27.0894986809994));
#15817=CARTESIAN_POINT('Ctrl Pts',(2.06950718689906,6.44278115439079,27.0982480582594));
#15818=CARTESIAN_POINT('Ctrl Pts',(1.89241596572848,6.49966521519728,27.1069973677741));
#15819=CARTESIAN_POINT('Ctrl Pts',(1.71297821457185,6.54924360009549,27.1157466772887));
#15820=CARTESIAN_POINT('Ctrl Pts',(1.53180337335832,6.59134792173559,27.1244959868034));
#15821=CARTESIAN_POINT('Ctrl Pts',(1.35062987477783,6.63345193135304,27.1332452314795));
#15822=CARTESIAN_POINT('Ctrl Pts',(1.16771959102965,6.66808192368235,27.1419944761556));
#15823=CARTESIAN_POINT('Ctrl Pts',(0.983693746907115,6.69512028363164,27.1507437208317));
#15824=CARTESIAN_POINT('Ctrl Pts',(0.799669205420143,6.72215845218864,27.1594929035759));
#15825=CARTESIAN_POINT('Ctrl Pts',(0.614529402873749,6.74160505424577,27.1682420863201));
#15826=CARTESIAN_POINT('Ctrl Pts',(0.428903127363522,6.7533940435412,27.1769912690643));
#15827=CARTESIAN_POINT('Ctrl Pts',(0.243278104164177,6.76518295330329,27.1857403927829));
#15828=CARTESIAN_POINT('Ctrl Pts',(0.0571669005394398,6.76931433552275,
27.1944895165015));
#15829=CARTESIAN_POINT('Ctrl Pts',(-0.128798404777167,6.76577415902474,
27.2032386402201));
#15830=CARTESIAN_POINT('Ctrl Pts',(-0.314762517258715,6.76223400523443,
27.2119877078193));
#15831=CARTESIAN_POINT('Ctrl Pts',(-0.500580446819089,6.75102239665092,
27.2207367754185));
#15832=CARTESIAN_POINT('Ctrl Pts',(-0.685621118842153,6.73217741012502,
27.2294858430177));
#15833=CARTESIAN_POINT('Ctrl Pts',(-0.870660665414015,6.71333253821778,
27.2382348574035));
#15834=CARTESIAN_POINT('Ctrl Pts',(-1.05492267885438,6.6868544103062,27.2469838717893));
#15835=CARTESIAN_POINT('Ctrl Pts',(-1.23778137635202,6.65283295028187,27.255732886175));
#15836=CARTESIAN_POINT('Ctrl Pts',(-1.429999229788,6.61707018861875,27.2649296965424));
#15837=CARTESIAN_POINT('Ctrl Pts',(-1.62066601233653,6.57297172934423,27.2741265069098));
#15838=CARTESIAN_POINT('Ctrl Pts',(-1.80906628500347,6.52070304311305,27.2833233172772));
#15839=CARTESIAN_POINT('Ctrl Pts',(-1.98831342545486,6.47097374915043,27.292073315015));
#15840=CARTESIAN_POINT('Ctrl Pts',(-2.16550875896657,6.41384933989543,27.3008233127528));
#15841=CARTESIAN_POINT('Ctrl Pts',(-2.34005036713964,6.34952386240493,27.3095733104905));
#15842=CARTESIAN_POINT('Ctrl Pts',(-2.51458843547038,6.28519968948616,27.3183231307714));
#15843=CARTESIAN_POINT('Ctrl Pts',(-2.68647261718,6.21367483971123,27.3270729510522));
#15844=CARTESIAN_POINT('Ctrl Pts',(-2.85511905908673,6.13519226743871,27.3358227713331));
#15845=CARTESIAN_POINT('Ctrl Pts',(-3.02376230488819,6.05671118252969,27.3445724257916));
#15846=CARTESIAN_POINT('Ctrl Pts',(-3.18916767379834,5.9712727599267,27.3533220802502));
#15847=CARTESIAN_POINT('Ctrl Pts',(-3.35077334102712,5.8791672043804,27.3620717347087));
#15848=CARTESIAN_POINT('Ctrl Pts',(-3.5123761603729,5.7870632719569,27.3708212349771));
#15849=CARTESIAN_POINT('Ctrl Pts',(-3.6701791630222,5.6882925836235,27.3795707352456));
#15850=CARTESIAN_POINT('Ctrl Pts',(-3.82364636566381,5.58319061741098,27.388320235514));
#15851=CARTESIAN_POINT('Ctrl Pts',(-3.97711106778721,5.47809036367758,27.3970695932225));
#15852=CARTESIAN_POINT('Ctrl Pts',(-4.12623987481854,5.36665920043281,27.4058189509309));
#15853=CARTESIAN_POINT('Ctrl Pts',(-4.27052628213861,5.24927559512391,27.4145683086393));
#15854=CARTESIAN_POINT('Ctrl Pts',(-4.41481053024924,5.13189374643084,27.4233175354159));
#15855=CARTESIAN_POINT('Ctrl Pts',(-4.5542523013649,5.00855981477391,27.4320667621924));
#15856=CARTESIAN_POINT('Ctrl Pts',(-4.6883780063052,4.87969268192103,27.4408159889689));
#15857=CARTESIAN_POINT('Ctrl Pts',(-4.82250188228861,4.75082730631843,27.4495650964397));
#15858=CARTESIAN_POINT('Ctrl Pts',(-4.95130963052928,4.61642907903566,27.4583142039106));
#15859=CARTESIAN_POINT('Ctrl Pts',(-5.07436379033325,4.47695444731737,27.4670633113814));
#15860=CARTESIAN_POINT('Ctrl Pts',(-5.19741643562769,4.3374815322063,27.4758123111712));
#15861=CARTESIAN_POINT('Ctrl Pts',(-5.31471544462742,4.19293255254629,27.4845613109609));
#15862=CARTESIAN_POINT('Ctrl Pts',(-5.42586245275601,4.04379841779638,27.4933103107507));
#15863=CARTESIAN_POINT('Ctrl Pts',(-5.53702160019125,3.89464799484383,27.5020602660928));
#15864=CARTESIAN_POINT('Ctrl Pts',(-5.64202723081222,3.74091164443895,27.510810221435));
#15865=CARTESIAN_POINT('Ctrl Pts',(-5.74052265232936,3.58311159163283,27.5195601767771));
#15866=CARTESIAN_POINT('Ctrl Pts',(-5.83901427066894,3.42531763191825,27.5283097942596));
#15867=CARTESIAN_POINT('Ctrl Pts',(-5.93099603115722,3.26346052695645,27.537059411742));
#15868=CARTESIAN_POINT('Ctrl Pts',(-6.01615550622742,3.09809004467099,27.5458090292245));
#15869=CARTESIAN_POINT('Ctrl Pts',(-6.10131214578801,2.93272506863826,27.5545583553756));
#15870=CARTESIAN_POINT('Ctrl Pts',(-6.17964682328761,2.76384720416866,27.5633076815267));
#15871=CARTESIAN_POINT('Ctrl Pts',(-6.25089348288587,2.59203002791538,27.5720570076778));
#15872=CARTESIAN_POINT('Ctrl Pts',(-6.3221381488934,2.42021765937001,27.5808060890094));
#15873=CARTESIAN_POINT('Ctrl Pts',(-6.38629508412584,2.24546640831917,27.5895551703409));
#15874=CARTESIAN_POINT('Ctrl Pts',(-6.44314639819803,2.0683697666007,27.5983042516725));
#15875=CARTESIAN_POINT('Ctrl Pts',(-6.50000285283692,1.89125711158305,27.6070541241069));
#15876=CARTESIAN_POINT('Ctrl Pts',(-6.54955227673241,1.71179891440286,27.6158039965413));
#15877=CARTESIAN_POINT('Ctrl Pts',(-6.59162635926377,1.53060476278464,27.6245538689757));
#15878=CARTESIAN_POINT('Ctrl Pts',(-6.63369752055188,1.34942319164737,27.6333031338982));
#15879=CARTESIAN_POINT('Ctrl Pts',(-6.66829431424245,1.16650618642754,27.6420523988207));
#15880=CARTESIAN_POINT('Ctrl Pts',(-6.69529923745409,0.982474997619145,
27.6508016637432));
#15881=CARTESIAN_POINT('Ctrl Pts',(-6.72230554731437,0.7984343591783,27.6595513779229));
#15882=CARTESIAN_POINT('Ctrl Pts',(-6.74171916496698,0.613279706240868,
27.6683010921026));
#15883=CARTESIAN_POINT('Ctrl Pts',(-6.75347414817272,0.427639953655878,
27.6770508062823));
#15884=CARTESIAN_POINT('Ctrl Pts',(-6.76248837758744,0.285283364198805,
27.6837604654582));
#15885=CARTESIAN_POINT('Ctrl Pts',(-6.76699999999997,0.142641701105077,
27.6904701246341));
#15886=CARTESIAN_POINT('Ctrl Pts',(-6.767,1.25880014828821E-12,27.69717978381));
#15887=CARTESIAN_POINT('',(-6.76699999814636,-0.000158389305696416,27.3028276665937));
#15888=CARTESIAN_POINT('Ctrl Pts',(3.09917575053263,6.01559628526637,26.6512724846455));
#15889=CARTESIAN_POINT('Ctrl Pts',(2.93615363517035,6.09958366785864,26.6599176115243));
#15890=CARTESIAN_POINT('Ctrl Pts',(2.7698470990166,6.17687257815703,26.6685627384031));
#15891=CARTESIAN_POINT('Ctrl Pts',(2.60082787562788,6.24723805864296,26.6772078652819));
#15892=CARTESIAN_POINT('Ctrl Pts',(2.48185569699916,6.29676813188447,26.6832931469361));
#15893=CARTESIAN_POINT('Ctrl Pts',(2.36153985499742,6.342868865374,26.6893784285903));
#15894=CARTESIAN_POINT('Ctrl Pts',(2.24008408109763,6.38547667050887,26.6954637102445));
#15895=CARTESIAN_POINT('Ctrl Pts',(2.07590198617098,6.44307326293634,26.7036897027858));
#15896=CARTESIAN_POINT('Ctrl Pts',(1.90928160896034,6.49440925938956,26.7119156953272));
#15897=CARTESIAN_POINT('Ctrl Pts',(1.7407407993885,6.53927446046916,26.7201416878685));
#15898=CARTESIAN_POINT('Ctrl Pts',(1.57237668307084,6.58409262618447,26.7283590565199));
#15899=CARTESIAN_POINT('Ctrl Pts',(1.40209648705597,6.62245341415902,26.7365764251714));
#15900=CARTESIAN_POINT('Ctrl Pts',(1.23043626458179,6.65419533819094,26.7447937938228));
#15901=CARTESIAN_POINT('Ctrl Pts',(1.05892165719612,6.68591033633979,26.7530041918852));
#15902=CARTESIAN_POINT('Ctrl Pts',(0.886029705179472,6.71101758802962,26.7612145899475));
#15903=CARTESIAN_POINT('Ctrl Pts',(0.712309885730461,6.72940588957827,26.7694249880099));
#15904=CARTESIAN_POINT('Ctrl Pts',(0.538702677679996,6.74778227117236,26.7776300637987));
#15905=CARTESIAN_POINT('Ctrl Pts',(0.364269026195079,6.75944834081458,26.7858351395875));
#15906=CARTESIAN_POINT('Ctrl Pts',(0.189566921231981,6.76434426846939,26.7940402153763));
#15907=CARTESIAN_POINT('Ctrl Pts',(0.0149431242319189,6.76923800158783,
26.8022416133458));
#15908=CARTESIAN_POINT('Ctrl Pts',(-0.159948529112916,6.76736762857281,
26.8104430113153));
#15909=CARTESIAN_POINT('Ctrl Pts',(-0.334546531099286,6.75872529538888,
26.8186444092848));
#15910=CARTESIAN_POINT('Ctrl Pts',(-0.509130857116212,6.75008363914445,
26.8268451648525));
#15911=CARTESIAN_POINT('Ctrl Pts',(-0.683421219594534,6.73467108828651,
26.8350459204202));
#15912=CARTESIAN_POINT('Ctrl Pts',(-0.856857337853241,6.71253189955676,
26.8432466759879));
#15913=CARTESIAN_POINT('Ctrl Pts',(-1.03029257513892,6.69039282328356,26.8514473898997));
#15914=CARTESIAN_POINT('Ctrl Pts',(-1.202873221224,6.6615272215178,26.8596481038115));
#15915=CARTESIAN_POINT('Ctrl Pts',(-1.37404545732681,6.62603109570123,26.8678488177232));
#15916=CARTESIAN_POINT('Ctrl Pts',(-1.5452478446275,6.59052871740623,26.8760509761528));
#15917=CARTESIAN_POINT('Ctrl Pts',(-1.71504097676692,6.54839356091663,26.8842531345824));
#15918=CARTESIAN_POINT('Ctrl Pts',(-1.88288248819614,6.49977249876058,26.892455293012));
#15919=CARTESIAN_POINT('Ctrl Pts',(-2.05078398151387,6.45113406078906,26.900660382665));
#15920=CARTESIAN_POINT('Ctrl Pts',(-2.21673212074827,6.39600519944694,26.9088654723179));
#15921=CARTESIAN_POINT('Ctrl Pts',(-2.38020087270768,6.33458229132447,26.9170705619708));
#15922=CARTESIAN_POINT('Ctrl Pts',(-2.54385636838946,6.27308921479145,26.9252850249686));
#15923=CARTESIAN_POINT('Ctrl Pts',(-2.70502648233334,6.20528785289478,26.9334994879664));
#15924=CARTESIAN_POINT('Ctrl Pts',(-2.86320532400266,6.13142269563948,26.9417139509642));
#15925=CARTESIAN_POINT('Ctrl Pts',(-3.02147788163616,6.05751377561312,26.9499332807716));
#15926=CARTESIAN_POINT('Ctrl Pts',(-3.17675531619248,5.97753406260601,26.9581526105791));
#15927=CARTESIAN_POINT('Ctrl Pts',(-3.32855754199713,5.89177339089124,26.9663719403866));
#15928=CARTESIAN_POINT('Ctrl Pts',(-3.48059497614724,5.80587983821513,26.9746040055473));
#15929=CARTESIAN_POINT('Ctrl Pts',(-3.62914613621989,5.71418761486332,26.982836070708));
#15930=CARTESIAN_POINT('Ctrl Pts',(-3.77375994572452,5.61702989773468,26.9910681358687));
#15931=CARTESIAN_POINT('Ctrl Pts',(-3.90374922154912,5.52969756527221,26.9984677071298));
#15932=CARTESIAN_POINT('Ctrl Pts',(-4.03055751378548,5.43794994954438,27.005867278391));
#15933=CARTESIAN_POINT('Ctrl Pts',(-4.15388145949066,5.34205558006464,27.0132668496522));
#15934=CARTESIAN_POINT('Ctrl Pts',(-4.28824747095195,5.23757510893708,27.0213289569031));
#15935=CARTESIAN_POINT('Ctrl Pts',(-4.41891022822859,5.12783417337497,27.0293910641541));
#15936=CARTESIAN_POINT('Ctrl Pts',(-4.5454190056654,5.01312827114326,27.037453171405));
#15937=CARTESIAN_POINT('Ctrl Pts',(-4.67177407218353,4.89856173907991,27.0455054830202));
#15938=CARTESIAN_POINT('Ctrl Pts',(-4.79398492773395,4.7790424921065,27.0535577946353));
#15939=CARTESIAN_POINT('Ctrl Pts',(-4.91163038948578,4.65490879793362,27.0616101062505));
#15940=CARTESIAN_POINT('Ctrl Pts',(-5.02915884175316,4.53089856640299,27.0696544090838));
#15941=CARTESIAN_POINT('Ctrl Pts',(-5.1421306812953,4.40228329063955,27.0776987119172));
#15942=CARTESIAN_POINT('Ctrl Pts',(-5.25015845764759,4.26944084975907,27.0857430147505));
#15943=CARTESIAN_POINT('Ctrl Pts',(-5.35810256470482,4.13670129754073,27.0937810871386));
#15944=CARTESIAN_POINT('Ctrl Pts',(-5.4611099955365,3.9997413858845,27.1018191595267));
#15945=CARTESIAN_POINT('Ctrl Pts',(-5.55883087639642,3.85897503070722,27.1098572319148));
#15946=CARTESIAN_POINT('Ctrl Pts',(-5.65650147768686,3.7182811029546,27.1178911685357));
#15947=CARTESIAN_POINT('Ctrl Pts',(-5.748890729455,3.57378493610329,27.1259251051565));
#15948=CARTESIAN_POINT('Ctrl Pts',(-5.83568975566038,3.42593258481256,27.1339590417774));
#15949=CARTESIAN_POINT('Ctrl Pts',(-5.92246553100392,3.27811983874258,27.141990826347));
#15950=CARTESIAN_POINT('Ctrl Pts',(-6.00365387041939,3.12695301925926,27.1500226109166));
#15951=CARTESIAN_POINT('Ctrl Pts',(-6.07898992023337,2.97290607818362,27.1580543954862));
#15952=CARTESIAN_POINT('Ctrl Pts',(-6.15432077633269,2.81886975720098,27.1660856263396));
#15953=CARTESIAN_POINT('Ctrl Pts',(-6.22379998117649,2.66195404604556,27.1741168571929));
#15954=CARTESIAN_POINT('Ctrl Pts',(-6.28720931491777,2.50265619500786,27.1821480880463));
#15955=CARTESIAN_POINT('Ctrl Pts',(-6.35062689211165,2.34333763464859,27.1901803629899));
#15956=CARTESIAN_POINT('Ctrl Pts',(-6.40797288983725,2.18163666614524,27.1982126379336));
#15957=CARTESIAN_POINT('Ctrl Pts',(-6.45907784002637,2.01806899200207,27.2062449128772));
#15958=CARTESIAN_POINT('Ctrl Pts',(-6.51022689465075,1.85436015619322,27.2142841198098));
#15959=CARTESIAN_POINT('Ctrl Pts',(-6.55512403028306,1.68878175439402,27.2223233267424));
#15960=CARTESIAN_POINT('Ctrl Pts',(-6.59364995435232,1.52186375194027,27.230362533675));
#15961=CARTESIAN_POINT('Ctrl Pts',(-6.6321922737588,1.35487471479997,27.2384051618236));
#15962=CARTESIAN_POINT('Ctrl Pts',(-6.66435790990869,1.18654530878259,27.2464477899723));
#15963=CARTESIAN_POINT('Ctrl Pts',(-6.69007911768547,1.01741358311594,27.2544904181209));
#15964=CARTESIAN_POINT('Ctrl Pts',(-6.71583589395875,0.848047974140052,
27.2625441679942));
#15965=CARTESIAN_POINT('Ctrl Pts',(-6.73513039384976,0.677878200650345,
27.2705979178675));
#15966=CARTESIAN_POINT('Ctrl Pts',(-6.74794688764199,0.507446353384106,
27.2786516677408));
#15967=CARTESIAN_POINT('Ctrl Pts',(-6.76066490161465,0.338324076257635,
27.2866435339315));
#15968=CARTESIAN_POINT('Ctrl Pts',(-6.76700418638193,0.16894409523193,27.2946354001221));
#15969=CARTESIAN_POINT('Ctrl Pts',(-6.76699999792448,-0.000167601012896156,
27.3026272663128));
#15970=CARTESIAN_POINT('Ctrl Pts',(-6.76699999814636,-0.000158389305696416,
27.3028276665937));
#15971=CARTESIAN_POINT('Ctrl Pts',(-6.76699564443585,-0.186165638445246,
27.311577178389));
#15972=CARTESIAN_POINT('Ctrl Pts',(-6.75931766370376,-0.37217256467103,
27.3203266901844));
#15973=CARTESIAN_POINT('Ctrl Pts',(-6.74399213454365,-0.557547387415058,
27.3290762019797));
#15974=CARTESIAN_POINT('Ctrl Pts',(-6.72866667011378,-0.742921427193918,
27.3378256768199));
#15975=CARTESIAN_POINT('Ctrl Pts',(-6.70569374550785,-0.927663083204684,
27.3465751516601));
#15976=CARTESIAN_POINT('Ctrl Pts',(-6.67515138859919,-1.11114487771953,
27.3553246265002));
#15977=CARTESIAN_POINT('Ctrl Pts',(-6.64460915815518,-1.29462591250379,
27.364074065112));
#15978=CARTESIAN_POINT('Ctrl Pts',(-6.60649760518768,-1.47684681352381,
27.3728235037238));
#15979=CARTESIAN_POINT('Ctrl Pts',(-6.56094617507105,-1.657188669953,27.3815729423356));
#15980=CARTESIAN_POINT('Ctrl Pts',(-6.51539492978294,-1.83752979463085,
27.3903223454459));
#15981=CARTESIAN_POINT('Ctrl Pts',(-6.46240393793969,-2.01599161211029,
27.3990717485562));
#15982=CARTESIAN_POINT('Ctrl Pts',(-6.4021531812695,-2.19196798415506,27.4078211516664));
#15983=CARTESIAN_POINT('Ctrl Pts',(-6.34190266406773,-2.36794365677655,
27.416570520002));
#15984=CARTESIAN_POINT('Ctrl Pts',(-6.27439253261081,-2.54143363259705,
27.4253198883375));
#15985=CARTESIAN_POINT('Ctrl Pts',(-6.19985208046774,-2.71184866471561,
27.434069256673));
#15986=CARTESIAN_POINT('Ctrl Pts',(-6.12531191839751,-2.88226303366712,
27.4428185909605));
#15987=CARTESIAN_POINT('Ctrl Pts',(-6.04374160523462,-3.04960222030065,
27.451567925248));
#15988=CARTESIAN_POINT('Ctrl Pts',(-5.95541818684473,-3.21329787287127,
27.4603172595355));
#15989=CARTESIAN_POINT('Ctrl Pts',(-5.86709510482902,-3.3769929020173,27.4690665605017));
#15990=CARTESIAN_POINT('Ctrl Pts',(-5.77201910513236,-3.53704417266323,
27.4778158614679));
#15991=CARTESIAN_POINT('Ctrl Pts',(-5.67051310195223,-3.69290808991886,
27.4865651624341));
#15992=CARTESIAN_POINT('Ctrl Pts',(-5.56900747692194,-3.84877142652,27.4953144308057));
#15993=CARTESIAN_POINT('Ctrl Pts',(-5.46107205273131,-4.00044720081222,
27.5040636991773));
#15994=CARTESIAN_POINT('Ctrl Pts',(-5.34707341633779,-4.14742026810568,
27.5128129675489));
#15995=CARTESIAN_POINT('Ctrl Pts',(-5.23307519516778,-4.29439280007104,
27.5215622040526));
#15996=CARTESIAN_POINT('Ctrl Pts',(-5.11301398162055,-4.43666243288071,
27.5303114405563));
#15997=CARTESIAN_POINT('Ctrl Pts',(-4.98729754316467,-4.57374597195161,
27.5390606770599));
#15998=CARTESIAN_POINT('Ctrl Pts',(-4.8615815521733,-4.71082902309892,27.5478098824223));
#15999=CARTESIAN_POINT('Ctrl Pts',(-4.73021057023571,-4.84272580625139,
27.5565590877847));
#16000=CARTESIAN_POINT('Ctrl Pts',(-4.59363077335013,-4.96898835962922,
27.5653082931471));
#16001=CARTESIAN_POINT('Ctrl Pts',(-4.45705145125412,-5.0952504740831,27.5740574680948));
#16002=CARTESIAN_POINT('Ctrl Pts',(-4.31526356086088,-5.21587820343581,
27.5828066430424));
#16003=CARTESIAN_POINT('Ctrl Pts',(-4.16874865382824,-5.33046186190327,
27.5915558179901));
#16004=CARTESIAN_POINT('Ctrl Pts',(-4.02223424395669,-5.4450451315602,27.6003049632497));
#16005=CARTESIAN_POINT('Ctrl Pts',(-3.87099307526245,-5.55358419484709,
27.6090541085093));
#16006=CARTESIAN_POINT('Ctrl Pts',(-3.71553880191979,-5.65571042499777,
27.6178032537689));
#16007=CARTESIAN_POINT('Ctrl Pts',(-3.56008504316433,-5.75783631708858,
27.6265523700669));
#16008=CARTESIAN_POINT('Ctrl Pts',(-3.4004184471562,-5.85354926119071,27.635301486365));
#16009=CARTESIAN_POINT('Ctrl Pts',(-3.23708127941626,-5.94252419351009,
27.644050602663));
#16010=CARTESIAN_POINT('Ctrl Pts',(-3.07374463879529,-6.03149883869107,
27.652799690726));
#16011=CARTESIAN_POINT('Ctrl Pts',(-2.90673770177539,-6.11373537853349,
27.6615487787891));
#16012=CARTESIAN_POINT('Ctrl Pts',(-2.73662765975433,-6.18895452010011,
27.6702978668521));
#16013=CARTESIAN_POINT('Ctrl Pts',(-2.56651815258613,-6.26417342516586,
27.6790469274066));
#16014=CARTESIAN_POINT('Ctrl Pts',(-2.39330582200001,-6.33237486023128,
27.6877959879611));
#16015=CARTESIAN_POINT('Ctrl Pts',(-2.21757893054653,-6.39332720004194,
27.6965450485156));
#16016=CARTESIAN_POINT('Ctrl Pts',(-2.04185257701619,-6.45427935326946,
27.7052940822881));
#16017=CARTESIAN_POINT('Ctrl Pts',(-1.86361194873049,-6.50798236175061,
27.7140431160606));
#16018=CARTESIAN_POINT('Ctrl Pts',(-1.68346238160849,-6.55425384080515,
27.7227921498331));
#16019=CARTESIAN_POINT('Ctrl Pts',(-1.50331335099113,-6.60052518205829,
27.73154115755));
#16020=CARTESIAN_POINT('Ctrl Pts',(-1.32125567043228,-6.63936496689287,
27.740290165267));
#16021=CARTESIAN_POINT('Ctrl Pts',(-1.13790763553999,-6.67064128948483,
27.7490391729839));
#16022=CARTESIAN_POINT('Ctrl Pts',(-0.954560131456165,-6.70191752152912,
27.7577881553717));
#16023=CARTESIAN_POINT('Ctrl Pts',(-0.769922562956765,-6.725630286969,27.7665371377595));
#16024=CARTESIAN_POINT('Ctrl Pts',(-0.584621983715095,-6.74169905410773,
27.7752861201473));
#16025=CARTESIAN_POINT('Ctrl Pts',(-0.39133411198032,-6.75846045773829,
27.7844122232199));
#16026=CARTESIAN_POINT('Ctrl Pts',(-0.197325135735471,-6.76690423582442,
27.7935383262926));
#16027=CARTESIAN_POINT('Ctrl Pts',(-0.00331189650882545,-6.76699918954787,
27.8026644293652));
#16028=CARTESIAN_POINT('Ctrl Pts',(0.18463842899198,-6.76709117596747,27.8115053417169));
#16029=CARTESIAN_POINT('Ctrl Pts',(0.372592438084156,-6.75934828281543,
27.8203462540685));
#16030=CARTESIAN_POINT('Ctrl Pts',(0.559898343344746,-6.74379736091765,
27.8291871664201));
#16031=CARTESIAN_POINT('Ctrl Pts',(0.74527770155342,-6.7284063890369,27.8379371449937));
#16032=CARTESIAN_POINT('Ctrl Pts',(0.930021936897552,-6.70536729682682,
27.8466871235672));
#16033=CARTESIAN_POINT('Ctrl Pts',(1.11350349070759,-6.67475834590152,27.8554371021407));
#16034=CARTESIAN_POINT('Ctrl Pts',(1.29698316624787,-6.6441497083149,27.8641869911422));
#16035=CARTESIAN_POINT('Ctrl Pts',(1.47919990335411,-6.60597141425457,27.8729368801437));
#16036=CARTESIAN_POINT('Ctrl Pts',(1.65953474168855,-6.56035314911695,27.8816867691451));
#16037=CARTESIAN_POINT('Ctrl Pts',(1.83986779389779,-6.51473533580514,27.8904365714834));
#16038=CARTESIAN_POINT('Ctrl Pts',(2.01831870672899,-6.46167776917716,27.8991863738216));
#16039=CARTESIAN_POINT('Ctrl Pts',(2.19428132372643,-6.40136067350883,27.9079361761599));
#16040=CARTESIAN_POINT('Ctrl Pts',(2.37024225637796,-6.34104415520662,27.9166858947434));
#16041=CARTESIAN_POINT('Ctrl Pts',(2.54371466970189,-6.27346833986935,27.925435613327));
#16042=CARTESIAN_POINT('Ctrl Pts',(2.71410932932242,-6.19886276251419,27.9341853319106));
#16043=CARTESIAN_POINT('Ctrl Pts',(2.88450241451495,-6.12425787450639,27.9429349696477));
#16044=CARTESIAN_POINT('Ctrl Pts',(3.05181754034475,-6.04262346942454,27.9516846073848));
#16045=CARTESIAN_POINT('Ctrl Pts',(3.21548639740849,-5.9542368300296,27.9604342451219));
#16046=CARTESIAN_POINT('Ctrl Pts',(3.37915379657157,-5.86585097794964,27.9691838049206));
#16047=CARTESIAN_POINT('Ctrl Pts',(3.53917473976983,-5.77071314811019,27.9779333647192));
#16048=CARTESIAN_POINT('Ctrl Pts',(3.69500570299244,-5.6691464838063,27.9866829245179));
#16049=CARTESIAN_POINT('Ctrl Pts',(3.85083532990542,-5.56758069047509,27.9954324092857));
#16050=CARTESIAN_POINT('Ctrl Pts',(4.00247480863557,-5.45958632949755,28.0041818940535));
#16051=CARTESIAN_POINT('Ctrl Pts',(4.14940909231515,-5.34553020612664,28.0129313788214));
#16052=CARTESIAN_POINT('Ctrl Pts',(4.29634216479246,-5.2314750229382,28.0216807914658));
#16053=CARTESIAN_POINT('Ctrl Pts',(4.43856989344099,-5.11135835308375,28.0304302041103));
#16054=CARTESIAN_POINT('Ctrl Pts',(4.57560920656789,-4.98558816878923,28.0391796167548));
#16055=CARTESIAN_POINT('Ctrl Pts',(4.71264743558326,-4.8598189794567,28.0479289601831));
#16056=CARTESIAN_POINT('Ctrl Pts',(4.8444971200733,-4.72839655896145,28.0566783036114));
#16057=CARTESIAN_POINT('Ctrl Pts',(4.97071044410098,-4.59176727207569,28.0654276470396));
#16058=CARTESIAN_POINT('Ctrl Pts',(5.09692281158692,-4.45513902067185,28.0741769241587));
#16059=CARTESIAN_POINT('Ctrl Pts',(5.21749870963727,-4.31330419234739,28.0829262012777));
#16060=CARTESIAN_POINT('Ctrl Pts',(5.33202861894698,-4.16674450941384,28.0916754783967));
#16061=CARTESIAN_POINT('Ctrl Pts',(5.44655769830365,-4.02018588854046,28.1004246921132));
#16062=CARTESIAN_POINT('Ctrl Pts',(5.5550407001457,-3.86890270737006,28.1091739058296));
#16063=CARTESIAN_POINT('Ctrl Pts',(5.65710918234642,-3.71340877079427,28.1179231195461));
#16064=CARTESIAN_POINT('Ctrl Pts',(5.75917695879893,-3.55791590937474,28.1266722727665));
#16065=CARTESIAN_POINT('Ctrl Pts',(5.85483014711972,-3.39821259036579,28.1354214259869));
#16066=CARTESIAN_POINT('Ctrl Pts',(5.94374388372034,-3.2348412085815,28.1441705792073));
#16067=CARTESIAN_POINT('Ctrl Pts',(6.03265703506149,-3.07147090216142,28.1529196748378));
#16068=CARTESIAN_POINT('Ctrl Pts',(6.1148306864786,-2.90443283296427,28.1616687704684));
#16069=CARTESIAN_POINT('Ctrl Pts',(6.18998575813472,-2.73429429909975,28.170417866099));
#16070=CARTESIAN_POINT('Ctrl Pts',(6.26514036005544,-2.56415682863772,28.1791669070459));
#16071=CARTESIAN_POINT('Ctrl Pts',(6.33327635422231,-2.39091919438814,28.1879159479927));
#16072=CARTESIAN_POINT('Ctrl Pts',(6.39416233866698,-2.21516974220327,28.1966649889396));
#16073=CARTESIAN_POINT('Ctrl Pts',(6.45504796278121,-2.03942133012435,28.2054139781086));
#16074=CARTESIAN_POINT('Ctrl Pts',(6.50868356924084,-1.86116140059545,28.2141629672776));
#16075=CARTESIAN_POINT('Ctrl Pts',(6.55488700412989,-1.68099534891952,28.2229119564466));
#16076=CARTESIAN_POINT('Ctrl Pts',(6.60202876080853,-1.49717039758741,28.2318386243357));
#16077=CARTESIAN_POINT('Ctrl Pts',(6.64143315241961,-1.31136136892039,28.2407652922247));
#16078=CARTESIAN_POINT('Ctrl Pts',(6.67296087137084,-1.12422515945592,28.2496919601138));
#16079=CARTESIAN_POINT('Ctrl Pts',(6.7038643211654,-0.940794367558994,28.2584418742249));
#16080=CARTESIAN_POINT('Ctrl Pts',(6.72720006210098,-0.756088753450049,
28.267191788336));
#16081=CARTESIAN_POINT('Ctrl Pts',(6.74288882604265,-0.570735735370709,
28.2759417024471));
#16082=CARTESIAN_POINT('Ctrl Pts',(6.75857728146194,-0.385386362292,28.2846914444896));
#16083=CARTESIAN_POINT('Ctrl Pts',(6.76661903663616,-0.199389896352124,
28.2934411865321));
#16084=CARTESIAN_POINT('Ctrl Pts',(6.76698677596,-0.0133781158060973,28.3021909285745));
#16085=CARTESIAN_POINT('Ctrl Pts',(6.76735450854098,0.172630254029962,28.3109405101818));
#16086=CARTESIAN_POINT('Ctrl Pts',(6.76004850628286,0.358653651283843,28.3196900917891));
#16087=CARTESIAN_POINT('Ctrl Pts',(6.74509358473383,0.544060229370441,28.3284396733964));
#16088=CARTESIAN_POINT('Ctrl Pts',(6.73013891752283,0.729463654251187,28.3371891061998));
#16089=CARTESIAN_POINT('Ctrl Pts',(6.70753561437841,0.914249995282579,28.3459385390031));
#16090=CARTESIAN_POINT('Ctrl Pts',(6.67736044701224,1.09779162898819,28.3546879718065));
#16091=CARTESIAN_POINT('Ctrl Pts',(6.64718575273648,1.2813303851029,28.363437267435));
#16092=CARTESIAN_POINT('Ctrl Pts',(6.60943947828775,1.46362419016019,28.3721865630635));
#16093=CARTESIAN_POINT('Ctrl Pts',(6.56424982419094,1.64405390593169,28.380935858692));
#16094=CARTESIAN_POINT('Ctrl Pts',(6.5190608185409,1.82448103263563,28.389685028773));
#16095=CARTESIAN_POINT('Ctrl Pts',(6.46642871659859,2.00304384560883,28.3984341988539));
#16096=CARTESIAN_POINT('Ctrl Pts',(6.406532271625,2.17913589586042,28.4071833689349));
#16097=CARTESIAN_POINT('Ctrl Pts',(6.34663660655764,2.35522565323327,28.4159324250936));
#16098=CARTESIAN_POINT('Ctrl Pts',(6.27947688001376,2.52884444098845,28.4246814812524));
#16099=CARTESIAN_POINT('Ctrl Pts',(6.20528117917537,2.69940261676022,28.4334305374112));
#16100=CARTESIAN_POINT('Ctrl Pts',(6.12826427824231,2.8764460569907,28.4425122656491));
#16101=CARTESIAN_POINT('Ctrl Pts',(6.04366596008219,3.05019126379016,28.4515939938871));
#16102=CARTESIAN_POINT('Ctrl Pts',(5.95179577696798,3.22000248901552,28.4606757221251));
#16103=CARTESIAN_POINT('Ctrl Pts',(5.86328355867829,3.3836069113176,28.4694255023584));
#16104=CARTESIAN_POINT('Ctrl Pts',(5.76802179058685,3.54355957239308,28.4781752825917));
#16105=CARTESIAN_POINT('Ctrl Pts',(5.66633405324216,3.69931715280918,28.4869250628251));
#16106=CARTESIAN_POINT('Ctrl Pts',(5.56464997144232,3.85506913393835,28.4956745285149));
#16107=CARTESIAN_POINT('Ctrl Pts',(5.45654053933722,4.00662609619198,28.5044239942048));
#16108=CARTESIAN_POINT('Ctrl Pts',(5.34237295142181,4.15347327521397,28.5131734598946));
#16109=CARTESIAN_POINT('Ctrl Pts',(5.22820886081963,4.30031595584379,28.5219226575608));
#16110=CARTESIAN_POINT('Ctrl Pts',(5.10798716166375,4.44244891571258,28.5306718552269));
#16111=CARTESIAN_POINT('Ctrl Pts',(4.9821161628635,4.57938942870491,28.539421052893));
#16112=CARTESIAN_POINT('Ctrl Pts',(4.85624835096625,4.71632647452739,28.54817002904));
#16113=CARTESIAN_POINT('Ctrl Pts',(4.724731719552,4.84807112559724,28.5569190051869));
#16114=CARTESIAN_POINT('Ctrl Pts',(4.58801291590907,4.97417596024221,28.5656679813338));
#16115=CARTESIAN_POINT('Ctrl Pts',(4.45128522596351,5.10028899131442,28.5744175261373));
#16116=CARTESIAN_POINT('Ctrl Pts',(4.30935489779267,5.22076127807759,28.5831670709409));
#16117=CARTESIAN_POINT('Ctrl Pts',(4.16270400752698,5.33518362811617,28.5919166157444));
#16118=CARTESIAN_POINT('Ctrl Pts',(4.01606173721642,5.44959925255274,28.6006656462606));
#16119=CARTESIAN_POINT('Ctrl Pts',(3.86469968596859,5.55796547558829,28.6094146767769));
#16120=CARTESIAN_POINT('Ctrl Pts',(3.70913190503631,5.65991426711057,28.6181637072932));
#16121=CARTESIAN_POINT('Ctrl Pts',(3.55356201479594,5.76186444093327,28.6269128564356));
#16122=CARTESIAN_POINT('Ctrl Pts',(3.39378652042069,5.85739685205832,28.6356620055779));
#16123=CARTESIAN_POINT('Ctrl Pts',(3.23034806134602,5.94618704739079,28.6444111547203));
#16124=CARTESIAN_POINT('Ctrl Pts',(3.18687941281391,5.96980198977251,28.6467381081876));
#16125=CARTESIAN_POINT('Ctrl Pts',(3.14315180418704,5.99294025706453,28.6490650616548));
#16126=CARTESIAN_POINT('Ctrl Pts',(3.09917575053261,6.01559628526638,28.6513920151221));
#16127=CARTESIAN_POINT('Origin',(0.,0.,-3.69717978381041));
#16128=CARTESIAN_POINT('',(3.09917575053259,6.01559628526639,31.0457515827422));
#16129=CARTESIAN_POINT('',(3.09917575053255,6.01559628526641,30.6514573492524));
#16130=CARTESIAN_POINT('',(3.09917575053259,6.01559628526639,-3.69717978381041));
#16131=CARTESIAN_POINT('',(-6.767,1.20905997887111E-12,29.69717978381));
#16132=CARTESIAN_POINT('Ctrl Pts',(-6.767,1.20906028438136E-12,29.69717978381));
#16133=CARTESIAN_POINT('Ctrl Pts',(-6.76700000000003,-0.18600724941446,
29.705929295616));
#16134=CARTESIAN_POINT('Ctrl Pts',(-6.75932637295445,-0.372014355526306,
29.7146788074219));
#16135=CARTESIAN_POINT('Ctrl Pts',(-6.74400518266938,-0.557389537153815,
29.7234283192279));
#16136=CARTESIAN_POINT('Ctrl Pts',(-6.72868405709658,-0.742763935810295,
29.7321777940784));
#16137=CARTESIAN_POINT('Ctrl Pts',(-6.70571545653005,-0.927506129694064,
29.7409272689289));
#16138=CARTESIAN_POINT('Ctrl Pts',(-6.67517739415664,-1.11098863924892,
29.7496767437795));
#16139=CARTESIAN_POINT('Ctrl Pts',(-6.64463945823084,-1.29447038906586,
29.7584261824015));
#16140=CARTESIAN_POINT('Ctrl Pts',(-6.60653217027138,-1.47669218228305,
29.7671756210235));
#16141=CARTESIAN_POINT('Ctrl Pts',(-6.56098496116689,-1.65703510504212,
29.7759250596455));
#16142=CARTESIAN_POINT('Ctrl Pts',(-6.51543793687488,-1.83737729604125,
29.7846744627657));
#16143=CARTESIAN_POINT('Ctrl Pts',(-6.46245112202603,-2.0158403539717,29.7934238658859));
#16144=CARTESIAN_POINT('Ctrl Pts',(-6.40220448416198,-2.19181813638273,
29.8021732690062));
#16145=CARTESIAN_POINT('Ctrl Pts',(-6.34195808575137,-2.36779521936079,
29.8109226373514));
#16146=CARTESIAN_POINT('Ctrl Pts',(-6.27445201489178,-2.54128677544968,
29.8196720056967));
#16147=CARTESIAN_POINT('Ctrl Pts',(-6.1999155513612,-2.71170355237987,29.828421374042));
#16148=CARTESIAN_POINT('Ctrl Pts',(-6.12537937788967,-2.88211966613225,
29.8371707083391));
#16149=CARTESIAN_POINT('Ctrl Pts',(-6.04381298133537,-3.04946076210603,
29.8459200426361));
#16150=CARTESIAN_POINT('Ctrl Pts',(-5.95549339426218,-3.21315848207019,
29.8546693769332));
#16151=CARTESIAN_POINT('Ctrl Pts',(-5.86717414355064,-3.37685557859804,
29.8634186779087));
#16152=CARTESIAN_POINT('Ctrl Pts',(-5.77210188986133,-3.53690907467483,
29.8721679788843));
#16153=CARTESIAN_POINT('Ctrl Pts',(-5.67059953466954,-3.6927753678508,29.8809172798599));
#16154=CARTESIAN_POINT('Ctrl Pts',(-5.56909755761641,-3.84864108035974,
29.8896665482406));
#16155=CARTESIAN_POINT('Ctrl Pts',(-5.46116568337934,-4.00031938104466,
29.8984158166214));
#16156=CARTESIAN_POINT('Ctrl Pts',(-5.34717048685966,-4.1472951166341,29.9071650850022));
#16157=CARTESIAN_POINT('Ctrl Pts',(-5.23317570555366,-4.29427031688225,
29.9159143215148));
#16158=CARTESIAN_POINT('Ctrl Pts',(-5.1131178217865,-4.43654275987308,29.9246635580274));
#16159=CARTESIAN_POINT('Ctrl Pts',(-4.98740459171857,-4.57362924147821,
29.93341279454));
#16160=CARTESIAN_POINT('Ctrl Pts',(-4.86169180910672,-4.71071523514599,
29.9421619999111));
#16161=CARTESIAN_POINT('Ctrl Pts',(-4.73032391415273,-4.84261509316678,
29.9509112052823));
#16162=CARTESIAN_POINT('Ctrl Pts',(-4.59374707237136,-4.96888084331669,
29.9596604106534));
#16163=CARTESIAN_POINT('Ctrl Pts',(-4.4571707053724,-5.09514615452866,29.9684095856096));
#16164=CARTESIAN_POINT('Ctrl Pts',(-4.31538563819343,-5.2157772025377,29.9771587605658));
#16165=CARTESIAN_POINT('Ctrl Pts',(-4.16887341290477,-5.33036429028784,
29.9859079355221));
#16166=CARTESIAN_POINT('Ctrl Pts',(-4.02236168477174,-5.44495098921298,
29.99465708079));
#16167=CARTESIAN_POINT('Ctrl Pts',(-3.87112305634281,-5.55349359238869,
30.0034062260579));
#16168=CARTESIAN_POINT('Ctrl Pts',(-3.71567117316582,-5.65562346102572,
30.0121553713258));
#16169=CARTESIAN_POINT('Ctrl Pts',(-3.5602198045717,-5.75775299158849,30.0209044876319));
#16170=CARTESIAN_POINT('Ctrl Pts',(-3.40055544862277,-5.85346967275417,
30.0296536039381));
#16171=CARTESIAN_POINT('Ctrl Pts',(-3.23722036323314,-5.9424484280361,30.0384027202442));
#16172=CARTESIAN_POINT('Ctrl Pts',(-3.07388580495985,-6.03142689616506,
30.0471518083152));
#16173=CARTESIAN_POINT('Ctrl Pts',(-2.90688079257675,-6.11366734484837,
30.0559008963861));
#16174=CARTESIAN_POINT('Ctrl Pts',(-2.73677251094613,-6.18889046787303,
30.064649984457));
#16175=CARTESIAN_POINT('Ctrl Pts',(-2.56666476416645,-6.2641133543827,30.0733990450193));
#16176=CARTESIAN_POINT('Ctrl Pts',(-2.39345402972095,-6.3323188435029,30.0821481055815));
#16177=CARTESIAN_POINT('Ctrl Pts',(-2.21772856474042,-6.39327529621042,
30.0908971661437));
#16178=CARTESIAN_POINT('Ctrl Pts',(-2.04200363768294,-6.45423156232073,
30.0996461999237));
#16179=CARTESIAN_POINT('Ctrl Pts',(-1.86376426620139,-6.50793874252042,
30.1083952337037));
#16180=CARTESIAN_POINT('Ctrl Pts',(-1.68361578194756,-6.55421443796105,
30.1171442674837));
#16181=CARTESIAN_POINT('Ctrl Pts',(-1.50346783419914,-6.6004899955867,30.1258932752079));
#16182=CARTESIAN_POINT('Ctrl Pts',(-1.32141106257271,-6.63933404145491,
30.1346422829322));
#16183=CARTESIAN_POINT('Ctrl Pts',(-1.13806375959047,-6.67061465527029,
30.1433912906564));
#16184=CARTESIAN_POINT('Ctrl Pts',(-0.954716987419053,-6.70189517852482,
30.1521402730513));
#16185=CARTESIAN_POINT('Ctrl Pts',(-0.770079973809654,-6.72561226535831,
30.1608892554462));
#16186=CARTESIAN_POINT('Ctrl Pts',(-0.584779770552109,-6.74168536939785,
30.1696382378411));
#16187=CARTESIAN_POINT('Ctrl Pts',(-0.391490647553584,-6.75845143942396,
30.1787644185171));
#16188=CARTESIAN_POINT('Ctrl Pts',(-0.197480213104026,-6.76689975924027,
30.1878905991932));
#16189=CARTESIAN_POINT('Ctrl Pts',(-0.00346532629750826,-6.76699911271707,
30.1970167798692));
#16190=CARTESIAN_POINT('Ctrl Pts',(0.184486595296305,-6.76709536139773,
30.2058577673992));
#16191=CARTESIAN_POINT('Ctrl Pts',(0.372442378185438,-6.75935659726769,
30.2146987549291));
#16192=CARTESIAN_POINT('Ctrl Pts',(0.559750217722256,-6.74380965729015,
30.223539742459));
#16193=CARTESIAN_POINT('Ctrl Pts',(0.745129914457859,-6.72842275717252,
30.2322897210568));
#16194=CARTESIAN_POINT('Ctrl Pts',(0.929874656314225,-6.70538772273472,
30.2410396996545));
#16195=CARTESIAN_POINT('Ctrl Pts',(1.11335688289775,-6.67478280180743,30.2497896782523));
#16196=CARTESIAN_POINT('Ctrl Pts',(1.29683723118851,-6.64417819418024,30.2585395672773));
#16197=CARTESIAN_POINT('Ctrl Pts',(1.47905480730225,-6.60600390230077,30.2672894563022));
#16198=CARTESIAN_POINT('Ctrl Pts',(1.65939064804795,-6.56038959797138,30.2760393453271));
#16199=CARTESIAN_POINT('Ctrl Pts',(1.83972470264242,-6.51477574543262,30.2847891476881));
#16200=CARTESIAN_POINT('Ctrl Pts',(2.01817678125815,-6.4617220982011,30.293538950049));
#16201=CARTESIAN_POINT('Ctrl Pts',(2.19414072347636,-6.40140886724029,30.30228875241));
#16202=CARTESIAN_POINT('Ctrl Pts',(2.37010298132055,-6.3410962136139,30.3110384710154));
#16203=CARTESIAN_POINT('Ctrl Pts',(2.54357687926873,-6.27352420825987,30.3197881896209));
#16204=CARTESIAN_POINT('Ctrl Pts',(2.71397317789932,-6.19892237325513,30.3285379082264));
#16205=CARTESIAN_POINT('Ctrl Pts',(2.88436790207167,-6.12432122756979,30.3372875459847));
#16206=CARTESIAN_POINT('Ctrl Pts',(3.05168482126228,-6.04269049717432,30.346037183743));
#16207=CARTESIAN_POINT('Ctrl Pts',(3.21535561997365,-5.95430745234942,30.3547868215012));
#16208=CARTESIAN_POINT('Ctrl Pts',(3.37902496075248,-5.86592519481535,30.3635363813202));
#16209=CARTESIAN_POINT('Ctrl Pts',(3.53904799384833,-5.77079087940257,30.3722859411392));
#16210=CARTESIAN_POINT('Ctrl Pts',(3.69488118814934,-5.66922763747057,30.3810355009583));
#16211=CARTESIAN_POINT('Ctrl Pts',(3.85071304610783,-5.56766526649086,30.3897849857457));
#16212=CARTESIAN_POINT('Ctrl Pts',(4.00235489705919,-5.4596742358075,30.3985344705331));
#16213=CARTESIAN_POINT('Ctrl Pts',(4.14929168607605,-5.34562133936366,30.4072839553206));
#16214=CARTESIAN_POINT('Ctrl Pts',(4.29622726385707,-5.23156938308572,30.4160333679839));
#16215=CARTESIAN_POINT('Ctrl Pts',(4.43845763092016,-5.11145583677246,30.4247827806472));
#16216=CARTESIAN_POINT('Ctrl Pts',(4.5754997066091,-4.98568866204259,30.4335321933105));
#16217=CARTESIAN_POINT('Ctrl Pts',(4.7125406981524,-4.85992248226215,30.4422815367568));
#16218=CARTESIAN_POINT('Ctrl Pts',(4.84439326931256,-4.72850295734061,30.4510308802031));
#16219=CARTESIAN_POINT('Ctrl Pts',(4.97060959434638,-4.59187644221747,30.4597802236494));
#16220=CARTESIAN_POINT('Ctrl Pts',(5.09682496280455,-4.45525096256732,30.4685295007857));
#16221=CARTESIAN_POINT('Ctrl Pts',(5.21740397615779,-4.31341878218398,30.477278777922));
#16222=CARTESIAN_POINT('Ctrl Pts',(5.33193710451875,-4.16686161438753,30.4860280550583));
#16223=CARTESIAN_POINT('Ctrl Pts',(5.44646940289336,-4.02030550864578,30.4947772687913));
#16224=CARTESIAN_POINT('Ctrl Pts',(5.55495572749629,-3.86902470980185,30.5035264825242));
#16225=CARTESIAN_POINT('Ctrl Pts',(5.65702762491431,-3.7135330146582,30.5122756962572));
#16226=CARTESIAN_POINT('Ctrl Pts',(5.7590988165514,-3.55804239466916,30.5210248494933));
#16227=CARTESIAN_POINT('Ctrl Pts',(5.85475551250779,-3.3983411761956,30.5297740027295));
#16228=CARTESIAN_POINT('Ctrl Pts',(5.943672837281,-3.2349717469196,30.5385231559656));
#16229=CARTESIAN_POINT('Ctrl Pts',(6.03258957676317,-3.07160339300955,30.5472722516111));
#16230=CARTESIAN_POINT('Ctrl Pts',(6.1147668968529,-2.90456712829493,30.5560213472567));
#16231=CARTESIAN_POINT('Ctrl Pts',(6.18992570525266,-2.73443024475892,30.5647704429022));
#16232=CARTESIAN_POINT('Ctrl Pts',(6.265084043887,-2.56429442463023,30.5735194838632));
#16233=CARTESIAN_POINT('Ctrl Pts',(6.33322384283315,-2.39105828655991,30.5822685248242));
#16234=CARTESIAN_POINT('Ctrl Pts',(6.39411368720031,-2.21531017132086,30.5910175657853));
#16235=CARTESIAN_POINT('Ctrl Pts',(6.45500317120888,-2.0395630961952,30.5997665549677));
#16236=CARTESIAN_POINT('Ctrl Pts',(6.50864269270072,-1.86130434438638,30.6085155441501));
#16237=CARTESIAN_POINT('Ctrl Pts',(6.55485008446332,-1.6811393071995,30.6172645333325));
#16238=CARTESIAN_POINT('Ctrl Pts',(6.60199664749403,-1.49731239211843,30.6261913468619));
#16239=CARTESIAN_POINT('Ctrl Pts',(6.64140563640906,-1.31150116499672,30.6351181603912));
#16240=CARTESIAN_POINT('Ctrl Pts',(6.67293772282172,-1.12436255155659,30.6440449739206));
#16241=CARTESIAN_POINT('Ctrl Pts',(6.70384494949871,-0.940932395051362,
30.6527948880761));
#16242=CARTESIAN_POINT('Ctrl Pts',(6.7271844934893,-0.75622726050676,30.6615448022316));
#16243=CARTESIAN_POINT('Ctrl Pts',(6.74287707373931,-0.570874564541765,
30.6702947163872));
#16244=CARTESIAN_POINT('Ctrl Pts',(6.7585693453867,-0.385525513632534,30.6790444584711));
#16245=CARTESIAN_POINT('Ctrl Pts',(6.76661493004103,-0.199529212418273,
30.6877942005551));
#16246=CARTESIAN_POINT('Ctrl Pts',(6.76698649908907,-0.0135174386004552,
30.6965439426391));
#16247=CARTESIAN_POINT('Ctrl Pts',(6.76735806132389,0.172490924445765,30.705293524285));
#16248=CARTESIAN_POINT('Ctrl Pts',(6.76005588896289,0.358514472901408,30.7140431059309));
#16249=CARTESIAN_POINT('Ctrl Pts',(6.74510478454584,0.543921359662228,30.7227926875768));
#16250=CARTESIAN_POINT('Ctrl Pts',(6.73015393440687,0.729325093150549,30.7315421204158));
#16251=CARTESIAN_POINT('Ctrl Pts',(6.70755443556895,0.914111900256543,30.7402915532549));
#16252=CARTESIAN_POINT('Ctrl Pts',(6.67738304682314,1.09765415591566,30.7490409860939));
#16253=CARTESIAN_POINT('Ctrl Pts',(6.64721213111855,1.28119353391299,30.7577902817553));
#16254=CARTESIAN_POINT('Ctrl Pts',(6.60946960955489,1.46348811672678,30.7665395774166));
#16255=CARTESIAN_POINT('Ctrl Pts',(6.56428366991177,1.64391876348245,30.7752888730779));
#16256=CARTESIAN_POINT('Ctrl Pts',(6.51909837867709,1.82434682109748,30.7840380431887));
#16257=CARTESIAN_POINT('Ctrl Pts',(6.46646995271908,2.00291071820487,30.7927872132996));
#16258=CARTESIAN_POINT('Ctrl Pts',(6.40657713281532,2.17900400212755,30.8015363834104));
#16259=CARTESIAN_POINT('Ctrl Pts',(6.3466850927904,2.35509499309711,30.8102854395962));
#16260=CARTESIAN_POINT('Ctrl Pts',(6.27952894037504,2.52871516398177,30.819034495782));
#16261=CARTESIAN_POINT('Ctrl Pts',(6.20533675061422,2.69927486771476,30.8277835519677));
#16262=CARTESIAN_POINT('Ctrl Pts',(6.12832117907893,2.87632521635974,30.83686555325));
#16263=CARTESIAN_POINT('Ctrl Pts',(6.04372366626056,3.05007728920043,30.8459475545323));
#16264=CARTESIAN_POINT('Ctrl Pts',(5.95185378007846,3.21989527478236,30.8550295558145));
#16265=CARTESIAN_POINT('Ctrl Pts',(5.86334450817347,3.38350129286793,30.8637793361217));
#16266=CARTESIAN_POINT('Ctrl Pts',(5.7680856205723,3.54345567125004,30.8725291164288));
#16267=CARTESIAN_POINT('Ctrl Pts',(5.66640068804456,3.69921508465352,30.8812788967359));
#16268=CARTESIAN_POINT('Ctrl Pts',(5.56471941107894,3.85496889852325,30.8900283624894));
#16269=CARTESIAN_POINT('Ctrl Pts',(5.45661270815084,4.00652780919678,30.8987778282429));
#16270=CARTESIAN_POINT('Ctrl Pts',(5.34244776449083,4.15337704569269,30.9075272939964));
#16271=CARTESIAN_POINT('Ctrl Pts',(5.22828631819568,4.30022178356283,30.916276491716));
#16272=CARTESIAN_POINT('Ctrl Pts',(5.10806717844046,4.44235690972705,30.9250256894356));
#16273=CARTESIAN_POINT('Ctrl Pts',(4.98219864544701,4.57929969070665,30.9337748871551));
#16274=CARTESIAN_POINT('Ctrl Pts',(4.85633329944005,4.71623900430022,30.9425238633454));
#16275=CARTESIAN_POINT('Ctrl Pts',(4.72481904033626,4.84798602483638,30.9512728395356));
#16276=CARTESIAN_POINT('Ctrl Pts',(4.58810250737175,4.97409332259147,30.9600218157259));
#16277=CARTESIAN_POINT('Ctrl Pts',(4.45137708685615,5.10020881822159,30.968771360662));
#16278=CARTESIAN_POINT('Ctrl Pts',(4.3094489263602,5.22068366307959,30.9775209055982));
#16279=CARTESIAN_POINT('Ctrl Pts',(4.16280009466626,5.33510865604878,30.9862704505344));
#16280=CARTESIAN_POINT('Ctrl Pts',(4.01615988348752,5.44952692272918,30.9950194811427));
#16281=CARTESIAN_POINT('Ctrl Pts',(3.86479978232193,5.55789587288653,31.0037685117509));
#16282=CARTESIAN_POINT('Ctrl Pts',(3.70923383581028,5.65984746713904,31.0125175423592));
#16283=CARTESIAN_POINT('Ctrl Pts',(3.55366577799506,5.76180044505404,31.0212666917072));
#16284=CARTESIAN_POINT('Ctrl Pts',(3.3938920002681,5.85733573571076,31.0300158410553));
#16285=CARTESIAN_POINT('Ctrl Pts',(3.23045513626017,5.94612887621941,31.0387649904033));
#16286=CARTESIAN_POINT('Ctrl Pts',(3.18695122151562,5.96976399206697,31.0410938545162));
#16287=CARTESIAN_POINT('Ctrl Pts',(3.14318791262656,5.99292165435337,31.0434227186292));
#16288=CARTESIAN_POINT('Ctrl Pts',(3.09917575053259,6.01559628526639,31.0457515827422));
#16289=CARTESIAN_POINT('Ctrl Pts',(3.09917575053261,6.01559628526638,29.0458547647091));
#16290=CARTESIAN_POINT('Ctrl Pts',(2.9439648467836,6.09555940883824,29.0540509860553));
#16291=CARTESIAN_POINT('Ctrl Pts',(2.78559192492888,6.1695453142795,29.0622472074014));
#16292=CARTESIAN_POINT('Ctrl Pts',(2.62455973683121,6.23730512223064,29.0704434287475));
#16293=CARTESIAN_POINT('Ctrl Pts',(2.46353786135157,6.30506059079456,29.0786391252017));
#16294=CARTESIAN_POINT('Ctrl Pts',(2.29985738630005,6.36659060972087,29.0868348216559));
#16295=CARTESIAN_POINT('Ctrl Pts',(2.13404236957982,6.42169387037705,29.09503051811));
#16296=CARTESIAN_POINT('Ctrl Pts',(1.96822457599583,6.47679805383413,29.1032263518155));
#16297=CARTESIAN_POINT('Ctrl Pts',(1.8002725099202,6.52547515085438,29.111422185521));
#16298=CARTESIAN_POINT('Ctrl Pts',(1.63072665516705,6.5675733399885,29.1196180192265));
#16299=CARTESIAN_POINT('Ctrl Pts',(1.46114711416693,6.60967989340848,29.1278154813227));
#16300=CARTESIAN_POINT('Ctrl Pts',(1.2899735019906,6.64520484872491,29.1360129434188));
#16301=CARTESIAN_POINT('Ctrl Pts',(1.11775783933176,6.67404722882693,29.1442104055149));
#16302=CARTESIAN_POINT('Ctrl Pts',(0.945476627084163,6.70290058706023,29.1524109877701));
#16303=CARTESIAN_POINT('Ctrl Pts',(0.772152927961196,6.72506624441566,29.1606115700254));
#16304=CARTESIAN_POINT('Ctrl Pts',(0.598345299828283,6.74049493006066,29.1688121522806));
#16305=CARTESIAN_POINT('Ctrl Pts',(0.424350213897592,6.75594025609978,29.1770215791596));
#16306=CARTESIAN_POINT('Ctrl Pts',(0.249870514114099,6.76463406695162,29.1852310060387));
#16307=CARTESIAN_POINT('Ctrl Pts',(0.0754671020344008,6.76657917388916,
29.1934404329178));
#16308=CARTESIAN_POINT('Ctrl Pts',(-0.0990439248821634,6.76852548104615,
29.2016549253866));
#16309=CARTESIAN_POINT('Ctrl Pts',(-0.273478212496277,6.76371479392963,
29.2098694178554));
#16310=CARTESIAN_POINT('Ctrl Pts',(-0.447278673085257,6.75220192149221,
29.2180839103242));
#16311=CARTESIAN_POINT('Ctrl Pts',(-0.621311993572233,6.74067362397311,
29.2263094086665));
#16312=CARTESIAN_POINT('Ctrl Pts',(-0.794709435215398,6.72242524414566,
29.2345349070087));
#16313=CARTESIAN_POINT('Ctrl Pts',(-0.966921867799625,6.6975630718621,29.242760405351));
#16314=CARTESIAN_POINT('Ctrl Pts',(-1.04025487874001,6.68697604324452,29.2462630593166));
#16315=CARTESIAN_POINT('Ctrl Pts',(-1.11337316883411,6.67519036143643,29.2497657132823));
#16316=CARTESIAN_POINT('Ctrl Pts',(-1.18623513486506,6.66221698872167,29.2532683672479));
#16317=CARTESIAN_POINT('Ctrl Pts',(-1.35732786195949,6.63175322500115,29.26149321557));
#16318=CARTESIAN_POINT('Ctrl Pts',(-1.52748644973448,6.59465170857477,29.269718063892));
#16319=CARTESIAN_POINT('Ctrl Pts',(-1.69615713523828,6.55098007725411,29.277942912214));
#16320=CARTESIAN_POINT('Ctrl Pts',(-1.86463786015288,6.50735762987311,29.2861584975332));
#16321=CARTESIAN_POINT('Ctrl Pts',(-2.03163367540517,6.45717989081006,29.2943740828525));
#16322=CARTESIAN_POINT('Ctrl Pts',(-2.19659849373558,6.40056591695755,29.3025896681717));
#16323=CARTESIAN_POINT('Ctrl Pts',(-2.36141066982093,6.34400432811753,29.310797651595));
#16324=CARTESIAN_POINT('Ctrl Pts',(-2.52419525441327,6.28101848063391,29.3190056350182));
#16325=CARTESIAN_POINT('Ctrl Pts',(-2.68441878475981,6.21177790878173,29.3272136184415));
#16326=CARTESIAN_POINT('Ctrl Pts',(-2.84452624169426,6.14258749803517,29.335415655618));
#16327=CARTESIAN_POINT('Ctrl Pts',(-3.00207601188468,6.06715152999008,29.3436176927945));
#16328=CARTESIAN_POINT('Ctrl Pts',(-3.15655208945124,5.98568859084576,29.3518197299711));
#16329=CARTESIAN_POINT('Ctrl Pts',(-3.31094727749595,5.90426830878011,29.3600174722504));
#16330=CARTESIAN_POINT('Ctrl Pts',(-3.46227166270541,5.81682750973103,29.3682152145298));
#16331=CARTESIAN_POINT('Ctrl Pts',(-3.61003136459167,5.72363193668709,29.3764129568092));
#16332=CARTESIAN_POINT('Ctrl Pts',(-3.75776297241603,5.63045408323899,29.3846091404236));
#16333=CARTESIAN_POINT('Ctrl Pts',(-3.90193094046812,5.5315238211852,29.3928053240379));
#16334=CARTESIAN_POINT('Ctrl Pts',(-4.04206778836664,5.42715183077172,29.4010015076523));
#16335=CARTESIAN_POINT('Ctrl Pts',(-4.18219432023783,5.32278752359302,29.4091970879132));
#16336=CARTESIAN_POINT('Ctrl Pts',(-4.31829003462124,5.21298249944986,29.4173926681741));
#16337=CARTESIAN_POINT('Ctrl Pts',(-4.44991819542317,5.09808954943338,29.4255882484349));
#16338=CARTESIAN_POINT('Ctrl Pts',(-4.58156061474275,4.98318415372787,29.4337847164757));
#16339=CARTESIAN_POINT('Ctrl Pts',(-4.70873424592737,4.86318997011062,29.4419811845164));
#16340=CARTESIAN_POINT('Ctrl Pts',(-4.831037045668,4.73849871408482,29.4501776525571));
#16341=CARTESIAN_POINT('Ctrl Pts',(-4.95337534540559,4.61377126478118,29.4583764997305));
#16342=CARTESIAN_POINT('Ctrl Pts',(-5.07083974634128,4.48434428348448,29.4665753469039));
#16343=CARTESIAN_POINT('Ctrl Pts',(-5.18306650837798,4.35064484527645,29.4747741940773));
#16344=CARTESIAN_POINT('Ctrl Pts',(-5.29541055829393,4.21680567815457,29.4829816098433));
#16345=CARTESIAN_POINT('Ctrl Pts',(-5.40250580228175,4.07868540857729,29.4911890256093));
#16346=CARTESIAN_POINT('Ctrl Pts',(-5.50402949796317,3.93674336038702,29.4993964413752));
#16347=CARTESIAN_POINT('Ctrl Pts',(-5.60560760677499,3.79472523625088,29.5076082560274));
#16348=CARTESIAN_POINT('Ctrl Pts',(-5.70160801720471,3.64888154952859,29.5158200706796));
#16349=CARTESIAN_POINT('Ctrl Pts',(-5.79175255353429,3.49969875255415,29.5240318853317));
#16350=CARTESIAN_POINT('Ctrl Pts',(-5.88202984139744,3.3502962612323,29.5322557931293));
#16351=CARTESIAN_POINT('Ctrl Pts',(-5.96643384746372,3.19754514655468,29.540479700927));
#16352=CARTESIAN_POINT('Ctrl Pts',(-6.04473281708655,3.04195564892667,29.5487036087246));
#16353=CARTESIAN_POINT('Ctrl Pts',(-6.1170796189689,2.89819382659247,29.5563023476479));
#16354=CARTESIAN_POINT('Ctrl Pts',(-6.18421473488204,2.75200919431501,29.5639010865713));
#16355=CARTESIAN_POINT('Ctrl Pts',(-6.24599284241516,2.60381689304347,29.5714998254947));
#16356=CARTESIAN_POINT('Ctrl Pts',(-6.31984132294676,2.42667038091511,29.5805832264899));
#16357=CARTESIAN_POINT('Ctrl Pts',(-6.38622117172981,2.2462088131756,29.589666627485));
#16358=CARTESIAN_POINT('Ctrl Pts',(-6.44485266720639,2.06304704212065,29.5987500284802));
#16359=CARTESIAN_POINT('Ctrl Pts',(-6.50324037875175,1.88064683950657,29.6077956615968));
#16360=CARTESIAN_POINT('Ctrl Pts',(-6.5539439232451,1.69556904279107,29.6168412947134));
#16361=CARTESIAN_POINT('Ctrl Pts',(-6.59673275028268,1.50844490166128,29.62588692783));
#16362=CARTESIAN_POINT('Ctrl Pts',(-6.63940881009013,1.32181391429492,29.6349087217562));
#16363=CARTESIAN_POINT('Ctrl Pts',(-6.67421169874369,1.13314755734616,29.6439305156825));
#16364=CARTESIAN_POINT('Ctrl Pts',(-6.70095996871385,0.943093048269617,
29.6529523096087));
#16365=CARTESIAN_POINT('Ctrl Pts',(-6.72759269831094,0.753859488320121,
29.6619351334843));
#16366=CARTESIAN_POINT('Ctrl Pts',(-6.74624015093949,0.563249957731145,
29.6709179573599));
#16367=CARTESIAN_POINT('Ctrl Pts',(-6.75677169811228,0.371920985679566,
29.6799007812355));
#16368=CARTESIAN_POINT('Ctrl Pts',(-6.76352438647371,0.249243386502655,
29.6856604487603));
#16369=CARTESIAN_POINT('Ctrl Pts',(-6.76694144236585,0.126270358197117,
29.6914201162852));
#16370=CARTESIAN_POINT('Ctrl Pts',(-6.76699925367029,0.0031781796254976,
29.69717978381));
#16371=CARTESIAN_POINT('',(-6.767,1.13258374575577E-12,29.3028202161899));
#16372=CARTESIAN_POINT('Ctrl Pts',(3.09917575053261,6.01559628526638,28.6513920151221));
#16373=CARTESIAN_POINT('Ctrl Pts',(2.93382384459268,6.10078395293758,28.6601414630345));
#16374=CARTESIAN_POINT('Ctrl Pts',(2.76495772122988,6.17915010267047,28.6688909109469));
#16375=CARTESIAN_POINT('Ctrl Pts',(2.59315093316716,6.25042856433175,28.6776403588593));
#16376=CARTESIAN_POINT('Ctrl Pts',(2.42134553245622,6.32170645041449,28.6863897361193));
#16377=CARTESIAN_POINT('Ctrl Pts',(2.24659977927595,6.38589665313456,28.6951391133793));
#16378=CARTESIAN_POINT('Ctrl Pts',(2.06950718689923,6.44278115439074,28.7038884906393));
#16379=CARTESIAN_POINT('Ctrl Pts',(1.89241596572865,6.49966521519723,28.712637800154));
#16380=CARTESIAN_POINT('Ctrl Pts',(1.71297821457201,6.54924360009545,28.7213871096686));
#16381=CARTESIAN_POINT('Ctrl Pts',(1.53180337335847,6.59134792173556,28.7301364191833));
#16382=CARTESIAN_POINT('Ctrl Pts',(1.35062987477779,6.63345193135306,28.7388856638594));
#16383=CARTESIAN_POINT('Ctrl Pts',(1.16771959102942,6.6680819236824,28.7476349085355));
#16384=CARTESIAN_POINT('Ctrl Pts',(0.983693746906687,6.69512028363171,28.7563841532116));
#16385=CARTESIAN_POINT('Ctrl Pts',(0.799669205419707,6.72215845218869,28.7651333359558));
#16386=CARTESIAN_POINT('Ctrl Pts',(0.614529402873306,6.74160505424581,28.7738825187));
#16387=CARTESIAN_POINT('Ctrl Pts',(0.428903127363072,6.75339404354123,28.7826317014442));
#16388=CARTESIAN_POINT('Ctrl Pts',(0.243278104163657,6.76518295330331,28.7913808251628));
#16389=CARTESIAN_POINT('Ctrl Pts',(0.0571669005388484,6.76931433552276,
28.8001299488814));
#16390=CARTESIAN_POINT('Ctrl Pts',(-0.128798404777828,6.76577415902472,
28.8088790726));
#16391=CARTESIAN_POINT('Ctrl Pts',(-0.314762517259509,6.7622340052344,28.8176281401992));
#16392=CARTESIAN_POINT('Ctrl Pts',(-0.500580446820015,6.75102239665086,
28.8263772077984));
#16393=CARTESIAN_POINT('Ctrl Pts',(-0.68562111884321,6.73217741012491,28.8351262753976));
#16394=CARTESIAN_POINT('Ctrl Pts',(-0.870660665414947,6.71333253821765,
28.8438752897834));
#16395=CARTESIAN_POINT('Ctrl Pts',(-1.05492267885519,6.68685441030607,28.8526243041692));
#16396=CARTESIAN_POINT('Ctrl Pts',(-1.2377813763527,6.65283295028174,28.861373318555));
#16397=CARTESIAN_POINT('Ctrl Pts',(-1.42999922978866,6.61707018861861,28.8705701289224));
#16398=CARTESIAN_POINT('Ctrl Pts',(-1.62066601233715,6.57297172934408,28.8797669392898));
#16399=CARTESIAN_POINT('Ctrl Pts',(-1.80906628500406,6.52070304311288,28.8889637496572));
#16400=CARTESIAN_POINT('Ctrl Pts',(-1.98831342545545,6.47097374915025,28.8977137473949));
#16401=CARTESIAN_POINT('Ctrl Pts',(-2.16550875896717,6.41384933989523,28.9064637451327));
#16402=CARTESIAN_POINT('Ctrl Pts',(-2.34005036714024,6.34952386240471,28.9152137428704));
#16403=CARTESIAN_POINT('Ctrl Pts',(-2.51458843547097,6.28519968948593,28.9239635631513));
#16404=CARTESIAN_POINT('Ctrl Pts',(-2.6864726171806,6.21367483971097,28.9327133834322));
#16405=CARTESIAN_POINT('Ctrl Pts',(-2.85511905908732,6.13519226743843,28.941463203713));
#16406=CARTESIAN_POINT('Ctrl Pts',(-3.02376230488879,6.0567111825294,28.9502128581716));
#16407=CARTESIAN_POINT('Ctrl Pts',(-3.18916767379893,5.97127275992639,28.9589625126301));
#16408=CARTESIAN_POINT('Ctrl Pts',(-3.3507733410277,5.87916720438006,28.9677121670886));
#16409=CARTESIAN_POINT('Ctrl Pts',(-3.51237616037351,5.78706327195653,28.9764616673571));
#16410=CARTESIAN_POINT('Ctrl Pts',(-3.67017916302283,5.68829258362309,28.9852111676255));
#16411=CARTESIAN_POINT('Ctrl Pts',(-3.82364636566446,5.58319061741053,28.9939606678939));
#16412=CARTESIAN_POINT('Ctrl Pts',(-3.97711106778796,5.47809036367704,29.0027100256024));
#16413=CARTESIAN_POINT('Ctrl Pts',(-4.12623987481938,5.36665920043217,29.0114593833108));
#16414=CARTESIAN_POINT('Ctrl Pts',(-4.27052628213953,5.24927559512316,29.0202087410193));
#16415=CARTESIAN_POINT('Ctrl Pts',(-4.41481053025014,5.13189374643006,29.0289579677958));
#16416=CARTESIAN_POINT('Ctrl Pts',(-4.55425230136578,5.0085598147731,29.0377071945723));
#16417=CARTESIAN_POINT('Ctrl Pts',(-4.68837800630607,4.8796926819202,29.0464564213489));
#16418=CARTESIAN_POINT('Ctrl Pts',(-4.8225018822896,4.75082730631744,29.0552055288197));
#16419=CARTESIAN_POINT('Ctrl Pts',(-4.95130963053038,4.61642907903449,29.0639546362905));
#16420=CARTESIAN_POINT('Ctrl Pts',(-5.07436379033444,4.47695444731602,29.0727037437614));
#16421=CARTESIAN_POINT('Ctrl Pts',(-5.197416435629,4.33748153220474,29.0814527435512));
#16422=CARTESIAN_POINT('Ctrl Pts',(-5.31471544462883,4.19293255254451,29.0902017433409));
#16423=CARTESIAN_POINT('Ctrl Pts',(-5.4258624527575,4.04379841779438,29.0989507431307));
#16424=CARTESIAN_POINT('Ctrl Pts',(-5.53702160019268,3.89464799484178,29.1077006984728));
#16425=CARTESIAN_POINT('Ctrl Pts',(-5.6420272308136,3.74091164443686,29.116450653815));
#16426=CARTESIAN_POINT('Ctrl Pts',(-5.74052265233068,3.5831115916307,29.1252006091571));
#16427=CARTESIAN_POINT('Ctrl Pts',(-5.83901427067014,3.42531763191619,29.1339502266396));
#16428=CARTESIAN_POINT('Ctrl Pts',(-5.93099603115831,3.26346052695447,29.142699844122));
#16429=CARTESIAN_POINT('Ctrl Pts',(-6.0161555062284,3.09809004466909,29.1514494616045));
#16430=CARTESIAN_POINT('Ctrl Pts',(-6.10131214578882,2.93272506863655,29.1601987877556));
#16431=CARTESIAN_POINT('Ctrl Pts',(-6.17964682328827,2.76384720416716,29.1689481139067));
#16432=CARTESIAN_POINT('Ctrl Pts',(-6.2508934828864,2.5920300279141,29.1776974400578));
#16433=CARTESIAN_POINT('Ctrl Pts',(-6.32213814889399,2.4202176593685,29.1864465213893));
#16434=CARTESIAN_POINT('Ctrl Pts',(-6.38629508412646,2.24546640831743,29.1951956027209));
#16435=CARTESIAN_POINT('Ctrl Pts',(-6.44314639819866,2.06836976659872,29.2039446840525));
#16436=CARTESIAN_POINT('Ctrl Pts',(-6.5000028528375,1.89125711158105,29.2126945564869));
#16437=CARTESIAN_POINT('Ctrl Pts',(-6.54955227673294,1.71179891440083,29.2214444289213));
#16438=CARTESIAN_POINT('Ctrl Pts',(-6.59162635926425,1.53060476278259,29.2301943013557));
#16439=CARTESIAN_POINT('Ctrl Pts',(-6.63369752055233,1.34942319164515,29.2389435662782));
#16440=CARTESIAN_POINT('Ctrl Pts',(-6.66829431424287,1.16650618642515,29.2476928312007));
#16441=CARTESIAN_POINT('Ctrl Pts',(-6.69529923745446,0.98247499761658,29.2564420961232));
#16442=CARTESIAN_POINT('Ctrl Pts',(-6.72230554731467,0.798434359175782,
29.2651918103029));
#16443=CARTESIAN_POINT('Ctrl Pts',(-6.74171916496721,0.613279706238397,
29.2739415244826));
#16444=CARTESIAN_POINT('Ctrl Pts',(-6.75347414817287,0.427639953653461,
29.2826912386623));
#16445=CARTESIAN_POINT('Ctrl Pts',(-6.76248837758749,0.285283364197147,
29.2894008978381));
#16446=CARTESIAN_POINT('Ctrl Pts',(-6.76699999999998,0.142641701104186,
29.296110557014));
#16447=CARTESIAN_POINT('Ctrl Pts',(-6.767,1.13258377759989E-12,29.3028202161899));
#16448=CARTESIAN_POINT('Ctrl Pts',(-6.7669999999775,1.74501576113346E-5,
29.303194762523));
#16449=CARTESIAN_POINT('Ctrl Pts',(-6.76700043912407,-0.170279283280337,
29.3112153743689));
#16450=CARTESIAN_POINT('Ctrl Pts',(-6.76056808912486,-0.340797073679393,
29.3192359862148));
#16451=CARTESIAN_POINT('Ctrl Pts',(-6.74767885333058,-0.51099813337755,
29.3272565980607));
#16452=CARTESIAN_POINT('Ctrl Pts',(-6.73479999248599,-0.68106219291069,
29.3352707538648));
#16453=CARTESIAN_POINT('Ctrl Pts',(-6.71547461738373,-0.850809655833912,
29.343284909669));
#16454=CARTESIAN_POINT('Ctrl Pts',(-6.68973068447703,-1.01970209824563,
29.3512990654731));
#16455=CARTESIAN_POINT('Ctrl Pts',(-6.66400175719607,-1.18849609661654,
29.3593085499854));
#16456=CARTESIAN_POINT('Ctrl Pts',(-6.63186177571983,-1.3564356954542,29.3673180344978));
#16457=CARTESIAN_POINT('Ctrl Pts',(-6.59339057337646,-1.52298711317939,
29.3753275190101));
#16458=CARTESIAN_POINT('Ctrl Pts',(-6.55492856997583,-1.68949870639008,
29.3833350883551));
#16459=CARTESIAN_POINT('Ctrl Pts',(-6.5101384373662,-1.8546224113429,29.3913426577001));
#16460=CARTESIAN_POINT('Ctrl Pts',(-6.45915121506458,-2.01783413117376,
29.3993502270452));
#16461=CARTESIAN_POINT('Ctrl Pts',(-6.40816847654063,-2.18103149828973,
29.4073570922106));
#16462=CARTESIAN_POINT('Ctrl Pts',(-6.35098984433623,-2.34231685517073,
29.415363957376));
#16463=CARTESIAN_POINT('Ctrl Pts',(-6.28779630693183,-2.50118104153508,
29.4233708225415));
#16464=CARTESIAN_POINT('Ctrl Pts',(-6.22459563317648,-2.66006316819256,
29.4313785919101));
#16465=CARTESIAN_POINT('Ctrl Pts',(-6.15537884183735,-2.81652323027482,
29.4393863612788));
#16466=CARTESIAN_POINT('Ctrl Pts',(-6.08037508791807,-2.9700720176833,29.4473941306474));
#16467=CARTESIAN_POINT('Ctrl Pts',(-6.00534779332565,-3.12366899790382,
29.455404413334));
#16468=CARTESIAN_POINT('Ctrl Pts',(-5.92453008738743,-3.27435254718969,
29.4634146960207));
#16469=CARTESIAN_POINT('Ctrl Pts',(-5.83819699347893,-3.42165820404867,
29.4714249787073));
#16470=CARTESIAN_POINT('Ctrl Pts',(-5.75177343064882,-3.56911822331169,
29.479443655413));
#16471=CARTESIAN_POINT('Ctrl Pts',(-5.65982313140622,-3.71319295820093,
29.4874623321186));
#16472=CARTESIAN_POINT('Ctrl Pts',(-5.56266471935812,-3.85344653784226,
29.4954810088243));
#16473=CARTESIAN_POINT('Ctrl Pts',(-5.46544895291773,-3.99378291174356,
29.5035044191019));
#16474=CARTESIAN_POINT('Ctrl Pts',(-5.36301917750028,-4.13029333907179,
29.5115278293795));
#16475=CARTESIAN_POINT('Ctrl Pts',(-5.25573379739927,-4.26257565925522,
29.519551239657));
#16476=CARTESIAN_POINT('Ctrl Pts',(-5.14829994362497,-4.39504104671185,
29.5275857536395));
#16477=CARTESIAN_POINT('Ctrl Pts',(-5.03599731748076,-4.52326636412461,
29.5356202676219));
#16478=CARTESIAN_POINT('Ctrl Pts',(-4.91922110787673,-4.64688634375967,
29.5436547816044));
#16479=CARTESIAN_POINT('Ctrl Pts',(-4.86090367700977,-4.70862151773549,
29.5476671760408));
#16480=CARTESIAN_POINT('Ctrl Pts',(-4.80147108011093,-4.76920876799802,
29.5516795704772));
#16481=CARTESIAN_POINT('Ctrl Pts',(-4.74097547761352,-4.82860647813293,
29.5556919649136));
#16482=CARTESIAN_POINT('Ctrl Pts',(-4.61694741955579,-4.95038363774422,
29.5639181742506));
#16483=CARTESIAN_POINT('Ctrl Pts',(-4.48805099989343,-5.06754926241064,
29.5721443835875));
#16484=CARTESIAN_POINT('Ctrl Pts',(-4.35466262607329,-5.17969134341811,
29.5803705929245));
#16485=CARTESIAN_POINT('Ctrl Pts',(-4.22142410837691,-5.29170743760162,
29.5885875604677));
#16486=CARTESIAN_POINT('Ctrl Pts',(-4.08370395753063,-5.3987109976466,29.5968045280109));
#16487=CARTESIAN_POINT('Ctrl Pts',(-3.94191601363492,-5.50032609410102,
29.6050214955541));
#16488=CARTESIAN_POINT('Ctrl Pts',(-3.80025890444357,-5.60184742531182,
29.6132308808975));
#16489=CARTESIAN_POINT('Ctrl Pts',(-3.65454176721587,-5.69798998765376,
29.6214402662408));
#16490=CARTESIAN_POINT('Ctrl Pts',(-3.50521223831033,-5.78841741449245,
29.6296496515842));
#16491=CARTESIAN_POINT('Ctrl Pts',(-3.35599054108758,-5.87877954318363,
29.6378531088848));
#16492=CARTESIAN_POINT('Ctrl Pts',(-3.20316195345764,-5.96343457149376,
29.6460565661854));
#16493=CARTESIAN_POINT('Ctrl Pts',(-3.04720394539792,-6.04208880397759,
29.654260023486));
#16494=CARTESIAN_POINT('Ctrl Pts',(-2.89132727068957,-6.12070201764868,
29.6624592026179));
#16495=CARTESIAN_POINT('Ctrl Pts',(-2.73232474627738,-6.19332050883013,
29.6706583817498));
#16496=CARTESIAN_POINT('Ctrl Pts',(-2.57069942579331,-6.25969595605298,
29.6788575608816));
#16497=CARTESIAN_POINT('Ctrl Pts',(-2.40910455900307,-6.326058896711,29.6870551951114));
#16498=CARTESIAN_POINT('Ctrl Pts',(-2.24488820956445,-6.38618099467243,
29.6952528293412));
#16499=CARTESIAN_POINT('Ctrl Pts',(-2.07857472887093,-6.43986149668602,
29.703450463571));
#16500=CARTESIAN_POINT('Ctrl Pts',(-1.91227325286635,-6.49353812398227,
29.7116475060866));
#16501=CARTESIAN_POINT('Ctrl Pts',(-1.7438752881423,-6.54077397031308,29.7198445486022));
#16502=CARTESIAN_POINT('Ctrl Pts',(-1.57392166355624,-6.58141774977006,
29.7280415911178));
#16503=CARTESIAN_POINT('Ctrl Pts',(-1.40394941762237,-6.62206598245335,
29.7362395317607));
#16504=CARTESIAN_POINT('Ctrl Pts',(-1.23242152115803,-6.65612062584086,
29.7444374724035));
#16505=CARTESIAN_POINT('Ctrl Pts',(-1.05989039667072,-6.68348122964711,
29.7526354130463));
#16506=CARTESIAN_POINT('Ctrl Pts',(-0.887309011067003,-6.71084980404126,
29.7608357418823));
#16507=CARTESIAN_POINT('Ctrl Pts',(-0.713724169464792,-6.73152039836163,
29.7690360707183));
#16508=CARTESIAN_POINT('Ctrl Pts',(-0.539694892081964,-6.74544427176303,
29.7772363995543));
#16509=CARTESIAN_POINT('Ctrl Pts',(-0.365484271676276,-6.75938265420182,
29.7854452733457));
#16510=CARTESIAN_POINT('Ctrl Pts',(-0.190828648268228,-6.76656024168427,
29.7936541471371));
#16511=CARTESIAN_POINT('Ctrl Pts',(-0.0162895385699319,-6.76698039386351,
29.8018630209285));
#16512=CARTESIAN_POINT('Ctrl Pts',(0.158343244343235,-6.7674007715338,29.810076300332));
#16513=CARTESIAN_POINT('Ctrl Pts',(0.332859030791997,-6.76105649708345,
29.8182895797354));
#16514=CARTESIAN_POINT('Ctrl Pts',(0.506700040159683,-6.7480029689755,29.8265028591388));
#16515=CARTESIAN_POINT('Ctrl Pts',(0.680795319326209,-6.73493034803107,
29.8347281517543));
#16516=CARTESIAN_POINT('Ctrl Pts',(0.854213492679924,-6.71512890280006,
29.8429534443697));
#16517=CARTESIAN_POINT('Ctrl Pts',(1.02640432737228,-6.68870564135928,29.8511787369851));
#16518=CARTESIAN_POINT('Ctrl Pts',(1.18213025302498,-6.66480897546541,29.8586175260972));
#16519=CARTESIAN_POINT('Ctrl Pts',(1.33685228200919,-6.63549701095803,29.8660563152092));
#16520=CARTESIAN_POINT('Ctrl Pts',(1.49017400361122,-6.60088406495382,29.8734951043213));
#16521=CARTESIAN_POINT('Ctrl Pts',(1.6597251608569,-6.56260726379757,29.8817213053401));
#16522=CARTESIAN_POINT('Ctrl Pts',(1.82803757945248,-6.5177400964149,29.889947506359));
#16523=CARTESIAN_POINT('Ctrl Pts',(1.99456103082754,-6.46637574645212,29.8981737073778));
#16524=CARTESIAN_POINT('Ctrl Pts',(2.16089742820167,-6.41506909351091,29.9063906679936));
#16525=CARTESIAN_POINT('Ctrl Pts',(2.32544852027893,-6.35727989546785,29.9146076286094));
#16526=CARTESIAN_POINT('Ctrl Pts',(2.48767412589913,-6.29315234547297,29.9228245892251));
#16527=CARTESIAN_POINT('Ctrl Pts',(2.64975006520956,-6.2290839583564,29.9310339690267));
#16528=CARTESIAN_POINT('Ctrl Pts',(2.8095044593794,-6.15868899610454,29.9392433488283));
#16529=CARTESIAN_POINT('Ctrl Pts',(2.9664120727298,-6.08216149199961,29.9474527286298));
#16530=CARTESIAN_POINT('Ctrl Pts',(3.12320640855058,-6.00568923598894,29.9556561817702));
#16531=CARTESIAN_POINT('Ctrl Pts',(3.27715773611907,-5.92309341315075,29.9638596349106));
#16532=CARTESIAN_POINT('Ctrl Pts',(3.42776052468915,-5.83461625005302,29.972063088051));
#16533=CARTESIAN_POINT('Ctrl Pts',(3.57828479796524,-5.74618521366076,29.9802622644011));
#16534=CARTESIAN_POINT('Ctrl Pts',(3.72546370155774,-5.65187912661656,29.9884614407513));
#16535=CARTESIAN_POINT('Ctrl Pts',(3.86881598384822,-5.55198630069641,29.9966606171014));
#16536=CARTESIAN_POINT('Ctrl Pts',(4.01214129224333,-5.45211227111902,30.0048582506528));
#16537=CARTESIAN_POINT('Ctrl Pts',(4.15164111607589,-5.34665379632587,30.0130558842042));
#16538=CARTESIAN_POINT('Ctrl Pts',(4.28686264893904,-5.23594285961291,30.0212535177555));
#16539=CARTESIAN_POINT('Ctrl Pts',(4.42207444253328,-5.1252398968044,30.0294505608761));
#16540=CARTESIAN_POINT('Ctrl Pts',(4.55300828075326,-5.00928545203083,30.0376476039967));
#16541=CARTESIAN_POINT('Ctrl Pts',(4.67924401020246,-4.88845215717454,30.0458446471173));
#16542=CARTESIAN_POINT('Ctrl Pts',(4.80549359071392,-4.76760560403158,30.0540425896485));
#16543=CARTESIAN_POINT('Ctrl Pts',(4.92704377627779,-4.64187938235337,30.0622405321797));
#16544=CARTESIAN_POINT('Ctrl Pts',(5.04351086237034,-4.51168340879016,30.0704384747108));
#16545=CARTESIAN_POINT('Ctrl Pts',(5.16001189545016,-4.38144948664246,30.0786388067193));
#16546=CARTESIAN_POINT('Ctrl Pts',(5.2714266388413,-4.24674348482788,30.0868391387277));
#16547=CARTESIAN_POINT('Ctrl Pts',(5.37741127787934,-4.10800887882878,30.0950394707361));
#16548=CARTESIAN_POINT('Ctrl Pts',(5.48350638155685,-3.96912967387295,30.1032483497069));
#16549=CARTESIAN_POINT('Ctrl Pts',(5.58415985575435,-3.82621376137857,30.1114572286777));
#16550=CARTESIAN_POINT('Ctrl Pts',(5.67907032608305,-3.67973494037315,30.1196661076484));
#16551=CARTESIAN_POINT('Ctrl Pts',(5.7740317465538,-3.53317748613884,30.1278793933358));
#16552=CARTESIAN_POINT('Ctrl Pts',(5.86324383407599,-3.38305361850086,30.1360926790232));
#16553=CARTESIAN_POINT('Ctrl Pts',(5.94645097924401,-3.22986218768665,30.1443059647107));
#16554=CARTESIAN_POINT('Ctrl Pts',(6.02977984621011,-3.07644665669003,30.1525312654227));
#16555=CARTESIAN_POINT('Ctrl Pts',(6.10708605674115,-2.91995491616811,30.1607565661348));
#16556=CARTESIAN_POINT('Ctrl Pts',(6.17816147052971,-2.76090743127367,30.1689818668469));
#16557=CARTESIAN_POINT('Ctrl Pts',(6.2424406086294,-2.61706816673768,30.1764206591409));
#16558=CARTESIAN_POINT('Ctrl Pts',(6.3016241288705,-2.47113897961145,30.1838594514349));
#16559=CARTESIAN_POINT('Ctrl Pts',(6.35559336697599,-2.32351499966124,30.1912982437289));
#16560=CARTESIAN_POINT('Ctrl Pts',(6.41474103907805,-2.16172626468913,30.1994507999422));
#16561=CARTESIAN_POINT('Ctrl Pts',(6.46779942281192,-1.99742449187936,30.2076033561554));
#16562=CARTESIAN_POINT('Ctrl Pts',(6.51454649890016,-1.83111247979684,30.2157559123687));
#16563=CARTESIAN_POINT('Ctrl Pts',(6.56123941737387,-1.66499314418938,30.2238990236491));
#16564=CARTESIAN_POINT('Ctrl Pts',(6.60163548513474,-1.49686855355554,30.2320421349294));
#16565=CARTESIAN_POINT('Ctrl Pts',(6.6355607488154,-1.32726129634689,30.2401852462098));
#16566=CARTESIAN_POINT('Ctrl Pts',(6.66945384162423,-1.15781487542191,30.2483206354871));
#16567=CARTESIAN_POINT('Ctrl Pts',(6.69688827548844,-0.986888943069949,
30.2564560247644));
#16568=CARTESIAN_POINT('Ctrl Pts',(6.71773992286671,-0.815021060294054,
30.2645914140417));
#16569=CARTESIAN_POINT('Ctrl Pts',(6.73857617834234,-0.643280043931621,
30.2727207980803));
#16570=CARTESIAN_POINT('Ctrl Pts',(6.75283927894112,-0.470598823004949,
30.2808501821189));
#16571=CARTESIAN_POINT('Ctrl Pts',(6.76045619009791,-0.297524959905691,
30.2889795661576));
#16572=CARTESIAN_POINT('Ctrl Pts',(6.7680690786526,-0.124542499642788,30.2971046569497));
#16573=CARTESIAN_POINT('Ctrl Pts',(6.76904275194078,0.0488318254332298,
30.3052297477418));
#16574=CARTESIAN_POINT('Ctrl Pts',(6.76335602970208,0.222045525720619,30.3133548385339));
#16575=CARTESIAN_POINT('Ctrl Pts',(6.75764760001176,0.395920420253286,30.321510944559));
#16576=CARTESIAN_POINT('Ctrl Pts',(6.74522778903052,0.569633090865725,30.3296670505841));
#16577=CARTESIAN_POINT('Ctrl Pts',(6.72612801283416,0.742624370033458,30.3378231566093));
#16578=CARTESIAN_POINT('Ctrl Pts',(6.70710510978276,0.914919390588353,30.3459464357827));
#16579=CARTESIAN_POINT('Ctrl Pts',(6.68145597482379,1.08649845211539,30.3540697149561));
#16580=CARTESIAN_POINT('Ctrl Pts',(6.64926363232801,1.25681428532626,30.3621929941295));
#16581=CARTESIAN_POINT('Ctrl Pts',(6.6170670031498,1.42715279752948,30.3703173549862));
#16582=CARTESIAN_POINT('Ctrl Pts',(6.57832549895059,1.59622738687732,30.3784417158428));
#16583=CARTESIAN_POINT('Ctrl Pts',(6.53317324601633,1.76350115892689,30.3865660766995));
#16584=CARTESIAN_POINT('Ctrl Pts',(6.48800639022984,1.93082902958763,30.3946930650849));
#16585=CARTESIAN_POINT('Ctrl Pts',(6.43642475235122,2.09635457018854,30.4028200534703));
#16586=CARTESIAN_POINT('Ctrl Pts',(6.37861226929006,2.25955626574386,30.4109470418557));
#16587=CARTESIAN_POINT('Ctrl Pts',(6.32042603510757,2.42381304168124,30.4191265702958));
#16588=CARTESIAN_POINT('Ctrl Pts',(6.25592823851356,2.58571546736119,30.4273060987359));
#16589=CARTESIAN_POINT('Ctrl Pts',(6.18535513706265,2.74475332742539,30.4354856271759));
#16590=CARTESIAN_POINT('Ctrl Pts',(6.11511438709857,2.90304222693424,30.4436266355796));
#16591=CARTESIAN_POINT('Ctrl Pts',(6.03885564892182,3.05849318339986,30.4517676439833));
#16592=CARTESIAN_POINT('Ctrl Pts',(5.9568573097243,3.21062922050869,30.4599086523869));
#16593=CARTESIAN_POINT('Ctrl Pts',(5.87427699489374,3.36384502907839,30.4681074408452));
#16594=CARTESIAN_POINT('Ctrl Pts',(5.78587549881093,3.51369836550209,30.4763062293035));
#16595=CARTESIAN_POINT('Ctrl Pts',(5.69198041889014,3.65973331145471,30.4845050177618));
#16596=CARTESIAN_POINT('Ctrl Pts',(5.59808533896934,3.80576825740733,30.4927038062201));
#16597=CARTESIAN_POINT('Ctrl Pts',(5.49869694104231,3.94798454559957,30.5009025946784));
#16598=CARTESIAN_POINT('Ctrl Pts',(5.3941824658027,4.08596188499436,30.5091013831367));
#16599=CARTESIAN_POINT('Ctrl Pts',(5.28922318646113,4.22452644339782,30.5173350648931));
#16600=CARTESIAN_POINT('Ctrl Pts',(5.17876790491029,4.35924673323055,30.5255687466494));
#16601=CARTESIAN_POINT('Ctrl Pts',(5.06312694145214,4.48965862563531,30.5338024284058));
#16602=CARTESIAN_POINT('Ctrl Pts',(4.94761961040267,4.61991981663823,30.5420265954825));
#16603=CARTESIAN_POINT('Ctrl Pts',(4.82693876392312,4.74588225737914,30.5502507625592));
#16604=CARTESIAN_POINT('Ctrl Pts',(4.70143722576662,4.86711177313362,30.5584749296358));
#16605=CARTESIAN_POINT('Ctrl Pts',(4.57608811390686,4.98819405112183,30.566689108155));
#16606=CARTESIAN_POINT('Ctrl Pts',(4.44593023459203,5.10455461276947,30.5749032866742));
#16607=CARTESIAN_POINT('Ctrl Pts',(4.31135555119798,5.21579354567974,30.5831174651934));
#16608=CARTESIAN_POINT('Ctrl Pts',(4.17687549472523,5.3269542603287,30.5913258678682));
#16609=CARTESIAN_POINT('Ctrl Pts',(4.0379850917432,5.43300028865593,30.599534270543));
#16610=CARTESIAN_POINT('Ctrl Pts',(3.89511235262337,5.53356926047202,30.6077426732179));
#16611=CARTESIAN_POINT('Ctrl Pts',(3.75232278353098,5.63407968841055,30.6159462975628));
#16612=CARTESIAN_POINT('Ctrl Pts',(3.60555578833066,5.72911920548128,30.6241499219078));
#16613=CARTESIAN_POINT('Ctrl Pts',(3.45527154973213,5.81836639595787,30.6323535462528));
#16614=CARTESIAN_POINT('Ctrl Pts',(3.33861577388611,5.88764312347243,30.638721480586));
#16615=CARTESIAN_POINT('Ctrl Pts',(3.21984142160767,5.95343052413751,30.6450894149192));
#16616=CARTESIAN_POINT('Ctrl Pts',(3.09917575053255,6.01559628526641,30.6514573492524));
#16617=CARTESIAN_POINT('Origin',(0.,0.,-3.69717978381041));
#16618=CARTESIAN_POINT('',(3.09917575053263,6.01559628526637,33.0456763245139));
#16619=CARTESIAN_POINT('',(3.0991757505326,6.01559628526638,32.6511251802053));
#16620=CARTESIAN_POINT('',(3.09917575053259,6.01559628526639,-3.69717978381041));
#16621=CARTESIAN_POINT('',(-6.76699986099963,-0.000377079920512664,31.69717978381));
#16622=CARTESIAN_POINT('Ctrl Pts',(-6.76699816095994,-0.00498894425489755,
31.69717978381));
#16623=CARTESIAN_POINT('Ctrl Pts',(-6.76684478702294,-0.213025173280864,
31.706943004568));
#16624=CARTESIAN_POINT('Ctrl Pts',(-6.75709420253893,-0.420655042332459,
31.7167062253261));
#16625=CARTESIAN_POINT('Ctrl Pts',(-6.73788167899273,-0.62708809580008,
31.7264694460841));
#16626=CARTESIAN_POINT('Ctrl Pts',(-6.71853295542026,-0.834984579474335,
31.7363018795575));
#16627=CARTESIAN_POINT('Ctrl Pts',(-6.68958775694725,-1.04166719573885,
31.7461343130309));
#16628=CARTESIAN_POINT('Ctrl Pts',(-6.65123312178949,-1.24634945324755,
31.7559667465042));
#16629=CARTESIAN_POINT('Ctrl Pts',(-6.61257356191642,-1.45265896333844,
31.7658773491993));
#16630=CARTESIAN_POINT('Ctrl Pts',(-6.56435440770036,-1.65693616212937,
31.7757879518943));
#16631=CARTESIAN_POINT('Ctrl Pts',(-6.50681559014289,-1.858397125448,31.7856985545894));
#16632=CARTESIAN_POINT('Ctrl Pts',(-6.48084152195962,-1.94934026643764,
31.7901723808004));
#16633=CARTESIAN_POINT('Ctrl Pts',(-6.45296895452249,-2.03970981023404,
31.7946462070114));
#16634=CARTESIAN_POINT('Ctrl Pts',(-6.42322312053385,-2.12943507622078,
31.7991200332224));
#16635=CARTESIAN_POINT('Ctrl Pts',(-6.36902839969197,-2.2929079089029,31.8072710153967));
#16636=CARTESIAN_POINT('Ctrl Pts',(-6.30850382475154,-2.45456728264385,
31.8154219975709));
#16637=CARTESIAN_POINT('Ctrl Pts',(-6.24178762935317,-2.61388144146856,
31.8235729797452));
#16638=CARTESIAN_POINT('Ctrl Pts',(-6.17514893099906,-2.77301054213242,
31.8317144937982));
#16639=CARTESIAN_POINT('Ctrl Pts',(-6.10233306850275,-2.92979951671739,
31.8398560078513));
#16640=CARTESIAN_POINT('Ctrl Pts',(-6.02352823808606,-3.08373094886371,
31.8479975219043));
#16641=CARTESIAN_POINT('Ctrl Pts',(-5.94479836335716,-3.23751596820376,
31.8561312921074));
#16642=CARTESIAN_POINT('Ctrl Pts',(-5.86009102698877,-3.38844853289979,
31.8642650623104));
#16643=CARTESIAN_POINT('Ctrl Pts',(-5.76964277484345,-3.53603043690191,
31.8723988325135));
#16644=CARTESIAN_POINT('Ctrl Pts',(-5.67926152996687,-3.68350300700242,
31.8805265769315));
#16645=CARTESIAN_POINT('Ctrl Pts',(-5.58314802813492,-3.82762954854115,
31.8886543213494));
#16646=CARTESIAN_POINT('Ctrl Pts',(-5.48158506974634,-3.96793575088283,
31.8967820657674));
#16647=CARTESIAN_POINT('Ctrl Pts',(-5.38007599994814,-4.10816750774175,
31.9049054976615));
#16648=CARTESIAN_POINT('Ctrl Pts',(-5.27312344592436,-4.24458266672557,
31.9130289295555));
#16649=CARTESIAN_POINT('Ctrl Pts',(-5.161053906689,-4.3767352641267,31.9211523614496));
#16650=CARTESIAN_POINT('Ctrl Pts',(-5.04827344237681,-4.50972618562644,
31.9293273252004));
#16651=CARTESIAN_POINT('Ctrl Pts',(-4.93031104950779,-4.63839996191676,
31.9375022889512));
#16652=CARTESIAN_POINT('Ctrl Pts',(-4.80754146012847,-4.76233494298184,
31.945677252702));
#16653=CARTESIAN_POINT('Ctrl Pts',(-4.68557343699443,-4.88546074892519,
31.9537988418751));
#16654=CARTESIAN_POINT('Ctrl Pts',(-4.55886108246186,-5.00390921065724,
31.9619204310481));
#16655=CARTESIAN_POINT('Ctrl Pts',(-4.42780940443511,-5.11730328180733,
31.9700420202211));
#16656=CARTESIAN_POINT('Ctrl Pts',(-4.29674042489908,-5.23071232330044,
31.9781646816105));
#16657=CARTESIAN_POINT('Ctrl Pts',(-4.16133125758528,-5.33906540560404,
31.9862873429998));
#16658=CARTESIAN_POINT('Ctrl Pts',(-4.02202050047103,-5.44202536688233,
31.9944100043892));
#16659=CARTESIAN_POINT('Ctrl Pts',(-3.88266482259069,-5.54501852760934,
32.0025352849314));
#16660=CARTESIAN_POINT('Ctrl Pts',(-3.73940534388417,-5.64261488698913,
32.0106605654737));
#16661=CARTESIAN_POINT('Ctrl Pts',(-3.59271012898014,-5.73452028761984,
32.018785846016));
#16662=CARTESIAN_POINT('Ctrl Pts',(-3.44441670014892,-5.82742697852009,
32.0269996498037));
#16663=CARTESIAN_POINT('Ctrl Pts',(-3.29261255875426,-5.91451777661114,
32.0352134535915));
#16664=CARTESIAN_POINT('Ctrl Pts',(-3.13780644165434,-5.99553665110243,
32.0434272573792));
#16665=CARTESIAN_POINT('Ctrl Pts',(-2.98440373249586,-6.07582104213792,
32.0515665982344));
#16666=CARTESIAN_POINT('Ctrl Pts',(-2.8280536103083,-6.15014304943466,32.0597059390896));
#16667=CARTESIAN_POINT('Ctrl Pts',(-2.66927053666758,-6.218302324757,32.0678452799447));
#16668=CARTESIAN_POINT('Ctrl Pts',(-2.50830851754669,-6.28739693494528,
32.0760963151988));
#16669=CARTESIAN_POINT('Ctrl Pts',(-2.34484665549254,-6.35015830627715,
32.0843473504529));
#16670=CARTESIAN_POINT('Ctrl Pts',(-2.17943561200694,-6.40643031751037,
32.092598385707));
#16671=CARTESIAN_POINT('Ctrl Pts',(-2.01402456852133,-6.46270232874358,
32.100849420961));
#16672=CARTESIAN_POINT('Ctrl Pts',(-1.84666473067044,-6.51248493471082,
32.1091004562151));
#16673=CARTESIAN_POINT('Ctrl Pts',(-1.67791584378681,-6.5556759698119,32.1173514914692));
#16674=CARTESIAN_POINT('Ctrl Pts',(-1.50956092534225,-6.59876616925714,
32.1255832635));
#16675=CARTESIAN_POINT('Ctrl Pts',(-1.33929790619343,-6.63543023282369,
32.1338150355308));
#16676=CARTESIAN_POINT('Ctrl Pts',(-1.16765820561721,-6.66549797951022,
32.1420468075617));
#16677=CARTESIAN_POINT('Ctrl Pts',(-0.996223459996037,-6.69552982230243,
32.1502687500341));
#16678=CARTESIAN_POINT('Ctrl Pts',(-0.823415655782832,-6.71898097124773,
32.1584906925064));
#16679=CARTESIAN_POINT('Ctrl Pts',(-0.649780791222935,-6.73573113502593,
32.1667126349788));
#16680=CARTESIAN_POINT('Ctrl Pts',(-0.476318474771694,-6.75246465347725,
32.1749264069687));
#16681=CARTESIAN_POINT('Ctrl Pts',(-0.302031088948244,-6.76251041405279,
32.1831401789586));
#16682=CARTESIAN_POINT('Ctrl Pts',(-0.127474328789869,-6.76579923553009,
32.1913539509485));
#16683=CARTESIAN_POINT('Ctrl Pts',(0.0469439284113645,-6.76908544747512,
32.1995612056789));
#16684=CARTESIAN_POINT('Ctrl Pts',(0.221630777597417,-6.76562539220543,
32.2077684604092));
#16685=CARTESIAN_POINT('Ctrl Pts',(0.396025806211847,-6.75540173200782,
32.2159757151396));
#16686=CARTESIAN_POINT('Ctrl Pts',(0.570317379979352,-6.74518413670329,
32.2241781011516));
#16687=CARTESIAN_POINT('Ctrl Pts',(0.744317121298345,-6.72821095039046,
32.2323804871635));
#16688=CARTESIAN_POINT('Ctrl Pts',(0.917464927668259,-6.70451691820512,
32.2405828731755));
#16689=CARTESIAN_POINT('Ctrl Pts',(1.09056105361766,-6.68082995811369,32.2487828109742));
#16690=CARTESIAN_POINT('Ctrl Pts',(1.26280539605337,-6.65042619271413,32.2569827487729));
#16691=CARTESIAN_POINT('Ctrl Pts',(1.43364303215575,-6.61339222006009,32.2651826865716));
#16692=CARTESIAN_POINT('Ctrl Pts',(1.60445678074731,-6.57636342571127,32.2733814778073));
#16693=CARTESIAN_POINT('Ctrl Pts',(1.77386386440957,-6.53270634561018,32.2815802690431));
#16694=CARTESIAN_POINT('Ctrl Pts',(1.94131959180215,-6.4825586956452,32.2897790602788));
#16695=CARTESIAN_POINT('Ctrl Pts',(2.10878228190038,-6.43240896057192,32.2979781924153));
#16696=CARTESIAN_POINT('Ctrl Pts',(2.27429311068322,-6.37576822073721,32.3061773245517));
#16697=CARTESIAN_POINT('Ctrl Pts',(2.43732253438915,-6.31282407986781,32.3143764566881));
#16698=CARTESIAN_POINT('Ctrl Pts',(2.60038831103241,-6.24986590346816,32.322577417099));
#16699=CARTESIAN_POINT('Ctrl Pts',(2.76097124625396,-6.18060165564131,32.3307783775099));
#16700=CARTESIAN_POINT('Ctrl Pts',(2.91856171277046,-6.10526711362823,32.3389793379208));
#16701=CARTESIAN_POINT('Ctrl Pts',(3.07629987949085,-6.029861965014,32.3471879846059));
#16702=CARTESIAN_POINT('Ctrl Pts',(3.2310396501565,-5.9483753100772,32.3553966312909));
#16703=CARTESIAN_POINT('Ctrl Pts',(3.38229511921994,-5.86108938052483,32.3636052779759));
#16704=CARTESIAN_POINT('Ctrl Pts',(3.53362280189238,-5.77376177821824,32.3718178436994));
#16705=CARTESIAN_POINT('Ctrl Pts',(3.68146256310972,-5.68062957185078,32.380030409423));
#16706=CARTESIAN_POINT('Ctrl Pts',(3.82535752992038,-5.58201834180804,32.3882429751465));
#16707=CARTESIAN_POINT('Ctrl Pts',(3.96944994138975,-5.48327180292795,32.3964668096952));
#16708=CARTESIAN_POINT('Ctrl Pts',(4.10958645295233,-5.37903142924726,32.404690644244));
#16709=CARTESIAN_POINT('Ctrl Pts',(4.24534236141756,-5.2696638635072,32.4129144787927));
#16710=CARTESIAN_POINT('Ctrl Pts',(4.37007650441145,-5.16917564359735,32.4204706357671));
#16711=CARTESIAN_POINT('Ctrl Pts',(4.49111271303223,-5.06435956603924,32.4280267927415));
#16712=CARTESIAN_POINT('Ctrl Pts',(4.60814964621003,-4.95552679723704,32.4355829497159));
#16713=CARTESIAN_POINT('Ctrl Pts',(4.74206273581399,-4.83100087260165,32.4442286677683));
#16714=CARTESIAN_POINT('Ctrl Pts',(4.8710450556412,-4.70093232175336,32.4528743858207));
#16715=CARTESIAN_POINT('Ctrl Pts',(4.9946388149526,-4.56572799323053,32.4615201038731));
#16716=CARTESIAN_POINT('Ctrl Pts',(5.11807390506471,-4.4306972395117,32.4701547225855));
#16717=CARTESIAN_POINT('Ctrl Pts',(5.2361340243519,-4.29054407950895,32.4787893412978));
#16718=CARTESIAN_POINT('Ctrl Pts',(5.34839713467694,-4.14571309786139,32.4874239600102));
#16719=CARTESIAN_POINT('Ctrl Pts',(5.46462494195089,-3.99576724856602,32.4963635199126));
#16720=CARTESIAN_POINT('Ctrl Pts',(5.57463855681819,-3.84080733988134,32.505303079815));
#16721=CARTESIAN_POINT('Ctrl Pts',(5.67801202730815,-3.68136773736936,32.5142426397175));
#16722=CARTESIAN_POINT('Ctrl Pts',(5.77758215396685,-3.5277942785188,32.522853292988));
#16723=CARTESIAN_POINT('Ctrl Pts',(5.87099180450186,-3.37006514882201,32.5314639462585));
#16724=CARTESIAN_POINT('Ctrl Pts',(5.95790150533329,-3.20869111208096,32.540074599529));
#16725=CARTESIAN_POINT('Ctrl Pts',(6.04472894031823,-3.04746982666234,32.5486771022401));
#16726=CARTESIAN_POINT('Ctrl Pts',(6.12506854816439,-2.88261078050792,32.5572796049512));
#16727=CARTESIAN_POINT('Ctrl Pts',(6.19862503150459,-2.71465222796674,32.5658821076623));
#16728=CARTESIAN_POINT('Ctrl Pts',(6.27209872850359,-2.54688270939516,32.5744749284298));
#16729=CARTESIAN_POINT('Ctrl Pts',(6.33880440904753,-2.37602092253564,32.5830677491973));
#16730=CARTESIAN_POINT('Ctrl Pts',(6.39849336995919,-2.20262833782468,32.5916605699648));
#16731=CARTESIAN_POINT('Ctrl Pts',(6.40552798512501,-2.18219323412346,32.592673272923));
#16732=CARTESIAN_POINT('Ctrl Pts',(6.41246519380273,-2.16172300429233,32.5936859758812));
#16733=CARTESIAN_POINT('Ctrl Pts',(6.41930463211463,-2.14121858765322,32.5946986788394));
#16734=CARTESIAN_POINT('Ctrl Pts',(6.47735396903799,-1.96718853787127,32.6032939365995));
#16735=CARTESIAN_POINT('Ctrl Pts',(6.52828795764044,-1.79089905606792,32.6118891943595));
#16736=CARTESIAN_POINT('Ctrl Pts',(6.57196228735581,-1.61294782729417,32.6204844521196));
#16737=CARTESIAN_POINT('Ctrl Pts',(6.61567751622878,-1.43482995474136,32.629087758974));
#16738=CARTESIAN_POINT('Ctrl Pts',(6.65211944363989,-1.25504752561917,32.6376910658284));
#16739=CARTESIAN_POINT('Ctrl Pts',(6.68119499365782,-1.07420782752765,32.6462943726829));
#16740=CARTESIAN_POINT('Ctrl Pts',(6.71147602606209,-0.885870452843098,
32.6552543756229));
#16741=CARTESIAN_POINT('Ctrl Pts',(6.7337667928603,-0.696386650018505,32.6642143785629));
#16742=CARTESIAN_POINT('Ctrl Pts',(6.7480220248994,-0.506446198003862,32.6731743815029));
#16743=CARTESIAN_POINT('Ctrl Pts',(6.76174720473161,-0.323568300670539,
32.6818012247076));
#16744=CARTESIAN_POINT('Ctrl Pts',(6.7680236811107,-0.140267398301859,32.6904280679123));
#16745=CARTESIAN_POINT('Ctrl Pts',(6.76686438025181,0.042842260436053,32.6990549111171));
#16746=CARTESIAN_POINT('Ctrl Pts',(6.76570397139435,0.226126925720858,32.7076899994032));
#16747=CARTESIAN_POINT('Ctrl Pts',(6.7570936109133,0.409219677908722,32.7163250876894));
#16748=CARTESIAN_POINT('Ctrl Pts',(6.74109815138213,0.591510535351992,32.7249601759755));
#16749=CARTESIAN_POINT('Ctrl Pts',(6.72507893538356,0.774072131301086,32.7336080891007));
#16750=CARTESIAN_POINT('Ctrl Pts',(6.7016527364256,0.955829149535095,32.7422560022258));
#16751=CARTESIAN_POINT('Ctrl Pts',(6.67093585820488,1.13617946457256,32.7509039153509));
#16752=CARTESIAN_POINT('Ctrl Pts',(6.66748989207677,1.15641202441624,32.7518740795549));
#16753=CARTESIAN_POINT('Ctrl Pts',(6.66395222187037,1.17662689398922,32.7528442437589));
#16754=CARTESIAN_POINT('Ctrl Pts',(6.66032305121468,1.19682323400673,32.7538144079629));
#16755=CARTESIAN_POINT('Ctrl Pts',(6.62955477662437,1.3680487271933,32.762039504399));
#16756=CARTESIAN_POINT('Ctrl Pts',(6.59213884052978,1.53831261615814,32.7702646008351));
#16757=CARTESIAN_POINT('Ctrl Pts',(6.54814725973299,1.70706076776762,32.7784896972711));
#16758=CARTESIAN_POINT('Ctrl Pts',(6.504202434922,1.87562956719112,32.7867060517506));
#16759=CARTESIAN_POINT('Ctrl Pts',(6.45369597298111,2.04268549338548,32.79492240623));
#16760=CARTESIAN_POINT('Ctrl Pts',(6.39675125827712,2.20768257223046,32.8031387607094));
#16761=CARTESIAN_POINT('Ctrl Pts',(6.33985566006461,2.37253733624149,32.8113480283414));
#16762=CARTESIAN_POINT('Ctrl Pts',(6.27653298579924,2.53533645288026,32.8195572959734));
#16763=CARTESIAN_POINT('Ctrl Pts',(6.20695699571139,2.69554704158349,32.8277665636055));
#16764=CARTESIAN_POINT('Ctrl Pts',(6.1374270842959,2.85565152628134,32.8359703944172));
#16765=CARTESIAN_POINT('Ctrl Pts',(6.06165224929661,3.01317057045485,32.8441742252289));
#16766=CARTESIAN_POINT('Ctrl Pts',(5.97985515367365,3.16758920017775,32.8523780560406));
#16767=CARTESIAN_POINT('Ctrl Pts',(5.89809132361558,3.32194503032434,32.8605785504862));
#16768=CARTESIAN_POINT('Ctrl Pts',(5.81031027763882,3.47320264082487,32.8687790449317));
#16769=CARTESIAN_POINT('Ctrl Pts',(5.71678168752888,3.62086952777016,32.8769795393772));
#16770=CARTESIAN_POINT('Ctrl Pts',(5.623272236074,3.76850619779878,32.8851783557643));
#16771=CARTESIAN_POINT('Ctrl Pts',(5.52401777391962,3.9125533046984,32.8933771721514));
#16772=CARTESIAN_POINT('Ctrl Pts',(5.41933261281328,4.05254525350408,32.9015759885386));
#16773=CARTESIAN_POINT('Ctrl Pts',(5.31464988302334,4.19253395099201,32.9097746145079));
#16774=CARTESIAN_POINT('Ctrl Pts',(5.20453692011565,4.32846739096257,32.9179732404773));
#16775=CARTESIAN_POINT('Ctrl Pts',(5.08934985901588,4.45991109917395,32.9261718664466));
#16776=CARTESIAN_POINT('Ctrl Pts',(4.97414457798132,4.59137559874654,32.9343717892494));
#16777=CARTESIAN_POINT('Ctrl Pts',(4.85386383666108,4.71834868284553,32.9425717120522));
#16778=CARTESIAN_POINT('Ctrl Pts',(4.72890237018331,4.84043090780921,32.9507716348549));
#16779=CARTESIAN_POINT('Ctrl Pts',(4.60383805510605,4.9626136116342,32.9589783065428));
#16780=CARTESIAN_POINT('Ctrl Pts',(4.47408557458634,5.0798971630359,32.9671849782306));
#16781=CARTESIAN_POINT('Ctrl Pts',(4.34007529857162,5.19192020380981,32.9753916499185));
#16782=CARTESIAN_POINT('Ctrl Pts',(4.20600842139092,5.3039905591249,32.983601787812));
#16783=CARTESIAN_POINT('Ctrl Pts',(4.06768044618244,5.41079575412562,32.9918119257056));
#16784=CARTESIAN_POINT('Ctrl Pts',(3.92555273277976,5.51201639530992,33.0000220635992));
#16785=CARTESIAN_POINT('Ctrl Pts',(3.78324764619229,5.61336335828653,33.0082424476177));
#16786=CARTESIAN_POINT('Ctrl Pts',(3.63713364440716,5.70911164252225,33.0164628316361));
#16787=CARTESIAN_POINT('Ctrl Pts',(3.4876997688326,5.79898605986297,33.0246832156546));
#16788=CARTESIAN_POINT('Ctrl Pts',(3.3604923451832,5.87549276249613,33.0316809186077));
#16789=CARTESIAN_POINT('Ctrl Pts',(3.2308797291331,5.94774369719842,33.0386786215608));
#16790=CARTESIAN_POINT('Ctrl Pts',(3.09917575053263,6.01559628526637,33.0456763245139));
#16791=CARTESIAN_POINT('Ctrl Pts',(3.09917575053259,6.01559628526639,31.0457515827422));
#16792=CARTESIAN_POINT('Ctrl Pts',(2.93382384459264,6.1007839529376,31.0545010306546));
#16793=CARTESIAN_POINT('Ctrl Pts',(2.76495772122983,6.1791501026705,31.063250478567));
#16794=CARTESIAN_POINT('Ctrl Pts',(2.5931509331671,6.25042856433178,31.0719999264794));
#16795=CARTESIAN_POINT('Ctrl Pts',(2.42134553245611,6.32170645041454,31.0807493037394));
#16796=CARTESIAN_POINT('Ctrl Pts',(2.24659977927579,6.38589665313461,31.0894986809994));
#16797=CARTESIAN_POINT('Ctrl Pts',(2.06950718689903,6.4427811543908,31.0982480582594));
#16798=CARTESIAN_POINT('Ctrl Pts',(1.89241596572849,6.49966521519727,31.1069973677741));
#16799=CARTESIAN_POINT('Ctrl Pts',(1.7129782145719,6.54924360009548,31.1157466772887));
#16800=CARTESIAN_POINT('Ctrl Pts',(1.53180337335841,6.59134792173557,31.1244959868034));
#16801=CARTESIAN_POINT('Ctrl Pts',(1.35062987477784,6.63345193135304,31.1332452314795));
#16802=CARTESIAN_POINT('Ctrl Pts',(1.16771959102958,6.66808192368237,31.1419944761556));
#16803=CARTESIAN_POINT('Ctrl Pts',(0.98369374690696,6.69512028363167,31.1507437208317));
#16804=CARTESIAN_POINT('Ctrl Pts',(0.799669205419936,6.72215845218866,31.1594929035759));
#16805=CARTESIAN_POINT('Ctrl Pts',(0.61452940287349,6.74160505424579,31.1682420863201));
#16806=CARTESIAN_POINT('Ctrl Pts',(0.42890312736321,6.75339404354122,31.1769912690643));
#16807=CARTESIAN_POINT('Ctrl Pts',(0.243278104163749,6.76518295330331,31.1857403927829));
#16808=CARTESIAN_POINT('Ctrl Pts',(0.0571669005388933,6.76931433552276,
31.1944895165015));
#16809=CARTESIAN_POINT('Ctrl Pts',(-0.12879840477783,6.76577415902472,31.2032386402201));
#16810=CARTESIAN_POINT('Ctrl Pts',(-0.314762517259429,6.7622340052344,31.2119877078193));
#16811=CARTESIAN_POINT('Ctrl Pts',(-0.500580446819854,6.75102239665086,
31.2207367754185));
#16812=CARTESIAN_POINT('Ctrl Pts',(-0.685621118842968,6.73217741012494,
31.2294858430177));
#16813=CARTESIAN_POINT('Ctrl Pts',(-0.870660665414657,6.71333253821769,
31.2382348574035));
#16814=CARTESIAN_POINT('Ctrl Pts',(-1.05492267885485,6.68685441030612,31.2469838717893));
#16815=CARTESIAN_POINT('Ctrl Pts',(-1.23778137635232,6.65283295028181,31.2557328861751));
#16816=CARTESIAN_POINT('Ctrl Pts',(-1.42999922978829,6.61707018861869,31.2649296965424));
#16817=CARTESIAN_POINT('Ctrl Pts',(-1.6206660123368,6.57297172934417,31.2741265069098));
#16818=CARTESIAN_POINT('Ctrl Pts',(-1.80906628500372,6.52070304311298,31.2833233172772));
#16819=CARTESIAN_POINT('Ctrl Pts',(-1.98831342545513,6.47097374915035,31.292073315015));
#16820=CARTESIAN_POINT('Ctrl Pts',(-2.16550875896686,6.41384933989534,31.3008233127528));
#16821=CARTESIAN_POINT('Ctrl Pts',(-2.34005036713995,6.34952386240482,31.3095733104905));
#16822=CARTESIAN_POINT('Ctrl Pts',(-2.51458843547073,6.28519968948602,31.3183231307714));
#16823=CARTESIAN_POINT('Ctrl Pts',(-2.6864726171804,6.21367483971106,31.3270729510523));
#16824=CARTESIAN_POINT('Ctrl Pts',(-2.85511905908717,6.13519226743851,31.3358227713331));
#16825=CARTESIAN_POINT('Ctrl Pts',(-3.02376230488868,6.05671118252945,31.3445724257917));
#16826=CARTESIAN_POINT('Ctrl Pts',(-3.18916767379886,5.97127275992643,31.3533220802502));
#16827=CARTESIAN_POINT('Ctrl Pts',(-3.35077334102767,5.87916720438008,31.3620717347087));
#16828=CARTESIAN_POINT('Ctrl Pts',(-3.51237616037355,5.78706327195651,31.3708212349772));
#16829=CARTESIAN_POINT('Ctrl Pts',(-3.67017916302293,5.68829258362303,31.3795707352456));
#16830=CARTESIAN_POINT('Ctrl Pts',(-3.82364636566462,5.58319061741042,31.3883202355141));
#16831=CARTESIAN_POINT('Ctrl Pts',(-3.97711106778789,5.47809036367708,31.3970695932225));
#16832=CARTESIAN_POINT('Ctrl Pts',(-4.1262398748191,5.36665920043238,31.4058189509309));
#16833=CARTESIAN_POINT('Ctrl Pts',(-4.27052628213905,5.24927559512355,31.4145683086394));
#16834=CARTESIAN_POINT('Ctrl Pts',(-4.41481053024949,5.13189374643061,31.4233175354159));
#16835=CARTESIAN_POINT('Ctrl Pts',(-4.55425230136496,5.00855981477383,31.4320667621924));
#16836=CARTESIAN_POINT('Ctrl Pts',(-4.6883780063051,4.87969268192113,31.4408159889689));
#16837=CARTESIAN_POINT('Ctrl Pts',(-4.82250188228876,4.75082730631829,31.4495650964398));
#16838=CARTESIAN_POINT('Ctrl Pts',(-4.95130963052966,4.61642907903527,31.4583142039106));
#16839=CARTESIAN_POINT('Ctrl Pts',(-5.07436379033383,4.47695444731671,31.4670633113815));
#16840=CARTESIAN_POINT('Ctrl Pts',(-5.19741643562795,4.33748153220597,31.4758123111712));
#16841=CARTESIAN_POINT('Ctrl Pts',(-5.31471544462739,4.19293255254631,31.4845613109609));
#16842=CARTESIAN_POINT('Ctrl Pts',(-5.42586245275572,4.04379841779678,31.4933103107506));
#16843=CARTESIAN_POINT('Ctrl Pts',(-5.53702160019097,3.89464799484422,31.5020602660928));
#16844=CARTESIAN_POINT('Ctrl Pts',(-5.64202723081196,3.74091164443933,31.5108102214349));
#16845=CARTESIAN_POINT('Ctrl Pts',(-5.74052265232913,3.5831115916332,31.5195601767771));
#16846=CARTESIAN_POINT('Ctrl Pts',(-5.83901427066876,3.42531763191855,31.5283097942596));
#16847=CARTESIAN_POINT('Ctrl Pts',(-5.93099603115709,3.26346052695669,31.537059411742));
#16848=CARTESIAN_POINT('Ctrl Pts',(-6.01615550622733,3.09809004467116,31.5458090292245));
#16849=CARTESIAN_POINT('Ctrl Pts',(-6.10131214578781,2.93272506863866,31.5545583553756));
#16850=CARTESIAN_POINT('Ctrl Pts',(-6.17964682328731,2.76384720416932,31.5633076815267));
#16851=CARTESIAN_POINT('Ctrl Pts',(-6.25089348288549,2.59203002791629,31.5720570076778));
#16852=CARTESIAN_POINT('Ctrl Pts',(-6.32213814889314,2.4202176593707,31.5808060890093));
#16853=CARTESIAN_POINT('Ctrl Pts',(-6.38629508412568,2.24546640831965,31.5895551703409));
#16854=CARTESIAN_POINT('Ctrl Pts',(-6.44314639819795,2.06836976660094,31.5983042516725));
#16855=CARTESIAN_POINT('Ctrl Pts',(-6.50000285283686,1.89125711158325,31.6070541241069));
#16856=CARTESIAN_POINT('Ctrl Pts',(-6.54955227673237,1.71179891440301,31.6158039965413));
#16857=CARTESIAN_POINT('Ctrl Pts',(-6.59162635926375,1.53060476278473,31.6245538689757));
#16858=CARTESIAN_POINT('Ctrl Pts',(-6.63369752055184,1.34942319164754,31.6333031338981));
#16859=CARTESIAN_POINT('Ctrl Pts',(-6.66829431424241,1.16650618642779,31.6420523988206));
#16860=CARTESIAN_POINT('Ctrl Pts',(-6.69529923745404,0.982474997619467,
31.6508016637431));
#16861=CARTESIAN_POINT('Ctrl Pts',(-6.72230554731433,0.798434359178603,
31.6595513779228));
#16862=CARTESIAN_POINT('Ctrl Pts',(-6.74171916496696,0.613279706241152,
31.6683010921025));
#16863=CARTESIAN_POINT('Ctrl Pts',(-6.7534741481727,0.427639953656142,31.6770508062822));
#16864=CARTESIAN_POINT('Ctrl Pts',(-6.76248837758744,0.28528336419895,31.6837604654582));
#16865=CARTESIAN_POINT('Ctrl Pts',(-6.76699999999998,0.142641701105103,
31.6904701246341));
#16866=CARTESIAN_POINT('Ctrl Pts',(-6.767,1.1656404461135E-12,31.69717978381));
#16867=CARTESIAN_POINT('',(-6.76699987500998,-0.00130062097133924,31.3028202162256));
#16868=CARTESIAN_POINT('Ctrl Pts',(3.09917575053255,6.01559628526641,30.6514573492524));
#16869=CARTESIAN_POINT('Ctrl Pts',(2.9437882613957,6.09565038388479,30.6596576710026));
#16870=CARTESIAN_POINT('Ctrl Pts',(2.78526378870031,6.16969705802948,30.6678579927529));
#16871=CARTESIAN_POINT('Ctrl Pts',(2.62410961849097,6.23749450582068,30.6760583145031));
#16872=CARTESIAN_POINT('Ctrl Pts',(2.46295499662551,6.30529214362329,30.6842586592359));
#16873=CARTESIAN_POINT('Ctrl Pts',(2.29917099269971,6.36684038095351,30.6924590039686));
#16874=CARTESIAN_POINT('Ctrl Pts',(2.13328512866462,6.42194546534136,30.7006593487014));
#16875=CARTESIAN_POINT('Ctrl Pts',(1.96736873792929,6.47706069029423,30.7088612024805));
#16876=CARTESIAN_POINT('Ctrl Pts',(1.79935005669109,6.52573028780835,30.7170630562597));
#16877=CARTESIAN_POINT('Ctrl Pts',(1.62977208218026,6.56781028655258,30.7252649100388));
#16878=CARTESIAN_POINT('Ctrl Pts',(1.4546507002461,6.61126585649397,30.7337348777476));
#16879=CARTESIAN_POINT('Ctrl Pts',(1.27786675017466,6.64769359432657,30.7422048454564));
#16880=CARTESIAN_POINT('Ctrl Pts',(1.10002932849864,6.67699217286068,30.7506748131651));
#16881=CARTESIAN_POINT('Ctrl Pts',(0.927584372820258,6.70540234676637,30.7588879507172));
#16882=CARTESIAN_POINT('Ctrl Pts',(0.754149264606598,6.72710940622123,30.7671010882693));
#16883=CARTESIAN_POINT('Ctrl Pts',(0.580283964397827,6.74207382936903,30.7753142258214));
#16884=CARTESIAN_POINT('Ctrl Pts',(0.398263342545787,6.75774017339368,30.7839126086085));
#16885=CARTESIAN_POINT('Ctrl Pts',(0.215771653946936,6.76601607239216,30.7925109913956));
#16886=CARTESIAN_POINT('Ctrl Pts',(0.0334502721502293,6.76691732469764,
30.8011093741828));
#16887=CARTESIAN_POINT('Ctrl Pts',(-0.148871109646478,6.76781857700313,
30.8097077569699));
#16888=CARTESIAN_POINT('Ctrl Pts',(-0.331021742430141,6.76134525818256,
30.818306139757));
#16889=CARTESIAN_POINT('Ctrl Pts',(-0.512368023175418,6.74757497244953,
30.8269045225441));
#16890=CARTESIAN_POINT('Ctrl Pts',(-0.694717879583281,6.7337284815494,30.835550489035));
#16891=CARTESIAN_POINT('Ctrl Pts',(-0.876668532959975,6.71247347993989,
30.8441964555258));
#16892=CARTESIAN_POINT('Ctrl Pts',(-1.05760834483217,6.68384272622728,30.8528424220167));
#16893=CARTESIAN_POINT('Ctrl Pts',(-1.23831671008625,6.65524859514102,30.861477329141));
#16894=CARTESIAN_POINT('Ctrl Pts',(-1.41801651240011,6.61929757251252,30.8701122362654));
#16895=CARTESIAN_POINT('Ctrl Pts',(-1.59610054872383,6.57607421174393,30.8787471433897));
#16896=CARTESIAN_POINT('Ctrl Pts',(-1.78009683132037,6.53141587028375,30.8876687224612));
#16897=CARTESIAN_POINT('Ctrl Pts',(-1.96236789808547,6.47899401621822,30.8965903015328));
#16898=CARTESIAN_POINT('Ctrl Pts',(-2.14225159143541,6.41895997175496,30.9055118806043));
#16899=CARTESIAN_POINT('Ctrl Pts',(-2.31587434137413,6.36101544273433,30.91412293958));
#16900=CARTESIAN_POINT('Ctrl Pts',(-2.48727276428476,6.29597975581458,30.9227339985557));
#16901=CARTESIAN_POINT('Ctrl Pts',(-2.65586293018433,6.22404057635173,30.9313450575313));
#16902=CARTESIAN_POINT('Ctrl Pts',(-2.82429410777394,6.15216923885641,30.9399479958808));
#16903=CARTESIAN_POINT('Ctrl Pts',(-2.98992202883562,6.073407507968,30.9485509342303));
#16904=CARTESIAN_POINT('Ctrl Pts',(-3.15218016280069,5.98799208593714,30.9571538725798));
#16905=CARTESIAN_POINT('Ctrl Pts',(-3.31425660519236,5.90267230941904,30.9657471776285));
#16906=CARTESIAN_POINT('Ctrl Pts',(-3.47297051900245,5.81071384723926,30.9743404826773));
#16907=CARTESIAN_POINT('Ctrl Pts',(-3.62777732434809,5.71240060613276,30.982933787726));
#16908=CARTESIAN_POINT('Ctrl Pts',(-3.64502533639689,5.70144690184711,30.9838912225667));
#16909=CARTESIAN_POINT('Ctrl Pts',(-3.66222487020964,5.69041435984547,30.9848486574074));
#16910=CARTESIAN_POINT('Ctrl Pts',(-3.67937519039829,5.6793034087185,30.9858060922482));
#16911=CARTESIAN_POINT('Ctrl Pts',(-3.83334910897148,5.57955036240354,30.9944018497958));
#16912=CARTESIAN_POINT('Ctrl Pts',(-3.9831736433357,5.47359055720332,31.0029976073434));
#16913=CARTESIAN_POINT('Ctrl Pts',(-4.12836292280519,5.36180087075298,31.0115933648909));
#16914=CARTESIAN_POINT('Ctrl Pts',(-4.27368766880941,5.24990688072391,31.0201971425726));
#16915=CARTESIAN_POINT('Ctrl Pts',(-4.41436828545345,5.13217233830758,31.0288009202543));
#16916=CARTESIAN_POINT('Ctrl Pts',(-4.54995293253852,5.00901360665791,31.037404697936));
#16917=CARTESIAN_POINT('Ctrl Pts',(-4.69086617481371,4.88101462916037,31.046346611604));
#16918=CARTESIAN_POINT('Ctrl Pts',(-4.82627452527868,4.74715675270992,31.0552885252719));
#16919=CARTESIAN_POINT('Ctrl Pts',(-4.95571483057532,4.60794743004039,31.0642304389399));
#16920=CARTESIAN_POINT('Ctrl Pts',(-5.08059947440093,4.47363759015746,31.0728576412706));
#16921=CARTESIAN_POINT('Ctrl Pts',(-5.19992884907543,4.33434683021309,31.0814848436014));
#16922=CARTESIAN_POINT('Ctrl Pts',(-5.31332949183721,4.19056305419367,31.0901120459321));
#16923=CARTESIAN_POINT('Ctrl Pts',(-5.42683813135508,4.04664234613391,31.0987474643527));
#16924=CARTESIAN_POINT('Ctrl Pts',(-5.53440658728367,3.89822032588502,31.1073828827732));
#16925=CARTESIAN_POINT('Ctrl Pts',(-5.63570461907915,3.74581398984119,31.1160183011937));
#16926=CARTESIAN_POINT('Ctrl Pts',(-5.73715230428661,3.59318249514627,31.1246664772149));
#16927=CARTESIAN_POINT('Ctrl Pts',(-5.83231089144553,3.43655518024921,31.133314653236));
#16928=CARTESIAN_POINT('Ctrl Pts',(-5.9208952358588,3.27647502752342,31.1419628292572));
#16929=CARTESIAN_POINT('Ctrl Pts',(-5.93026712361037,3.25953915434473,31.1428777734887));
#16930=CARTESIAN_POINT('Ctrl Pts',(-5.93956547085843,3.2425646536331,31.1437927177202));
#16931=CARTESIAN_POINT('Ctrl Pts',(-5.94878997126802,3.22555218183509,31.1447076619518));
#16932=CARTESIAN_POINT('Ctrl Pts',(-6.03489620025897,3.0667490242332,31.1532482217672));
#16933=CARTESIAN_POINT('Ctrl Pts',(-6.11473540022817,2.90431951038833,31.1617887815826));
#16934=CARTESIAN_POINT('Ctrl Pts',(-6.18800286363856,2.73877884459498,31.170329341398));
#16935=CARTESIAN_POINT('Ctrl Pts',(-6.26116971371862,2.57346550477845,31.1788581730311));
#16936=CARTESIAN_POINT('Ctrl Pts',(-6.3277826876891,2.40504981867954,31.1873870046642));
#16937=CARTESIAN_POINT('Ctrl Pts',(-6.38758252318929,2.23407218089451,31.1959158362974));
#16938=CARTESIAN_POINT('Ctrl Pts',(-6.45004579098903,2.05547934886741,31.2048245346218));
#16939=CARTESIAN_POINT('Ctrl Pts',(-6.50507492820516,1.87409140196102,31.2137332329461));
#16940=CARTESIAN_POINT('Ctrl Pts',(-6.5524289823788,1.69055122101708,31.2226419312705));
#16941=CARTESIAN_POINT('Ctrl Pts',(-6.59763534842354,1.51533529181184,31.2311465859292));
#16942=CARTESIAN_POINT('Ctrl Pts',(-6.63584728569493,1.33815838867071,31.2396512405878));
#16943=CARTESIAN_POINT('Ctrl Pts',(-6.66690478959617,1.1595988644612,31.2481558952465));
#16944=CARTESIAN_POINT('Ctrl Pts',(-6.69793377371252,0.981203309617538,
31.2566527401687));
#16945=CARTESIAN_POINT('Ctrl Pts',(-6.72182136437854,0.801427977178822,
31.2651495850908));
#16946=CARTESIAN_POINT('Ctrl Pts',(-6.73845808253665,0.620863648393569,
31.273646430013));
#16947=CARTESIAN_POINT('Ctrl Pts',(-6.75507757981683,0.440486224034566,
31.2821344797432));
#16948=CARTESIAN_POINT('Ctrl Pts',(-6.76446114528484,0.259321749013042,
31.2906225294735));
#16949=CARTESIAN_POINT('Ctrl Pts',(-6.76655081321516,0.0779685332507414,
31.2991105792037));
#16950=CARTESIAN_POINT('Ctrl Pts',(-6.76685523765853,0.0515488562485993,
31.3003471248658));
#16951=CARTESIAN_POINT('Ctrl Pts',(-6.76700495406095,0.0251251850256775,
31.3015836705278));
#16952=CARTESIAN_POINT('Ctrl Pts',(-6.76699987501013,-0.00130062020750468,
31.3028202161899));
#16953=CARTESIAN_POINT('Ctrl Pts',(-6.76699987500998,-0.00130062097129432,
31.3028202162256));
#16954=CARTESIAN_POINT('Ctrl Pts',(-6.76696418572452,-0.186988377484985,
31.3115091241998));
#16955=CARTESIAN_POINT('Ctrl Pts',(-6.75928127931588,-0.372492585525971,
31.320198032174));
#16956=CARTESIAN_POINT('Ctrl Pts',(-6.74402186049804,-0.557187710852092,
31.3288869401482));
#16957=CARTESIAN_POINT('Ctrl Pts',(-6.72873714990478,-0.742188959739467,
31.3375902495824));
#16958=CARTESIAN_POINT('Ctrl Pts',(-6.70585086745089,-0.926378161231628,
31.3462935590165));
#16959=CARTESIAN_POINT('Ctrl Pts',(-6.67548509089492,-1.10913831474692,
31.3549968684507));
#16960=CARTESIAN_POINT('Ctrl Pts',(-6.64422548702367,-1.297278077674,31.3639563628598));
#16961=CARTESIAN_POINT('Ctrl Pts',(-6.60503944955329,-1.48390304693927,
31.3729158572688));
#16962=CARTESIAN_POINT('Ctrl Pts',(-6.55811497097053,-1.66835758383274,
31.3818753516779));
#16963=CARTESIAN_POINT('Ctrl Pts',(-6.51233849186315,-1.84829947150813,
31.3906156535633));
#16964=CARTESIAN_POINT('Ctrl Pts',(-6.45919792650325,-2.02617564230019,
31.3993559554488));
#16965=CARTESIAN_POINT('Ctrl Pts',(-6.3989168635405,-2.20139773178247,31.4080962573342));
#16966=CARTESIAN_POINT('Ctrl Pts',(-6.33636817438614,-2.38321124782446,
31.4171653480051));
#16967=CARTESIAN_POINT('Ctrl Pts',(-6.26613152823398,-2.56216680451879,
31.426234438676));
#16968=CARTESIAN_POINT('Ctrl Pts',(-6.18850929400993,-2.73763432875041,
31.4353035293469));
#16969=CARTESIAN_POINT('Ctrl Pts',(-6.11088705978587,-2.91310185298206,
31.4443726200178));
#16970=CARTESIAN_POINT('Ctrl Pts',(-6.02587944881343,-3.08508107139603,
31.4534417106886));
#16971=CARTESIAN_POINT('Ctrl Pts',(-5.93383941563804,-3.25297383780141,
31.4625108013595));
#16972=CARTESIAN_POINT('Ctrl Pts',(-5.85107161789943,-3.40395286347316,
31.4706662597663));
#16973=CARTESIAN_POINT('Ctrl Pts',(-5.76240285295694,-3.5520172041671,31.4788217181731));
#16974=CARTESIAN_POINT('Ctrl Pts',(-5.66806278834808,-3.69666785461499,
31.4869771765799));
#16975=CARTESIAN_POINT('Ctrl Pts',(-5.57383754799868,-3.84114244620722,
31.4951227087218));
#16976=CARTESIAN_POINT('Ctrl Pts',(-5.47395494562947,-3.98221131530862,
31.5032682408637));
#16977=CARTESIAN_POINT('Ctrl Pts',(-5.36869131702243,-4.11939832287775,
31.5114137730056));
#16978=CARTESIAN_POINT('Ctrl Pts',(-5.26353367325877,-4.25644720350119,
31.5195511038061));
#16979=CARTESIAN_POINT('Ctrl Pts',(-5.15300601015973,-4.38962171583212,
31.5276884346067));
#16980=CARTESIAN_POINT('Ctrl Pts',(-5.03742889329539,-4.51847309884576,
31.5358257654072));
#16981=CARTESIAN_POINT('Ctrl Pts',(-4.9219438565367,-4.64722182616697,31.5439566132092));
#16982=CARTESIAN_POINT('Ctrl Pts',(-4.80141761900865,-4.77165401124391,
31.5520874610112));
#16983=CARTESIAN_POINT('Ctrl Pts',(-4.67621209563142,-4.89135251609107,
31.5602183088133));
#16984=CARTESIAN_POINT('Ctrl Pts',(-4.55108002170852,-5.01098080207225,
31.568344386807));
#16985=CARTESIAN_POINT('Ctrl Pts',(-4.4212743921104,-5.12588068607262,31.5764704648008));
#16986=CARTESIAN_POINT('Ctrl Pts',(-4.28719517807036,-5.23567058791233,
31.5845965427946));
#16987=CARTESIAN_POINT('Ctrl Pts',(-4.15264054362595,-5.34584978469161,
31.5927514343768));
#16988=CARTESIAN_POINT('Ctrl Pts',(-4.01378221527217,-5.45088242198391,
31.600906325959));
#16989=CARTESIAN_POINT('Ctrl Pts',(-3.87105974598709,-5.55042209593094,
31.6090612175412));
#16990=CARTESIAN_POINT('Ctrl Pts',(-3.72889384443081,-5.64957359995257,
31.6171843078975));
#16991=CARTESIAN_POINT('Ctrl Pts',(-3.58289419735056,-5.74327470834417,
31.6253073982538));
#16992=CARTESIAN_POINT('Ctrl Pts',(-3.43352588972085,-5.83122533989355,
31.6334304886101));
#16993=CARTESIAN_POINT('Ctrl Pts',(-3.28414585300972,-5.91918287772804,
31.6415542168285));
#16994=CARTESIAN_POINT('Ctrl Pts',(-3.13139694407138,-6.00138885361899,
31.649677945047));
#16995=CARTESIAN_POINT('Ctrl Pts',(-2.97577035579683,-6.07758832017774,
31.6578016732654));
#16996=CARTESIAN_POINT('Ctrl Pts',(-2.82010193923835,-6.15380826712455,
31.6659275849257));
#16997=CARTESIAN_POINT('Ctrl Pts',(-2.6615546316913,-6.22401832938343,31.674053496586));
#16998=CARTESIAN_POINT('Ctrl Pts',(-2.50064113288644,-6.28801104678709,
31.6821794082463));
#16999=CARTESIAN_POINT('Ctrl Pts',(-2.33869857552963,-6.35241300427063,
31.6903572859564));
#17000=CARTESIAN_POINT('Ctrl Pts',(-2.17435980680415,-6.41051768095202,
31.6985351636665));
#17001=CARTESIAN_POINT('Ctrl Pts',(-2.00816373523178,-6.46216429785718,
31.7067130413765));
#17002=CARTESIAN_POINT('Ctrl Pts',(-1.84276088146323,-6.51356441666134,
31.71485188785));
#17003=CARTESIAN_POINT('Ctrl Pts',(-1.6755187842758,-6.55856795078435,31.7229907343234));
#17004=CARTESIAN_POINT('Ctrl Pts',(-1.50697937842296,-6.5970676935293,31.7311295807969));
#17005=CARTESIAN_POINT('Ctrl Pts',(-1.33722758305271,-6.63584438447096,
31.7393269741253));
#17006=CARTESIAN_POINT('Ctrl Pts',(-1.1661601154976,-6.66802329127322,31.7475243674537));
#17007=CARTESIAN_POINT('Ctrl Pts',(-0.994336027983862,-6.69354800262561,
31.7557217607821));
#17008=CARTESIAN_POINT('Ctrl Pts',(-0.822511940470152,-6.71907271397799,
31.7639191541104));
#17009=CARTESIAN_POINT('Ctrl Pts',(-0.649931609667629,-6.73794325016948,
31.7721165474388));
#17010=CARTESIAN_POINT('Ctrl Pts',(-0.477153788763507,-6.75015653610112,
31.7803139407672));
#17011=CARTESIAN_POINT('Ctrl Pts',(-0.303768608059589,-6.76241275496743,
31.7885401501042));
#17012=CARTESIAN_POINT('Ctrl Pts',(-0.129668529657173,-6.76800143151726,
31.7967663594412));
#17013=CARTESIAN_POINT('Ctrl Pts',(0.0445927278613814,-6.76685307130441,
31.8049925687782));
#17014=CARTESIAN_POINT('Ctrl Pts',(0.218658210322328,-6.76570600122506,
31.8132095363214));
#17015=CARTESIAN_POINT('Ctrl Pts',(0.392884155952847,-6.75783696820683,
31.8214265038646));
#17016=CARTESIAN_POINT('Ctrl Pts',(0.566711752314562,-6.74322821724051,
31.8296434714077));
#17017=CARTESIAN_POINT('Ctrl Pts',(0.740378949409586,-6.72863294648671,
31.8378528567511));
#17018=CARTESIAN_POINT('Ctrl Pts',(0.913648174147453,-6.70731037313801,
31.8460622420945));
#17019=CARTESIAN_POINT('Ctrl Pts',(1.08596054741427,-6.67929477485907,31.8542716274379));
#17020=CARTESIAN_POINT('Ctrl Pts',(1.25814849295863,-6.65129940679936,31.8624750847385));
#17021=CARTESIAN_POINT('Ctrl Pts',(1.42938061072744,-6.61662069777632,31.8706785420391));
#17022=CARTESIAN_POINT('Ctrl Pts',(1.59910298711738,-6.57534475420052,31.8788819993397));
#17023=CARTESIAN_POINT('Ctrl Pts',(1.76873685192792,-6.53409033636007,31.8870811784716));
#17024=CARTESIAN_POINT('Ctrl Pts',(1.93686219623547,-6.48624562262405,31.8952803576035));
#17025=CARTESIAN_POINT('Ctrl Pts',(2.10293505979891,-6.43194784915647,31.9034795367353));
#17026=CARTESIAN_POINT('Ctrl Pts',(2.26897663165553,-6.37766030655968,31.9116771709651));
#17027=CARTESIAN_POINT('Ctrl Pts',(2.4329661506371,-6.31692223159436,31.9198748051949));
#17028=CARTESIAN_POINT('Ctrl Pts',(2.59437429525009,-6.24992088079086,31.9280724394248));
#17029=CARTESIAN_POINT('Ctrl Pts',(2.75577078924634,-6.18292436621828,31.9362694819404));
#17030=CARTESIAN_POINT('Ctrl Pts',(2.91458594834338,-6.10966561286604,31.9444665244559));
#17031=CARTESIAN_POINT('Ctrl Pts',(3.0703099905606,-6.03038021702312,31.9526635669715));
#17032=CARTESIAN_POINT('Ctrl Pts',(3.22605109502979,-5.95108613409898,31.9608615076144));
#17033=CARTESIAN_POINT('Ctrl Pts',(3.37870008815778,-5.86576425590392,31.9690594482572));
#17034=CARTESIAN_POINT('Ctrl Pts',(3.5277713323129,-5.77469639261765,31.9772573889));
#17035=CARTESIAN_POINT('Ctrl Pts',(3.67688600334077,-5.68360199978483,31.985457717736));
#17036=CARTESIAN_POINT('Ctrl Pts',(3.82242054334053,-5.58675847459734,31.993658046572));
#17037=CARTESIAN_POINT('Ctrl Pts',(3.96391782853191,-5.48449126616561,32.001858375408));
#17038=CARTESIAN_POINT('Ctrl Pts',(4.105562557566,-5.38211749264909,32.0100672491994));
#17039=CARTESIAN_POINT('Ctrl Pts',(4.24316133590766,-5.27430895519029,32.0182761229908));
#17040=CARTESIAN_POINT('Ctrl Pts',(4.37628892899677,-5.16143237967334,32.0264849967823));
#17041=CARTESIAN_POINT('Ctrl Pts',(4.50948797019639,-5.04849522454359,32.0346982761857));
#17042=CARTESIAN_POINT('Ctrl Pts',(4.63821077825436,-4.93048485117022,32.0429115555891));
#17043=CARTESIAN_POINT('Ctrl Pts',(4.76206871192509,-4.80780517314337,32.0511248349925));
#17044=CARTESIAN_POINT('Ctrl Pts',(4.8861078072909,-4.68494605680551,32.059350127608));
#17045=CARTESIAN_POINT('Ctrl Pts',(5.00526756326862,-4.55740424939333,32.0675754202234));
#17046=CARTESIAN_POINT('Ctrl Pts',(5.1191985549309,-4.4256180534693,32.0758007128389));
#17047=CARTESIAN_POINT('Ctrl Pts',(5.22223545099334,-4.30643326999845,32.0832395019509));
#17048=CARTESIAN_POINT('Ctrl Pts',(5.32099614197417,-4.18377755902988,32.0906782910629));
#17049=CARTESIAN_POINT('Ctrl Pts',(5.4152530290108,-4.05799502609224,32.098117080175));
#17050=CARTESIAN_POINT('Ctrl Pts',(5.51948721128105,-3.91889814015816,32.1063432811938));
#17051=CARTESIAN_POINT('Ctrl Pts',(5.61850434854473,-3.77558819810754,32.1145694822127));
#17052=CARTESIAN_POINT('Ctrl Pts',(5.71194605337206,-3.62849297689377,32.1227956832315));
#17053=CARTESIAN_POINT('Ctrl Pts',(5.80528279613786,-3.48156298615912,32.1310126438473));
#17054=CARTESIAN_POINT('Ctrl Pts',(5.89305638689484,-3.33085648304833,32.139229604463));
#17055=CARTESIAN_POINT('Ctrl Pts',(5.97494916800274,-3.17683355556809,32.1474465650788));
#17056=CARTESIAN_POINT('Ctrl Pts',(6.05676639636252,-3.02295272675988,32.1556559448804));
#17057=CARTESIAN_POINT('Ctrl Pts',(6.1327134529015,-2.86576188170144,32.163865324682));
#17058=CARTESIAN_POINT('Ctrl Pts',(6.20251637967704,-2.70574935273724,32.1720747044836));
#17059=CARTESIAN_POINT('Ctrl Pts',(6.27226891308459,-2.54585234285841,32.180278157624));
#17060=CARTESIAN_POINT('Ctrl Pts',(6.33588600902273,-2.38313803397643,32.1884816107644));
#17061=CARTESIAN_POINT('Ctrl Pts',(6.39313996397682,-2.21811866251615,32.1966850639048));
#17062=CARTESIAN_POINT('Ctrl Pts',(6.45036407014013,-2.05318532229507,32.2048842402549));
#17063=CARTESIAN_POINT('Ctrl Pts',(6.50123152681869,-1.88594965155674,32.213083416605));
#17064=CARTESIAN_POINT('Ctrl Pts',(6.5455629995142,-1.71694321961754,32.2212825929552));
#17065=CARTESIAN_POINT('Ctrl Pts',(6.58988613057413,-1.54796858878896,32.2294802265066));
#17066=CARTESIAN_POINT('Ctrl Pts',(6.6276756304514,-1.37722420541406,32.2376778600579));
#17067=CARTESIAN_POINT('Ctrl Pts',(6.65880213940589,-1.20525643256677,32.2458754936093));
#17068=CARTESIAN_POINT('Ctrl Pts',(6.68992640648781,-1.03330104561965,32.2540725367299));
#17069=CARTESIAN_POINT('Ctrl Pts',(6.71438857363848,-0.860122797470459,
32.2622695798505));
#17070=CARTESIAN_POINT('Ctrl Pts',(6.73211049824738,-0.686277815019089,
32.270466622971));
#17071=CARTESIAN_POINT('Ctrl Pts',(6.74983436737299,-0.512413757637681,
32.2786645655022));
#17072=CARTESIAN_POINT('Ctrl Pts',(6.76081648414606,-0.337883177110012,
32.2868625080334));
#17073=CARTESIAN_POINT('Ctrl Pts',(6.76503063082165,-0.163246941915793,
32.2950604505646));
#17074=CARTESIAN_POINT('Ctrl Pts',(6.76924600580636,0.0114401949902511,
32.3032607825731));
#17075=CARTESIAN_POINT('Ctrl Pts',(6.7666894727042,0.186232689418164,32.3114611145815));
#17076=CARTESIAN_POINT('Ctrl Pts',(6.75738694139935,0.360569999036963,32.3196614465899));
#17077=CARTESIAN_POINT('Ctrl Pts',(6.74807471434261,0.53508901525204,32.3278703255607));
#17078=CARTESIAN_POINT('Ctrl Pts',(6.73200246103901,0.709151540184308,32.3360792045314));
#17079=CARTESIAN_POINT('Ctrl Pts',(6.70924806209167,0.88220147433519,32.3442880835022));
#17080=CARTESIAN_POINT('Ctrl Pts',(6.68648144805519,1.05534430570459,32.3525013691896));
#17081=CARTESIAN_POINT('Ctrl Pts',(6.6570255977479,1.22747310944518,32.360714654877));
#17082=CARTESIAN_POINT('Ctrl Pts',(6.6210094738311,1.39804239829802,32.3689279405644));
#17083=CARTESIAN_POINT('Ctrl Pts',(6.5849406627639,1.56886120899821,32.3771532412764));
#17084=CARTESIAN_POINT('Ctrl Pts',(6.5422924869989,1.73811559783988,32.3853785419886));
#17085=CARTESIAN_POINT('Ctrl Pts',(6.49324405981116,1.90527441061046,32.3936038427006));
#17086=CARTESIAN_POINT('Ctrl Pts',(6.44888567402466,2.05644939275844,32.4010426349946));
#17087=CARTESIAN_POINT('Ctrl Pts',(6.39929321471691,2.20591044020288,32.4084814272886));
#17088=CARTESIAN_POINT('Ctrl Pts',(6.3446326166538,2.35327983029913,32.4159202195826));
#17089=CARTESIAN_POINT('Ctrl Pts',(6.28471566292562,2.51482078009176,32.4240743523486));
#17090=CARTESIAN_POINT('Ctrl Pts',(6.21853144286844,2.67432463303835,32.4322284851145));
#17091=CARTESIAN_POINT('Ctrl Pts',(6.14623714389316,2.83126437674549,32.4403826178805));
#17092=CARTESIAN_POINT('Ctrl Pts',(6.07402941856448,2.98801618245334,32.4485269859344));
#17093=CARTESIAN_POINT('Ctrl Pts',(5.99572633284242,3.14220966305313,32.4566713539884));
#17094=CARTESIAN_POINT('Ctrl Pts',(5.91153450832306,3.29333398805916,32.4648157220424));
#17095=CARTESIAN_POINT('Ctrl Pts',(5.82744327266781,3.44427775605412,32.4729503595466));
#17096=CARTESIAN_POINT('Ctrl Pts',(5.73747749404295,3.59215935775243,32.4810849970509));
#17097=CARTESIAN_POINT('Ctrl Pts',(5.64189126552677,3.73648925436334,32.4892196345552));
#17098=CARTESIAN_POINT('Ctrl Pts',(5.5463704465614,3.88072038618511,32.497348705536));
#17099=CARTESIAN_POINT('Ctrl Pts',(5.44523703419817,4.02140434728218,32.5054777765168));
#17100=CARTESIAN_POINT('Ctrl Pts',(5.33879053080062,4.15807703971843,32.5136068474976));
#17101=CARTESIAN_POINT('Ctrl Pts',(5.23239661581678,4.2946822109129,32.521731902424));
#17102=CARTESIAN_POINT('Ctrl Pts',(5.12069505983306,4.42727977118434,32.5298569573504));
#17103=CARTESIAN_POINT('Ctrl Pts',(5.00402805947163,4.55543545448957,32.5379820122768));
#17104=CARTESIAN_POINT('Ctrl Pts',(4.88739650143855,4.68355220531352,32.5461045988885));
#17105=CARTESIAN_POINT('Ctrl Pts',(4.76580274928459,4.80722949669052,32.5542271855003));
#17106=CARTESIAN_POINT('Ctrl Pts',(4.63962854518207,4.92606698723553,32.5623497721121));
#17107=CARTESIAN_POINT('Ctrl Pts',(4.51344096484698,5.04491707621873,32.5704732198318));
#17108=CARTESIAN_POINT('Ctrl Pts',(4.38267222337509,5.15892608295491,32.5785966675515));
#17109=CARTESIAN_POINT('Ctrl Pts',(4.24774033827205,5.26773110728105,32.5867201152712));
#17110=CARTESIAN_POINT('Ctrl Pts',(4.11280270583172,5.37654076608757,32.5948439090039));
#17111=CARTESIAN_POINT('Ctrl Pts',(3.97370186490346,5.48014577588667,32.6029677027367));
#17112=CARTESIAN_POINT('Ctrl Pts',(3.83088789796103,5.57822435128382,32.6110914964694));
#17113=CARTESIAN_POINT('Ctrl Pts',(3.68799082433446,5.67636000082686,32.6192200176219));
#17114=CARTESIAN_POINT('Ctrl Pts',(3.54137661311616,5.76896258923199,32.6273485387743));
#17115=CARTESIAN_POINT('Ctrl Pts',(3.39152367184721,5.85575410884884,32.6354770599267));
#17116=CARTESIAN_POINT('Ctrl Pts',(3.29536362809119,5.91144788605024,32.6406931000196));
#17117=CARTESIAN_POINT('Ctrl Pts',(3.19787050428405,5.96474972359129,32.6459091401124));
#17118=CARTESIAN_POINT('Ctrl Pts',(3.0991757505326,6.01559628526638,32.6511251802053));
#17119=CARTESIAN_POINT('Origin',(0.,0.,-3.69717978381041));
#17120=CARTESIAN_POINT('',(3.09917575053259,6.01559628526639,35.0459310802154));
#17121=CARTESIAN_POINT('',(3.09917575053259,6.01559628526639,34.6514942595564));
#17122=CARTESIAN_POINT('',(3.09917575053259,6.01559628526639,-3.69717978381041));
#17123=CARTESIAN_POINT('',(-6.76699984329972,-0.00145629033198537,33.6971797837663));
#17124=CARTESIAN_POINT('Ctrl Pts',(-6.76699984329952,-0.00145629125626415,
33.69717978381));
#17125=CARTESIAN_POINT('Ctrl Pts',(-6.76698266837336,-0.081263625227222,
33.7009561167744));
#17126=CARTESIAN_POINT('Ctrl Pts',(-6.76555371680281,-0.161054131447447,
33.7047324497388));
#17127=CARTESIAN_POINT('Ctrl Pts',(-6.76271448371177,-0.240794127409707,
33.7085087827031));
#17128=CARTESIAN_POINT('Ctrl Pts',(-6.75653063770426,-0.414467735690516,
33.7167336310252));
#17129=CARTESIAN_POINT('Ctrl Pts',(-6.74364363212401,-0.588146728668887,
33.7249584793472));
#17130=CARTESIAN_POINT('Ctrl Pts',(-6.72404282540133,-0.761273329474309,
33.7331833276693));
#17131=CARTESIAN_POINT('Ctrl Pts',(-6.70446409353292,-0.934204951341491,
33.7413989129885));
#17132=CARTESIAN_POINT('Ctrl Pts',(-6.67818665685065,-1.10658506658277,
33.7496144983077));
#17133=CARTESIAN_POINT('Ctrl Pts',(-6.64525186112367,-1.27785629169811,
33.7578300836269));
#17134=CARTESIAN_POINT('Ctrl Pts',(-6.61234754002283,-1.44896903923858,
33.7660380670502));
#17135=CARTESIAN_POINT('Ctrl Pts',(-6.57279819509873,-1.61897458997166,
33.7742460504734));
#17136=CARTESIAN_POINT('Ctrl Pts',(-6.52669692064897,-1.78732098571891,
33.7824540338966));
#17137=CARTESIAN_POINT('Ctrl Pts',(-6.48062904411642,-1.95554542347145,
33.7906560710732));
#17138=CARTESIAN_POINT('Ctrl Pts',(-6.42801878661428,-2.12211275570558,
33.7988581082497));
#17139=CARTESIAN_POINT('Ctrl Pts',(-6.36901025685276,-2.28648143401699,
33.8070601454263));
#17140=CARTESIAN_POINT('Ctrl Pts',(-6.31003262619114,-2.45076404266638,
33.8152578877057));
#17141=CARTESIAN_POINT('Ctrl Pts',(-6.24466351869628,-2.61284995409234,
33.8234556299851));
#17142=CARTESIAN_POINT('Ctrl Pts',(-6.17309683537031,-2.77221291771412,
33.8316533722645));
#17143=CARTESIAN_POINT('Ctrl Pts',(-6.10154375926479,-2.93154558110572,
33.8398495558788));
#17144=CARTESIAN_POINT('Ctrl Pts',(-6.0237955956277,-3.08815599842659,33.8480457394932));
#17145=CARTESIAN_POINT('Ctrl Pts',(-5.94009443924441,-3.24153776051701,
33.8562419231075));
#17146=CARTESIAN_POINT('Ctrl Pts',(-5.85639944443407,-3.39490823156968,
33.8644375033684));
#17147=CARTESIAN_POINT('Ctrl Pts',(-5.76675250070972,-3.5450502053198,33.8726330836293));
#17148=CARTESIAN_POINT('Ctrl Pts',(-5.67144170697693,-3.69148181146307,
33.8808286638902));
#17149=CARTESIAN_POINT('Ctrl Pts',(-5.57612058877703,-3.83792927969542,
33.8890251319309));
#17150=CARTESIAN_POINT('Ctrl Pts',(-5.47513459401187,-3.9806652787704,33.8972215999717));
#17151=CARTESIAN_POINT('Ctrl Pts',(-5.36881522412025,-4.11923683335332,
33.9054180680124));
#17152=CARTESIAN_POINT('Ctrl Pts',(-5.26246499363265,-4.25784861015317,
33.9136169151858));
#17153=CARTESIAN_POINT('Ctrl Pts',(-5.15077852280994,-4.39229325009773,
33.9218157623592));
#17154=CARTESIAN_POINT('Ctrl Pts',(-5.03412769199013,-4.52215074723722,
33.9300146095326));
#17155=CARTESIAN_POINT('Ctrl Pts',(-4.91735494970878,-4.65214395808878,
33.9382220252985));
#17156=CARTESIAN_POINT('Ctrl Pts',(-4.79560772212199,-4.77754018102969,
33.9464294410645));
#17157=CARTESIAN_POINT('Ctrl Pts',(-4.66929556599789,-4.8979554833984,33.9546368568305));
#17158=CARTESIAN_POINT('Ctrl Pts',(-4.54291571100061,-5.01843532413408,
33.9628486714826));
#17159=CARTESIAN_POINT('Ctrl Pts',(-4.41196631888719,-5.13392868526123,
33.9710604861348));
#17160=CARTESIAN_POINT('Ctrl Pts',(-4.27689005332436,-5.24409195874511,
33.9792723007869));
#17161=CARTESIAN_POINT('Ctrl Pts',(-4.14161486742574,-5.35441746439659,
33.9874962085845));
#17162=CARTESIAN_POINT('Ctrl Pts',(-4.00220094912176,-5.45939697981976,
33.9957201163822));
#17163=CARTESIAN_POINT('Ctrl Pts',(-3.85912102143023,-5.55872952588587,
34.0039440241798));
#17164=CARTESIAN_POINT('Ctrl Pts',(-3.72691781068673,-5.65051096394738,
34.0115427631032));
#17165=CARTESIAN_POINT('Ctrl Pts',(-3.59158526791413,-5.7374717215886,34.0191415020265));
#17166=CARTESIAN_POINT('Ctrl Pts',(-3.45351406910012,-5.81940972732867,
34.0267402409499));
#17167=CARTESIAN_POINT('Ctrl Pts',(-3.3054084568843,-5.90730263046935,34.0348912231242));
#17168=CARTESIAN_POINT('Ctrl Pts',(-3.15371264648572,-5.98967591738706,
34.0430422052985));
#17169=CARTESIAN_POINT('Ctrl Pts',(-2.99887967364111,-6.06621873188086,
34.0511931874728));
#17170=CARTESIAN_POINT('Ctrl Pts',(-2.84422655364465,-6.14267263480149,
34.0593347015258));
#17171=CARTESIAN_POINT('Ctrl Pts',(-2.68644384953959,-6.21330938633918,
34.0674762155788));
#17172=CARTESIAN_POINT('Ctrl Pts',(-2.52601291824701,-6.27786171692633,
34.0756177296319));
#17173=CARTESIAN_POINT('Ctrl Pts',(-2.36573458179814,-6.3423526481766,34.0837514998349));
#17174=CARTESIAN_POINT('Ctrl Pts',(-2.20281336980553,-6.40077054443534,
34.091885270038));
#17175=CARTESIAN_POINT('Ctrl Pts',(-2.03775454890624,-6.45289434272807,
34.1000190402411));
#17176=CARTESIAN_POINT('Ctrl Pts',(-1.87281800942803,-6.50497952586474,
34.108146784659));
#17177=CARTESIAN_POINT('Ctrl Pts',(-1.70574736152882,-6.5507797859163,34.116274529077));
#17178=CARTESIAN_POINT('Ctrl Pts',(-1.53706712773142,-6.59012243018652,
34.124402273495));
#17179=CARTESIAN_POINT('Ctrl Pts',(-1.36847639447767,-6.62944419952687,
34.1325257053891));
#17180=CARTESIAN_POINT('Ctrl Pts',(-1.19827813151021,-6.66231509388206,
34.1406491372831));
#17181=CARTESIAN_POINT('Ctrl Pts',(-1.02701126863786,-6.6886124759991,34.1487725691772));
#17182=CARTESIAN_POINT('Ctrl Pts',(-0.854657956151481,-6.7150766783648,
34.156947532928));
#17183=CARTESIAN_POINT('Ctrl Pts',(-0.681222798994661,-6.73488357358447,
34.1651224966788));
#17184=CARTESIAN_POINT('Ctrl Pts',(-0.507265202436242,-6.74796050776806,
34.1732974604296));
#17185=CARTESIAN_POINT('Ctrl Pts',(-0.334443380121393,-6.7609520622653,
34.1814190496027));
#17186=CARTESIAN_POINT('Ctrl Pts',(-0.161106291187816,-6.76730127307965,
34.1895406387757));
#17187=CARTESIAN_POINT('Ctrl Pts',(0.0121930457427909,-6.7669890150373,
34.1976622279487));
#17188=CARTESIAN_POINT('Ctrl Pts',(0.185515261740115,-6.76667671577049,
34.2057848893381));
#17189=CARTESIAN_POINT('Ctrl Pts',(0.358799349785193,-6.75970119659649,
34.2139075507275));
#17190=CARTESIAN_POINT('Ctrl Pts',(0.531493081306014,-6.74609547105019,
34.2220302121168));
#17191=CARTESIAN_POINT('Ctrl Pts',(0.704242497935716,-6.73248535833649,
34.2301554926591));
#17192=CARTESIAN_POINT('Ctrl Pts',(0.876400814308157,-6.71224081074426,
34.2382807732013));
#17193=CARTESIAN_POINT('Ctrl Pts',(1.04742175089768,-6.68544663248062,34.2464060537436));
#17194=CARTESIAN_POINT('Ctrl Pts',(1.22030592510498,-6.65836053720451,34.2546198575314));
#17195=CARTESIAN_POINT('Ctrl Pts',(1.39202741182048,-6.62458132085763,34.2628336613191));
#17196=CARTESIAN_POINT('Ctrl Pts',(1.56203422165276,-6.58424924272963,34.2710474651069));
#17197=CARTESIAN_POINT('Ctrl Pts',(1.73049982037851,-6.54428279846548,34.2791868059621));
#17198=CARTESIAN_POINT('Ctrl Pts',(1.89728136921399,-6.49788197471459,34.2873261468172));
#17199=CARTESIAN_POINT('Ctrl Pts',(2.06185906664541,-6.44523282661628,34.2954654876724));
#17200=CARTESIAN_POINT('Ctrl Pts',(2.22869522791532,-6.39186118574427,34.3037165229265));
#17201=CARTESIAN_POINT('Ctrl Pts',(2.39326624427484,-6.33206862222528,34.3119675581806));
#17202=CARTESIAN_POINT('Ctrl Pts',(2.55505398101794,-6.26609831985458,34.3202185934347));
#17203=CARTESIAN_POINT('Ctrl Pts',(2.71684171776106,-6.20012801748387,34.3284696286888));
#17204=CARTESIAN_POINT('Ctrl Pts',(2.87584585302401,-6.1279801959522,34.3367206639428));
#17205=CARTESIAN_POINT('Ctrl Pts',(3.03157677142156,-6.04994473354734,34.3449716991969));
#17206=CARTESIAN_POINT('Ctrl Pts',(3.18694411369143,-5.97209145610316,34.3532034712278));
#17207=CARTESIAN_POINT('Ctrl Pts',(3.33953861418369,-5.88813511228987,34.3614352432586));
#17208=CARTESIAN_POINT('Ctrl Pts',(3.48884744795318,-5.79829565345806,34.3696670152895));
#17209=CARTESIAN_POINT('Ctrl Pts',(3.63797799205412,-5.7085634719181,34.3778889577619));
#17210=CARTESIAN_POINT('Ctrl Pts',(3.78383037786145,-5.61296234672479,34.3861109002343));
#17211=CARTESIAN_POINT('Ctrl Pts',(3.92591348474255,-5.51175945686281,34.3943328427067));
#17212=CARTESIAN_POINT('Ctrl Pts',(4.06785539779484,-5.41065713647611,34.4025466146966));
#17213=CARTESIAN_POINT('Ctrl Pts',(4.20603520160814,-5.30396434393153,34.4107603866865));
#17214=CARTESIAN_POINT('Ctrl Pts',(4.33998796628217,-5.19199320613249,34.4189741586764));
#17215=CARTESIAN_POINT('Ctrl Pts',(4.47383444544757,-5.08011091240742,34.4271814134068));
#17216=CARTESIAN_POINT('Ctrl Pts',(4.6034602921703,-4.962958844041,34.4353886681372));
#17217=CARTESIAN_POINT('Ctrl Pts',(4.72843100769114,-4.84089136477003,34.4435959228675));
#17218=CARTESIAN_POINT('Ctrl Pts',(4.85332758792063,-4.7188962985288,34.4517983088795));
#17219=CARTESIAN_POINT('Ctrl Pts',(4.97357428259048,-4.59199187995433,34.4600006948915));
#17220=CARTESIAN_POINT('Ctrl Pts',(5.08877097700547,-4.46057159381921,34.4682030809035));
#17221=CARTESIAN_POINT('Ctrl Pts',(5.20393328800127,-4.32919053345189,34.4764030187022));
#17222=CARTESIAN_POINT('Ctrl Pts',(5.31404836241997,-4.19329655699442,34.4846029565009));
#17223=CARTESIAN_POINT('Ctrl Pts',(5.41875399560152,-4.0533189037075,34.4928028942996));
#17224=CARTESIAN_POINT('Ctrl Pts',(5.5234449882331,-3.91336082290932,34.5010016855354));
#17225=CARTESIAN_POINT('Ctrl Pts',(5.62272783078984,-3.76932048893365,34.5092004767711));
#17226=CARTESIAN_POINT('Ctrl Pts',(5.71628156094439,-3.62165902812609,34.5173992680069));
#17227=CARTESIAN_POINT('Ctrl Pts',(5.80983918100523,-3.47399142764621,34.5255984001433));
#17228=CARTESIAN_POINT('Ctrl Pts',(5.89766702218114,-3.32270270312299,34.5337975322797));
#17229=CARTESIAN_POINT('Ctrl Pts',(5.97948826981045,-3.16828171588311,34.5419966644162));
#17230=CARTESIAN_POINT('Ctrl Pts',(6.061327762261,-3.01382629524862,34.5501976248271));
#17231=CARTESIAN_POINT('Ctrl Pts',(6.13715782573818,-2.85623753744992,34.558398585238));
#17232=CARTESIAN_POINT('Ctrl Pts',(6.20674826987113,-2.69602761752393,34.566599545649));
#17233=CARTESIAN_POINT('Ctrl Pts',(6.27640393700271,-2.53566754233571,34.574808192334));
#17234=CARTESIAN_POINT('Ctrl Pts',(6.33980815780448,-2.37268172594962,34.5830168390191));
#17235=CARTESIAN_POINT('Ctrl Pts',(6.39677911214155,-2.2076018641208,34.5912254857041));
#17236=CARTESIAN_POINT('Ctrl Pts',(6.45377726601229,-2.04244318852952,34.5994380514276));
#17237=CARTESIAN_POINT('Ctrl Pts',(6.50433592586619,-1.8751888170663,34.6076506171512));
#17238=CARTESIAN_POINT('Ctrl Pts',(6.54832361526619,-1.70638413897548,34.6158631828747));
#17239=CARTESIAN_POINT('Ctrl Pts',(6.59237166212351,-1.53734783650767,34.6240870174234));
#17240=CARTESIAN_POINT('Ctrl Pts',(6.62983064205607,-1.36675732621911,34.6323108519722));
#17241=CARTESIAN_POINT('Ctrl Pts',(6.66062029188332,-1.19516790759801,34.640534686521));
#17242=CARTESIAN_POINT('Ctrl Pts',(6.68891018826879,-1.03750950937422,34.6480908434952));
#17243=CARTESIAN_POINT('Ctrl Pts',(6.71157030468227,-0.87900811179361,34.6556470004694));
#17244=CARTESIAN_POINT('Ctrl Pts',(6.72857714554799,-0.720096241074283,
34.6632031574437));
#17245=CARTESIAN_POINT('Ctrl Pts',(6.74803629013535,-0.538270051637305,
34.671848875496));
#17246=CARTESIAN_POINT('Ctrl Pts',(6.76013831584193,-0.355492023085606,
34.6804945935484));
#17247=CARTESIAN_POINT('Ctrl Pts',(6.76480433960703,-0.172369506682167,
34.6891403116007));
#17248=CARTESIAN_POINT('Ctrl Pts',(6.76946437314853,0.0105179177294988,
34.697774930313));
#17249=CARTESIAN_POINT('Ctrl Pts',(6.76670743285558,0.193748644696248,34.7064095490253));
#17250=CARTESIAN_POINT('Ctrl Pts',(6.75650637311489,0.37671027336384,34.7150441677377));
#17251=CARTESIAN_POINT('Ctrl Pts',(6.74594505157208,0.566133396007559,34.7239837276401));
#17252=CARTESIAN_POINT('Ctrl Pts',(6.72740415662827,0.755267750292087,34.7329232875426));
#17253=CARTESIAN_POINT('Ctrl Pts',(6.70091245562786,0.943430581448054,34.741862847445));
#17254=CARTESIAN_POINT('Ctrl Pts',(6.6753954442371,1.12467047638163,34.7504735007155));
#17255=CARTESIAN_POINT('Ctrl Pts',(6.64250224987259,1.3050087111855,34.759084153986));
#17256=CARTESIAN_POINT('Ctrl Pts',(6.60231145869739,1.48383705384156,34.7676948072564));
#17257=CARTESIAN_POINT('Ctrl Pts',(6.56215871079495,1.66249612350699,34.7762973099675));
#17258=CARTESIAN_POINT('Ctrl Pts',(6.51472220476322,1.83964785390516,34.7848998126785));
#17259=CARTESIAN_POINT('Ctrl Pts',(6.46013190646794,2.01469222240889,34.7935023153896));
#17260=CARTESIAN_POINT('Ctrl Pts',(6.40560304845452,2.18953958199941,34.802095136157));
#17261=CARTESIAN_POINT('Ctrl Pts',(6.34393655118883,2.36228402081068,34.8106879569245));
#17262=CARTESIAN_POINT('Ctrl Pts',(6.2753127831944,2.53233853840219,34.8192807776919));
#17263=CARTESIAN_POINT('Ctrl Pts',(6.26722516042807,2.55238023573515,34.8202934806503));
#17264=CARTESIAN_POINT('Ctrl Pts',(6.25904096073811,2.57238458649186,34.8213061836087));
#17265=CARTESIAN_POINT('Ctrl Pts',(6.25076052528401,2.59235064286281,34.8223188865671));
#17266=CARTESIAN_POINT('Ctrl Pts',(6.18048080851004,2.76181139098665,34.8309141443272));
#17267=CARTESIAN_POINT('Ctrl Pts',(6.10334728356888,2.92831265800815,34.8395094020873));
#17268=CARTESIAN_POINT('Ctrl Pts',(6.01964288437314,3.09130854891838,34.8481046598474));
#17269=CARTESIAN_POINT('Ctrl Pts',(5.9358600995574,3.2544570785679,34.8567079667018));
#17270=CARTESIAN_POINT('Ctrl Pts',(5.84549429766296,3.41409340821317,34.8653112735563));
#17271=CARTESIAN_POINT('Ctrl Pts',(5.74887339275734,3.56969798639139,34.8739145804107));
#17272=CARTESIAN_POINT('Ctrl Pts',(5.64824655162947,3.73175398433929,34.8828745833507));
#17273=CARTESIAN_POINT('Ctrl Pts',(5.54083509015897,3.88943647468561,34.8918345862906));
#17274=CARTESIAN_POINT('Ctrl Pts',(5.42705710653814,4.04219496837719,34.9007945892306));
#17275=CARTESIAN_POINT('Ctrl Pts',(5.31750972899516,4.18927344392038,34.9094214324354));
#17276=CARTESIAN_POINT('Ctrl Pts',(5.20206096701656,4.33178729701084,34.9180482756402));
#17277=CARTESIAN_POINT('Ctrl Pts',(5.08112333419013,4.46928122439712,34.9266751188449));
#17278=CARTESIAN_POINT('Ctrl Pts',(4.96007011555765,4.60690656122189,34.9353102071311));
#17279=CARTESIAN_POINT('Ctrl Pts',(4.83351776288989,4.73950217293558,34.9439452954172));
#17280=CARTESIAN_POINT('Ctrl Pts',(4.70191519813217,4.86665002538437,34.9525803837034));
#17281=CARTESIAN_POINT('Ctrl Pts',(4.57011717715539,4.99398671791047,34.9612282968285));
#17282=CARTESIAN_POINT('Ctrl Pts',(4.43325418017205,5.11585927647829,34.9698762099537));
#17283=CARTESIAN_POINT('Ctrl Pts',(4.2918088253146,5.23188933435635,34.9785241230789));
#17284=CARTESIAN_POINT('Ctrl Pts',(4.27594080974908,5.24490614050267,34.9794942872827));
#17285=CARTESIAN_POINT('Ctrl Pts',(4.26001515371489,5.25784946086792,34.9804644514865));
#17286=CARTESIAN_POINT('Ctrl Pts',(4.24403256126565,5.27071879527991,34.9814346156904));
#17287=CARTESIAN_POINT('Ctrl Pts',(4.10852187633418,5.37983327882315,34.9896602909789));
#17288=CARTESIAN_POINT('Ctrl Pts',(3.96862187091144,5.48386222780802,34.9978859662674));
#17289=CARTESIAN_POINT('Ctrl Pts',(3.82475034660732,5.58243439604329,35.0061116415559));
#17290=CARTESIAN_POINT('Ctrl Pts',(3.68105229940655,5.68088770813729,35.014327398507));
#17291=CARTESIAN_POINT('Ctrl Pts',(3.53339256754797,5.77389714739813,35.022543155458));
#17292=CARTESIAN_POINT('Ctrl Pts',(3.38222220039914,5.86113145963535,35.0307589124091));
#17293=CARTESIAN_POINT('Ctrl Pts',(3.28916596746455,5.91483045258312,35.0358163016779));
#17294=CARTESIAN_POINT('Ctrl Pts',(3.19478012133075,5.96634185834478,35.0408736909467));
#17295=CARTESIAN_POINT('Ctrl Pts',(3.09917575053259,6.01559628526639,35.0459310802154));
#17296=CARTESIAN_POINT('Ctrl Pts',(3.09917575053263,6.01559628526637,33.0456763245139));
#17297=CARTESIAN_POINT('Ctrl Pts',(2.94420350634443,6.09543645379131,33.0539103182196));
#17298=CARTESIAN_POINT('Ctrl Pts',(2.7863355469165,6.16918564830321,33.0621443119252));
#17299=CARTESIAN_POINT('Ctrl Pts',(2.62609851799988,6.23665740391108,33.0703783056308));
#17300=CARTESIAN_POINT('Ctrl Pts',(2.61528137133451,6.24121223047716,33.0709341591571));
#17301=CARTESIAN_POINT('Ctrl Pts',(2.60445343349253,6.24573846840104,33.0714900126833));
#17302=CARTESIAN_POINT('Ctrl Pts',(2.59361486864044,6.25023606859511,33.0720458662095));
#17303=CARTESIAN_POINT('Ctrl Pts',(2.43462246349058,6.31621198717994,33.0801997583762));
#17304=CARTESIAN_POINT('Ctrl Pts',(2.27285054793751,6.37622538676165,33.088353650543));
#17305=CARTESIAN_POINT('Ctrl Pts',(2.10879019303076,6.43003055372036,33.0965075427097));
#17306=CARTESIAN_POINT('Ctrl Pts',(1.9449300375929,6.48377006334305,33.1046514848499));
#17307=CARTESIAN_POINT('Ctrl Pts',(1.77878734502059,6.53131630744089,33.1127954269901));
#17308=CARTESIAN_POINT('Ctrl Pts',(1.61087531091298,6.5724705958027,33.1209393691303));
#17309=CARTESIAN_POINT('Ctrl Pts',(1.44313283426488,6.61358332659169,33.1290750875232));
#17310=CARTESIAN_POINT('Ctrl Pts',(1.27362492547906,6.6483168650809,33.1372108059161));
#17311=CARTESIAN_POINT('Ctrl Pts',(1.10288217885207,6.67652154190867,33.145346524309));
#17312=CARTESIAN_POINT('Ctrl Pts',(0.932275932358765,6.70470367053317,33.1534757386092));
#17313=CARTESIAN_POINT('Ctrl Pts',(0.760437172698095,6.72636727073683,33.1616049529094));
#17314=CARTESIAN_POINT('Ctrl Pts',(0.587908988690094,6.74141320651816,33.1697341672096));
#17315=CARTESIAN_POINT('Ctrl Pts',(0.415482455990325,6.75645027743451,33.177858591885));
#17316=CARTESIAN_POINT('Ctrl Pts',(0.24236767122647,6.7648774170212,33.1859830165605));
#17317=CARTESIAN_POINT('Ctrl Pts',(0.0691151854357627,6.76664703462078,
33.1941074412359));
#17318=CARTESIAN_POINT('Ctrl Pts',(-0.105189053854327,6.76842739493204,
33.2022811863701));
#17319=CARTESIAN_POINT('Ctrl Pts',(-0.279632301184222,6.76346907674447,
33.2104549315043));
#17320=CARTESIAN_POINT('Ctrl Pts',(-0.45365088200447,6.75177679409328,33.2186286766385));
#17321=CARTESIAN_POINT('Ctrl Pts',(-0.626555098754313,6.74015938539881,
33.2267500795006));
#17322=CARTESIAN_POINT('Ctrl Pts',(-0.799039704118879,6.72189405262479,
33.2348714823628));
#17323=CARTESIAN_POINT('Ctrl Pts',(-0.970554318162976,6.69703765223813,
33.2429928852249));
#17324=CARTESIAN_POINT('Ctrl Pts',(-1.14208219281405,6.67217933008546,33.2511149159912));
#17325=CARTESIAN_POINT('Ctrl Pts',(-1.31263956454788,6.64072897771616,33.2592369467574));
#17326=CARTESIAN_POINT('Ctrl Pts',(-1.48168392233174,6.60279499562902,33.2673589775237));
#17327=CARTESIAN_POINT('Ctrl Pts',(-1.65077353968421,6.56485085718004,33.2754831828648));
#17328=CARTESIAN_POINT('Ctrl Pts',(-1.81834897952148,6.52041971260246,33.2836073882059));
#17329=CARTESIAN_POINT('Ctrl Pts',(-1.98388066364218,6.46966046345762,33.291731593547));
#17330=CARTESIAN_POINT('Ctrl Pts',(-2.15120411370535,6.41835178056318,33.2999437377895));
#17331=CARTESIAN_POINT('Ctrl Pts',(-2.31643893803346,6.36057730971967,33.3081558820319));
#17332=CARTESIAN_POINT('Ctrl Pts',(-2.47905746567104,6.29655168182559,33.3163680262744));
#17333=CARTESIAN_POINT('Ctrl Pts',(-2.64019146537982,6.23311053734893,33.3245052026908));
#17334=CARTESIAN_POINT('Ctrl Pts',(-2.79875642796621,6.16353209787753,33.3326423791073));
#17335=CARTESIAN_POINT('Ctrl Pts',(-2.95426280511298,6.08807196724267,33.3407795555238));
#17336=CARTESIAN_POINT('Ctrl Pts',(-3.11191820320259,6.01156901505888,33.3490291836792));
#17337=CARTESIAN_POINT('Ctrl Pts',(-3.26642951438578,5.92902080207527,33.3572788118347));
#17338=CARTESIAN_POINT('Ctrl Pts',(-3.41731639764043,5.84073947701983,33.3655284399901));
#17339=CARTESIAN_POINT('Ctrl Pts',(-3.56820328089505,5.7524581519644,33.3737780681456));
#17340=CARTESIAN_POINT('Ctrl Pts',(-3.71546544594209,5.65844397520847,33.382027696301));
#17341=CARTESIAN_POINT('Ctrl Pts',(-3.85865710243923,5.55905157070838,33.3902773244565));
#17342=CARTESIAN_POINT('Ctrl Pts',(-4.00063037221616,5.46050487460146,33.3984567583168));
#17343=CARTESIAN_POINT('Ctrl Pts',(-4.13903662439936,5.35636963765497,33.4066361921772));
#17344=CARTESIAN_POINT('Ctrl Pts',(-4.27340384810683,5.24693325200405,33.4148156260376));
#17345=CARTESIAN_POINT('Ctrl Pts',(-4.40761908259811,5.13762065510174,33.4229858077477));
#17346=CARTESIAN_POINT('Ctrl Pts',(-4.53780410542421,5.02301907483016,33.4311559894578));
#17347=CARTESIAN_POINT('Ctrl Pts',(-4.66351509958021,4.90345958645397,33.4393261711679));
#17348=CARTESIAN_POINT('Ctrl Pts',(-4.78910994358985,4.78401056456616,33.4474888040729));
#17349=CARTESIAN_POINT('Ctrl Pts',(-4.91023872837106,4.6596130045306,33.4556514369778));
#17350=CARTESIAN_POINT('Ctrl Pts',(-5.02648999868304,4.53063872904686,33.4638140698828));
#17351=CARTESIAN_POINT('Ctrl Pts',(-5.14265793676042,4.40175690601164,33.471970851579));
#17352=CARTESIAN_POINT('Ctrl Pts',(-5.25395508100174,4.26830516978556,33.4801276332753));
#17353=CARTESIAN_POINT('Ctrl Pts',(-5.36000619247849,4.13069275262543,33.4882844149716));
#17354=CARTESIAN_POINT('Ctrl Pts',(-5.46600324239429,3.99315048599908,33.4964370385941));
#17355=CARTESIAN_POINT('Ctrl Pts',(-5.56675936506153,3.85145205028661,33.5045896622165));
#17356=CARTESIAN_POINT('Ctrl Pts',(-5.66193904021825,3.7060403808988,33.512742285839));
#17357=CARTESIAN_POINT('Ctrl Pts',(-5.75710247557083,3.56065352202884,33.5208935184396));
#17358=CARTESIAN_POINT('Ctrl Pts',(-5.84669115424689,3.41155499152871,33.5290447510402));
#17359=CARTESIAN_POINT('Ctrl Pts',(-5.93041227645633,3.25921757961264,33.5371959836407));
#17360=CARTESIAN_POINT('Ctrl Pts',(-6.01412923751425,3.10688773925123,33.5453468111045));
#17361=CARTESIAN_POINT('Ctrl Pts',(-6.09197904718912,2.9513196561671,33.5534976385682));
#17362=CARTESIAN_POINT('Ctrl Pts',(-6.16371442687925,2.79301154023406,33.5616484660319));
#17363=CARTESIAN_POINT('Ctrl Pts',(-6.23545969583281,2.63468160033258,33.5698004171486));
#17364=CARTESIAN_POINT('Ctrl Pts',(-6.30108870615159,2.47361120636607,33.5779523682654));
#17365=CARTESIAN_POINT('Ctrl Pts',(-6.36040197912863,2.31031938569034,33.5861043193822));
#17366=CARTESIAN_POINT('Ctrl Pts',(-6.41973455400394,2.14697442611413,33.5942589233307));
#17367=CARTESIAN_POINT('Ctrl Pts',(-6.47274717479817,1.98140694165762,33.6024135272792));
#17368=CARTESIAN_POINT('Ctrl Pts',(-6.51928996406023,1.81415196841487,33.6105681312277));
#17369=CARTESIAN_POINT('Ctrl Pts',(-6.56588084541217,1.64672417267195,33.6187311612278));
#17370=CARTESIAN_POINT('Ctrl Pts',(-6.60598844634254,1.47760575605507,33.6268941912279));
#17371=CARTESIAN_POINT('Ctrl Pts',(-6.63951365496063,1.30734365244618,33.635057221228));
#17372=CARTESIAN_POINT('Ctrl Pts',(-6.67305825389327,1.13698307261951,33.6432249725625));
#17373=CARTESIAN_POINT('Ctrl Pts',(-6.70001281730768,0.965477845723865,
33.651392723897));
#17374=CARTESIAN_POINT('Ctrl Pts',(-6.72033005790458,0.793380685941044,
33.6595604752315));
#17375=CARTESIAN_POINT('Ctrl Pts',(-6.74067470280054,0.621051398079019,
33.6677392433918));
#17376=CARTESIAN_POINT('Ctrl Pts',(-6.75436411559209,0.448128943948057,
33.6759180115521));
#17377=CARTESIAN_POINT('Ctrl Pts',(-6.76140309140205,0.275167649949594,
33.6840967797123));
#17378=CARTESIAN_POINT('Ctrl Pts',(-6.76515634402121,0.182942950328629,
33.6884577810636));
#17379=CARTESIAN_POINT('Ctrl Pts',(-6.76701967731049,0.0907071641554947,
33.692818782415));
#17380=CARTESIAN_POINT('Ctrl Pts',(-6.76699984329972,-0.00145629033193495,
33.6971797837663));
#17381=CARTESIAN_POINT('',(-6.76699867180277,-0.0042397900355361,33.3028202161613));
#17382=CARTESIAN_POINT('Ctrl Pts',(3.0991757505326,6.01559628526638,32.6511251802053));
#17383=CARTESIAN_POINT('Ctrl Pts',(2.94517234236558,6.09493731904879,32.6592642952129));
#17384=CARTESIAN_POINT('Ctrl Pts',(2.78824240218256,6.16829766025846,32.6674034102206));
#17385=CARTESIAN_POINT('Ctrl Pts',(2.62890093239468,6.23547663676598,32.6755425252283));
#17386=CARTESIAN_POINT('Ctrl Pts',(2.46945010388479,6.30270171933131,32.683687226247));
#17387=CARTESIAN_POINT('Ctrl Pts',(2.30758478925735,6.36373685678097,32.6918319272657));
#17388=CARTESIAN_POINT('Ctrl Pts',(2.14383537037269,6.41843118719357,32.6999766282845));
#17389=CARTESIAN_POINT('Ctrl Pts',(1.97985080910237,6.47320405807014,32.7081330250053));
#17390=CARTESIAN_POINT('Ctrl Pts',(1.8139770908749,6.52161784001265,32.7162894217262));
#17391=CARTESIAN_POINT('Ctrl Pts',(1.64675585234037,6.56357251523763,32.7244458184471));
#17392=CARTESIAN_POINT('Ctrl Pts',(1.58335359791805,6.57947971109463,32.7275383319615));
#17393=CARTESIAN_POINT('Ctrl Pts',(1.51975769263817,6.59445890225035,32.7306308454759));
#17394=CARTESIAN_POINT('Ctrl Pts',(1.45599782810842,6.60850658806841,32.7337233589903));
#17395=CARTESIAN_POINT('Ctrl Pts',(1.28625300447666,6.64590506702078,32.7419564091223));
#17396=CARTESIAN_POINT('Ctrl Pts',(1.11481819085282,6.67681397247402,32.7501894592543));
#17397=CARTESIAN_POINT('Ctrl Pts',(0.942230479786608,6.70108130997984,32.7584225093863));
#17398=CARTESIAN_POINT('Ctrl Pts',(0.769848294154741,6.72531974881697,32.7666457552212));
#17399=CARTESIAN_POINT('Ctrl Pts',(0.596316296124643,6.74293231927,32.7748690010561));
#17400=CARTESIAN_POINT('Ctrl Pts',(0.422184442116325,6.75381738699196,32.7830922468909));
#17401=CARTESIAN_POINT('Ctrl Pts',(0.248225099513035,6.76469167094127,32.7913073460044));
#17402=CARTESIAN_POINT('Ctrl Pts',(0.0736674394620265,6.76885170319191,
32.7995224451179));
#17403=CARTESIAN_POINT('Ctrl Pts',(-0.10093063706062,6.76624726170294,32.8077375442314));
#17404=CARTESIAN_POINT('Ctrl Pts',(-0.275390673851752,6.76364487932259,
32.8159461483703));
#17405=CARTESIAN_POINT('Ctrl Pts',(-0.449890706938323,6.75428868084474,
32.8241547525092));
#17406=CARTESIAN_POINT('Ctrl Pts',(-0.623869890403432,6.7381804190633,32.8323633566481));
#17407=CARTESIAN_POINT('Ctrl Pts',(-0.79774632413001,6.72208167060209,32.8405671128971));
#17408=CARTESIAN_POINT('Ctrl Pts',(-0.971102165329179,6.69923883576472,
32.848770869146));
#17409=CARTESIAN_POINT('Ctrl Pts',(-1.14337865411116,6.66970570964889,32.856974625395));
#17410=CARTESIAN_POINT('Ctrl Pts',(-1.3156041706225,6.64018132164066,32.8651759543593));
#17411=CARTESIAN_POINT('Ctrl Pts',(-1.48675061762056,6.60397064206156,32.8733772833236));
#17412=CARTESIAN_POINT('Ctrl Pts',(-1.65626617800443,6.56117911259848,32.8815786122879));
#17413=CARTESIAN_POINT('Ctrl Pts',(-1.82575836057417,6.51839348449585,32.8897788102106));
#17414=CARTESIAN_POINT('Ctrl Pts',(-1.99361975702006,6.46902890094111,32.8979790081333));
#17415=CARTESIAN_POINT('Ctrl Pts',(-2.15931051581672,6.41324154357867,32.906179206056));
#17416=CARTESIAN_POINT('Ctrl Pts',(-2.32500845081249,6.35745177002122,32.9143797591359));
#17417=CARTESIAN_POINT('Ctrl Pts',(-2.48853522127145,6.29523878273873,32.9225803122157));
#17418=CARTESIAN_POINT('Ctrl Pts',(-2.6493678107698,6.22680810714903,32.9307808652955));
#17419=CARTESIAN_POINT('Ctrl Pts',(-2.81023651207198,6.15836206679313,32.9389832596488));
#17420=CARTESIAN_POINT('Ctrl Pts',(-2.96840949795698,6.08369569781668,32.947185654002));
#17421=CARTESIAN_POINT('Ctrl Pts',(-3.1233852931445,6.00306199456316,32.9553880483552));
#17422=CARTESIAN_POINT('Ctrl Pts',(-3.27850601794381,5.92235288462246,32.963598113389));
#17423=CARTESIAN_POINT('Ctrl Pts',(-3.43042326015574,5.83566545660226,32.9718081784228));
#17424=CARTESIAN_POINT('Ctrl Pts',(-3.57866083317763,5.74329832422802,32.9800182434567));
#17425=CARTESIAN_POINT('Ctrl Pts',(-3.72696935007209,5.65088698658291,32.988232237682));
#17426=CARTESIAN_POINT('Ctrl Pts',(-3.87159439023403,5.55279072593261,32.9964462319073));
#17427=CARTESIAN_POINT('Ctrl Pts',(-4.01209025154482,5.44935049464237,33.0046602261326));
#17428=CARTESIAN_POINT('Ctrl Pts',(-4.15277765550822,5.34576923986501,33.0128854187678));
#17429=CARTESIAN_POINT('Ctrl Pts',(-4.28932434994916,5.23682967756364,33.021110611403));
#17430=CARTESIAN_POINT('Ctrl Pts',(-4.42131818512401,5.12291269746926,33.0293358040382));
#17431=CARTESIAN_POINT('Ctrl Pts',(-4.54001995838984,5.02046740125994,33.0367327021581));
#17432=CARTESIAN_POINT('Ctrl Pts',(-4.65504001218599,4.91399732511296,33.0441296002781));
#17433=CARTESIAN_POINT('Ctrl Pts',(-4.76610547379797,4.80380345274795,33.051526498398));
#17434=CARTESIAN_POINT('Ctrl Pts',(-4.89592587200022,4.67500182367038,33.0601724648889));
#17435=CARTESIAN_POINT('Ctrl Pts',(-5.02063765702566,4.54081990971175,33.0688184313798));
#17436=CARTESIAN_POINT('Ctrl Pts',(-5.1397965093271,4.40167932074895,33.0774643978707));
#17437=CARTESIAN_POINT('Ctrl Pts',(-5.258802941257,4.26271671151537,33.0860993049951));
#17438=CARTESIAN_POINT('Ctrl Pts',(-5.37227040676659,4.11880830574691,33.0947342121194));
#17439=CARTESIAN_POINT('Ctrl Pts',(-5.47979155368142,3.97041226174333,33.1033691192438));
#17440=CARTESIAN_POINT('Ctrl Pts',(-5.59088231589151,3.81708958885203,33.1122906983153));
#17441=CARTESIAN_POINT('Ctrl Pts',(-5.69562490032188,3.65897639025737,33.1212122773868));
#17442=CARTESIAN_POINT('Ctrl Pts',(-5.79361342723059,3.49661728758145,33.1301338564583));
#17443=CARTESIAN_POINT('Ctrl Pts',(-5.88819141363774,3.33990917602604,33.138744915434));
#17444=CARTESIAN_POINT('Ctrl Pts',(-5.97647736241497,3.17924601535045,33.1473559744097));
#17445=CARTESIAN_POINT('Ctrl Pts',(-6.05814850899848,3.01514935665209,33.1559670333854));
#17446=CARTESIAN_POINT('Ctrl Pts',(-6.13974263592032,2.8512074486786,33.164569971735));
#17447=CARTESIAN_POINT('Ctrl Pts',(-6.21473426228188,2.68383877041427,33.1731729100845));
#17448=CARTESIAN_POINT('Ctrl Pts',(-6.2828456701583,2.51359091440375,33.1817758484341));
#17449=CARTESIAN_POINT('Ctrl Pts',(-6.35088080901431,2.34353369660803,33.1903691534828));
#17450=CARTESIAN_POINT('Ctrl Pts',(-6.41205098612041,2.17060401541842,33.1989624585316));
#17451=CARTESIAN_POINT('Ctrl Pts',(-6.4661258061129,1.99537115833642,33.2075557635804));
#17452=CARTESIAN_POINT('Ctrl Pts',(-6.47215062617444,1.97584734978866,33.2085131984208));
#17453=CARTESIAN_POINT('Ctrl Pts',(-6.4780874159619,1.95629497210247,33.2094706332613));
#17454=CARTESIAN_POINT('Ctrl Pts',(-6.48393589367517,1.93671482844296,33.2104280681017));
#17455=CARTESIAN_POINT('Ctrl Pts',(-6.53278554370796,1.77317087525512,33.2184250818853));
#17456=CARTESIAN_POINT('Ctrl Pts',(-6.57543908001728,1.60779208142203,33.2264220956689));
#17457=CARTESIAN_POINT('Ctrl Pts',(-6.61177080042785,1.44110231510803,33.2344191094524));
#17458=CARTESIAN_POINT('Ctrl Pts',(-6.64810882117877,1.27438364286145,33.2424175100107));
#17459=CARTESIAN_POINT('Ctrl Pts',(-6.67812277164572,1.10635391685539,33.2504159105689));
#17460=CARTESIAN_POINT('Ctrl Pts',(-6.70173829295727,0.937546186974363,
33.2584143111271));
#17461=CARTESIAN_POINT('Ctrl Pts',(-6.7253752626298,0.768585140591094,33.2664199760848));
#17462=CARTESIAN_POINT('Ctrl Pts',(-6.74260215172067,0.598845054670808,
33.2744256410426));
#17463=CARTESIAN_POINT('Ctrl Pts',(-6.75339654668035,0.428863711784925,
33.2824313060004));
#17464=CARTESIAN_POINT('Ctrl Pts',(-6.76256030552012,0.28456029882994,33.2892276093873));
#17465=CARTESIAN_POINT('Ctrl Pts',(-6.76708909581097,0.140083192540306,
33.2960239127743));
#17466=CARTESIAN_POINT('Ctrl Pts',(-6.76699867180277,-0.0042397900354902,
33.3028202161613));
#17467=CARTESIAN_POINT('Ctrl Pts',(-6.76699867180239,-0.00423979064372843,
33.3028202161899));
#17468=CARTESIAN_POINT('Ctrl Pts',(-6.76685118845725,-0.239633394842735,
33.3139051197925));
#17469=CARTESIAN_POINT('Ctrl Pts',(-6.75441678713885,-0.47460457998798,
33.3249900233951));
#17470=CARTESIAN_POINT('Ctrl Pts',(-6.72985396171361,-0.708064018297538,
33.3360749269978));
#17471=CARTESIAN_POINT('Ctrl Pts',(-6.70529113628837,-0.941523456607097,
33.3471598306004));
#17472=CARTESIAN_POINT('Ctrl Pts',(-6.66859999616083,-1.17347154533364,
33.358244734203));
#17473=CARTESIAN_POINT('Ctrl Pts',(-6.61999462935251,-1.40284001487838,
33.3693296378057));
#17474=CARTESIAN_POINT('Ctrl Pts',(-6.58392508836533,-1.57305198850748,
33.377555630347));
#17475=CARTESIAN_POINT('Ctrl Pts',(-6.5412393073043,-1.74209535196447,33.3857816228884));
#17476=CARTESIAN_POINT('Ctrl Pts',(-6.49202667257248,-1.90941841475552,
33.3940076154297));
#17477=CARTESIAN_POINT('Ctrl Pts',(-6.44286563092718,-2.07656606094264,
33.4022249840811));
#17478=CARTESIAN_POINT('Ctrl Pts',(-6.38719146195261,-2.24199665701822,
33.4104423527325));
#17479=CARTESIAN_POINT('Ctrl Pts',(-6.32514463314709,-2.40516826225746,
33.418659721384));
#17480=CARTESIAN_POINT('Ctrl Pts',(-6.26315043712016,-2.56820145309043,
33.4268701194463));
#17481=CARTESIAN_POINT('Ctrl Pts',(-6.19479447420671,-2.72897913653461,
33.4350805175087));
#17482=CARTESIAN_POINT('Ctrl Pts',(-6.12026715130905,-2.88697402077113,
33.4432909155711));
#17483=CARTESIAN_POINT('Ctrl Pts',(-6.0457881396868,-3.0448664870746,33.4514959913599));
#17484=CARTESIAN_POINT('Ctrl Pts',(-5.96514588908751,-3.19997942454144,
33.4597010671487));
#17485=CARTESIAN_POINT('Ctrl Pts',(-5.87857912702016,-3.35180495365749,
33.4679061429375));
#17486=CARTESIAN_POINT('Ctrl Pts',(-5.79205116738638,-3.5035624289401,33.476107540907));
#17487=CARTESIAN_POINT('Ctrl Pts',(-5.69960416408486,-3.65203512099309,
33.4843089388765));
#17488=CARTESIAN_POINT('Ctrl Pts',(-5.60152308524453,-3.79673914372224,
33.492510336846));
#17489=CARTESIAN_POINT('Ctrl Pts',(-5.50344968893109,-3.94143183202726,
33.5007110924137));
#17490=CARTESIAN_POINT('Ctrl Pts',(-5.39974328975629,-4.08235613776238,
33.5089118479814));
#17491=CARTESIAN_POINT('Ctrl Pts',(-5.29073274692962,-4.21905629265202,
33.5171126035491));
#17492=CARTESIAN_POINT('Ctrl Pts',(-5.18172275782461,-4.35575575316995,
33.5253133174609));
#17493=CARTESIAN_POINT('Ctrl Pts',(-5.06740890133723,-4.48823082472467,
33.5335140313726));
#17494=CARTESIAN_POINT('Ctrl Pts',(-4.94816089564999,-4.61605813988086,
33.5417147452844));
#17495=CARTESIAN_POINT('Ctrl Pts',(-4.82889188497798,-4.74390797122751,
33.549916903714));
#17496=CARTESIAN_POINT('Ctrl Pts',(-4.70468723798313,-4.86710815304147,
33.5581190621436));
#17497=CARTESIAN_POINT('Ctrl Pts',(-4.57595419253586,-4.98527152999849,
33.5663212205732));
#17498=CARTESIAN_POINT('Ctrl Pts',(-4.44717514147813,-5.10347713526039,
33.5745263102262));
#17499=CARTESIAN_POINT('Ctrl Pts',(-4.31386473202012,-5.21664210774924,
33.5827313998791));
#17500=CARTESIAN_POINT('Ctrl Pts',(-4.17646401910527,-5.32441896333478,
33.590936489532));
#17501=CARTESIAN_POINT('Ctrl Pts',(-4.03890634212075,-5.43231894123542,
33.5991509525298));
#17502=CARTESIAN_POINT('Ctrl Pts',(-3.89724930873116,-5.53481828364786,
33.6073654155276));
#17503=CARTESIAN_POINT('Ctrl Pts',(-3.75196462336234,-5.63161171113896,
33.6155798785254));
#17504=CARTESIAN_POINT('Ctrl Pts',(-3.60659386140927,-5.72846248567662,
33.6237992083329));
#17505=CARTESIAN_POINT('Ctrl Pts',(-3.45759146836291,-5.81960041982921,
33.6320185381403));
#17506=CARTESIAN_POINT('Ctrl Pts',(-3.30545449063006,-5.90476583874192,
33.6402378679478));
#17507=CARTESIAN_POINT('Ctrl Pts',(-3.15308178587413,-5.99006321630775,
33.6484699331085));
#17508=CARTESIAN_POINT('Ctrl Pts',(-2.99756510958667,-6.06936942273954,
33.6567019982692));
#17509=CARTESIAN_POINT('Ctrl Pts',(-2.83942347525055,-6.14247208607383,
33.6649340634299));
#17510=CARTESIAN_POINT('Ctrl Pts',(-2.69727441911673,-6.20818200893797,
33.672333634691));
#17511=CARTESIAN_POINT('Ctrl Pts',(-2.55300490545345,-6.26888024119241,
33.6797332059522));
#17512=CARTESIAN_POINT('Ctrl Pts',(-2.4070019758854,-6.32444704998657,33.6871327772133));
#17513=CARTESIAN_POINT('Ctrl Pts',(-2.2460844338632,-6.3856901655571,33.6952882356201));
#17514=CARTESIAN_POINT('Ctrl Pts',(-2.08256551603612,-6.44088765077319,
33.7034436940269));
#17515=CARTESIAN_POINT('Ctrl Pts',(-1.91694366712445,-6.4898086240714,33.7115991524337));
#17516=CARTESIAN_POINT('Ctrl Pts',(-1.75152340177355,-6.53867005411454,
33.7197446845756));
#17517=CARTESIAN_POINT('Ctrl Pts',(-1.58400564690597,-6.58127007629404,
33.7278902167174));
#17518=CARTESIAN_POINT('Ctrl Pts',(-1.41490954025648,-6.61742548072067,
33.7360357488593));
#17519=CARTESIAN_POINT('Ctrl Pts',(-1.245983688277,-6.65354448202383,33.7441730796599));
#17520=CARTESIAN_POINT('Ctrl Pts',(-1.07548300301375,-6.68323170772014,
33.7523104104605));
#17521=CARTESIAN_POINT('Ctrl Pts',(-0.903942533023143,-6.70635347241642,
33.760447741261));
#17522=CARTESIAN_POINT('Ctrl Pts',(-0.732538729053215,-6.72945681603939,
33.768578589063));
#17523=CARTESIAN_POINT('Ctrl Pts',(-0.560097150334056,-6.74600506502437,
33.7767094368651));
#17524=CARTESIAN_POINT('Ctrl Pts',(-0.387163810635177,-6.75591542159421,
33.7848402846671));
#17525=CARTESIAN_POINT('Ctrl Pts',(-0.214331919012058,-6.76581996444065,
33.7929663626609));
#17526=CARTESIAN_POINT('Ctrl Pts',(-0.04100920490468,-6.76909434882516,
33.8010924406546));
#17527=CARTESIAN_POINT('Ctrl Pts',(0.132252411158641,-6.76570752395806,
33.8092185186484));
#17528=CARTESIAN_POINT('Ctrl Pts',(0.306128381267504,-6.76230869002857,
33.8173734102306));
#17529=CARTESIAN_POINT('Ctrl Pts',(0.479942449932698,-6.75220127770795,
33.8255283018128));
#17530=CARTESIAN_POINT('Ctrl Pts',(0.653135381334614,-6.73540668212758,
33.833683193395));
#17531=CARTESIAN_POINT('Ctrl Pts',(0.825652920859281,-6.71867757959791,
33.8418062837513));
#17532=CARTESIAN_POINT('Ctrl Pts',(0.997553793903495,-6.69531340813728,
33.8499293741076));
#17533=CARTESIAN_POINT('Ctrl Pts',(1.16828937258548,-6.66538738123328,33.8580524644639));
#17534=CARTESIAN_POINT('Ctrl Pts',(1.33903835820453,-6.63545900440103,33.8661761926823));
#17535=CARTESIAN_POINT('Ctrl Pts',(1.50862150684899,-6.59896780888909,33.8742999209008));
#17536=CARTESIAN_POINT('Ctrl Pts',(1.6764995891936,-6.55603829514698,33.8824236491192));
#17537=CARTESIAN_POINT('Ctrl Pts',(1.84442279269734,-6.51309724309448,33.8905495607795));
#17538=CARTESIAN_POINT('Ctrl Pts',(2.01063966311429,-6.46371451775911,33.8986754724398));
#17539=CARTESIAN_POINT('Ctrl Pts',(2.17462539819144,-6.40806471390081,33.9068013841001));
#17540=CARTESIAN_POINT('Ctrl Pts',(2.339659839091,-6.35205902376195,33.9149792618102));
#17541=CARTESIAN_POINT('Ctrl Pts',(2.5024341532386,-6.28970594034005,33.9231571395203));
#17542=CARTESIAN_POINT('Ctrl Pts',(2.66243386369257,-6.22123258860036,33.9313350172304));
#17543=CARTESIAN_POINT('Ctrl Pts',(2.82166993023045,-6.15308604531752,33.9394738637038));
#17544=CARTESIAN_POINT('Ctrl Pts',(2.97815751599557,-6.07887773947098,33.9476127101772));
#17545=CARTESIAN_POINT('Ctrl Pts',(3.13141458455669,-5.99887753664181,33.9557515566507));
#17546=CARTESIAN_POINT('Ctrl Pts',(3.28577410902384,-5.91830185173588,33.9639489499791));
#17547=CARTESIAN_POINT('Ctrl Pts',(3.43685613567875,-5.83185081518611,33.9721463433075));
#17548=CARTESIAN_POINT('Ctrl Pts',(3.58419854173878,-5.73984405828222,33.9803437366358));
#17549=CARTESIAN_POINT('Ctrl Pts',(3.73154094779878,-5.64783730137834,33.9885411299642));
#17550=CARTESIAN_POINT('Ctrl Pts',(3.87514345970992,-5.55027508385098,33.9967385232926));
#17551=CARTESIAN_POINT('Ctrl Pts',(4.01457877321954,-5.44751744133189,34.004935916621));
#17552=CARTESIAN_POINT('Ctrl Pts',(4.15450423878479,-5.34439857848456,34.013162125958));
#17553=CARTESIAN_POINT('Ctrl Pts',(4.29064966970499,-5.23574089470283,34.021388335295));
#17554=CARTESIAN_POINT('Ctrl Pts',(4.42254851804683,-5.12185060359259,34.0296145446319));
#17555=CARTESIAN_POINT('Ctrl Pts',(4.55429918368309,-5.00808826334537,34.0378315121751));
#17556=CARTESIAN_POINT('Ctrl Pts',(4.68181249782518,-4.88910525393652,34.0460484797183));
#17557=CARTESIAN_POINT('Ctrl Pts',(4.80465159054427,-4.76525047541894,34.0542654472615));
#17558=CARTESIAN_POINT('Ctrl Pts',(4.9273773335949,-4.64150998379304,34.0624748326049));
#17559=CARTESIAN_POINT('Ctrl Pts',(5.04543719402836,-4.51290692889217,34.0706842179482));
#17560=CARTESIAN_POINT('Ctrl Pts',(5.15842799667021,-4.37982986007093,34.0788936032916));
#17561=CARTESIAN_POINT('Ctrl Pts',(5.27133720802551,-4.24684888694069,34.0870970605922));
#17562=CARTESIAN_POINT('Ctrl Pts',(5.37918442128618,-4.10940060718806,34.0953005178928));
#17563=CARTESIAN_POINT('Ctrl Pts',(5.48160385415867,-3.96790980064729,34.1035039751934));
#17564=CARTESIAN_POINT('Ctrl Pts',(5.5839698744761,-3.82649278269609,34.1117031543252));
#17565=CARTESIAN_POINT('Ctrl Pts',(5.68091354373583,-3.68103772770865,34.1199023334571));
#17566=CARTESIAN_POINT('Ctrl Pts',(5.77210981583395,-3.53200187909823,34.128101512589));
#17567=CARTESIAN_POINT('Ctrl Pts',(5.86328890458893,-3.38299411205371,34.1362991468188));
#17568=CARTESIAN_POINT('Ctrl Pts',(5.94872256097374,-3.23040719766393,34.1444967810486));
#17569=CARTESIAN_POINT('Ctrl Pts',(6.02812932199339,-3.07472695980042,34.1526944152784));
#17570=CARTESIAN_POINT('Ctrl Pts',(6.10753035134604,-2.91905795910703,34.160891457794));
#17571=CARTESIAN_POINT('Ctrl Pts',(6.18090518795532,-2.76029639872704,34.1690885003095));
#17572=CARTESIAN_POINT('Ctrl Pts',(6.2480185923347,-2.59895222538622,34.1772855428251));
#17573=CARTESIAN_POINT('Ctrl Pts',(6.31513935014388,-2.43759037401126,34.185483483468));
#17574=CARTESIAN_POINT('Ctrl Pts',(6.375997171133,-2.27364567715848,34.1936814241108));
#17575=CARTESIAN_POINT('Ctrl Pts',(6.43040516569789,-2.10764759980551,34.2018793647536));
#17576=CARTESIAN_POINT('Ctrl Pts',(6.48482901019461,-1.94160116451853,34.2100796935896));
#17577=CARTESIAN_POINT('Ctrl Pts',(6.53279917396162,-1.77350049797662,34.2182800224256));
#17578=CARTESIAN_POINT('Ctrl Pts',(6.57417877326439,-1.60388978959275,34.2264803512616));
#17579=CARTESIAN_POINT('Ctrl Pts',(6.61560149118333,-1.4341023424498,34.234689225053));
#17580=CARTESIAN_POINT('Ctrl Pts',(6.65041983920748,-1.26280205876364,34.2428980988444));
#17581=CARTESIAN_POINT('Ctrl Pts',(6.67854797676003,-1.09054386528675,34.2511069726358));
#17582=CARTESIAN_POINT('Ctrl Pts',(6.70669121037371,-0.918193222737659,
34.2593202520392));
#17583=CARTESIAN_POINT('Ctrl Pts',(6.7281370315992,-0.744884001142171,34.2675335314427));
#17584=CARTESIAN_POINT('Ctrl Pts',(6.74285157172199,-0.5711757012744,34.2757468108461));
#17585=CARTESIAN_POINT('Ctrl Pts',(6.75758763417243,-0.397213325716036,
34.2839721034615));
#17586=CARTESIAN_POINT('Ctrl Pts',(6.76557272340834,-0.222851063650834,
34.292197396077));
#17587=CARTESIAN_POINT('Ctrl Pts',(6.76682512404348,-0.0486491584089832,
34.3004226886924));
#17588=CARTESIAN_POINT('Ctrl Pts',(6.76795776997406,0.108895538978431,34.3078614778045));
#17589=CARTESIAN_POINT('Ctrl Pts',(6.76358441712264,0.266308916115103,34.3153002669166));
#17590=CARTESIAN_POINT('Ctrl Pts',(6.753754990295,0.423181439887758,34.3227390560288));
#17591=CARTESIAN_POINT('Ctrl Pts',(6.74288509739099,0.596659259387358,34.3309652570476));
#17592=CARTESIAN_POINT('Ctrl Pts',(6.72531175680491,0.769960473067657,34.3391914580664));
#17593=CARTESIAN_POINT('Ctrl Pts',(6.70103960477615,0.942527036865035,34.3474176590853));
#17594=CARTESIAN_POINT('Ctrl Pts',(6.67679471739456,1.11489975849825,34.355634619701));
#17595=CARTESIAN_POINT('Ctrl Pts',(6.64586605179754,1.28653912157858,34.3638515803168));
#17596=CARTESIAN_POINT('Ctrl Pts',(6.60831020194873,1.45688890270342,34.3720685409326));
#17597=CARTESIAN_POINT('Ctrl Pts',(6.57078900042455,1.6270815223064,34.3802779207342));
#17598=CARTESIAN_POINT('Ctrl Pts',(6.52665286786645,1.79598658134815,34.3884873005357));
#17599=CARTESIAN_POINT('Ctrl Pts',(6.47600997914114,1.96305469869396,34.3966966803373));
#17600=CARTESIAN_POINT('Ctrl Pts',(6.42540365142904,2.13000220325879,34.4049001334777));
#17601=CARTESIAN_POINT('Ctrl Pts',(6.36830002772615,2.29511506578169,34.4131035866181));
#17602=CARTESIAN_POINT('Ctrl Pts',(6.30485799355328,2.45785570795507,34.4213070397585));
#17603=CARTESIAN_POINT('Ctrl Pts',(6.24144903426589,2.6205115068826,34.4295062161086));
#17604=CARTESIAN_POINT('Ctrl Pts',(6.17170837754986,2.78079721590573,34.4377053924588));
#17605=CARTESIAN_POINT('Ctrl Pts',(6.095844264536,2.93819191043124,34.4459045688089));
#17606=CARTESIAN_POINT('Ctrl Pts',(6.01999442649988,3.09555698876971,34.4541022023603));
#17607=CARTESIAN_POINT('Ctrl Pts',(5.93802357722017,3.25003181074202,34.4622998359117));
#17608=CARTESIAN_POINT('Ctrl Pts',(5.85018759186039,3.40111660194747,34.4704974694631));
#17609=CARTESIAN_POINT('Ctrl Pts',(5.76235793284728,3.55219051133994,34.4786945125836));
#17610=CARTESIAN_POINT('Ctrl Pts',(5.66866415856292,3.69987456570618,34.4868915557042));
#17611=CARTESIAN_POINT('Ctrl Pts',(5.56940746173311,3.84369477523795,34.4950885988248));
#17612=CARTESIAN_POINT('Ctrl Pts',(5.47013987408253,3.98753076526794,34.503286541356));
#17613=CARTESIAN_POINT('Ctrl Pts',(5.36530835159771,4.12750177055697,34.5114844838872));
#17614=CARTESIAN_POINT('Ctrl Pts',(5.25525668612859,4.26316386770445,34.5196824264183));
#17615=CARTESIAN_POINT('Ctrl Pts',(5.14517294359279,4.39886550666276,34.5278827584268));
#17616=CARTESIAN_POINT('Ctrl Pts',(5.02986625327844,4.53025545733841,34.5360830904352));
#17617=CARTESIAN_POINT('Ctrl Pts',(4.90971987385085,4.65692385167656,34.5442834224436));
#17618=CARTESIAN_POINT('Ctrl Pts',(4.78944826942286,4.7837242687174,34.5524923014144));
#17619=CARTESIAN_POINT('Ctrl Pts',(4.66432714536748,4.90579303715201,34.5607011803851));
#17620=CARTESIAN_POINT('Ctrl Pts',(4.53477643787629,5.02275737603181,34.5689100593559));
#17621=CARTESIAN_POINT('Ctrl Pts',(4.40515618456044,5.13978450408168,34.5771233450433));
#17622=CARTESIAN_POINT('Ctrl Pts',(4.27110188244815,5.25170151029451,34.5853366307307));
#17623=CARTESIAN_POINT('Ctrl Pts',(4.13306546769413,5.35817682050101,34.5935499164181));
#17624=CARTESIAN_POINT('Ctrl Pts',(3.99482712267796,5.46480789096354,34.6017752171302));
#17625=CARTESIAN_POINT('Ctrl Pts',(3.8525953157173,5.5659811489269,34.6100005178422));
#17626=CARTESIAN_POINT('Ctrl Pts',(3.70685086082731,5.66140845510937,34.6182258185543));
#17627=CARTESIAN_POINT('Ctrl Pts',(3.57504258221534,5.7477109423634,34.6256646108483));
#17628=CARTESIAN_POINT('Ctrl Pts',(3.44036181171218,5.82931429266173,34.6331034031423));
#17629=CARTESIAN_POINT('Ctrl Pts',(3.30317982495396,5.90603860840895,34.6405421954363));
#17630=CARTESIAN_POINT('Ctrl Pts',(3.23585590749851,5.94369210521459,34.6441928834763));
#17631=CARTESIAN_POINT('Ctrl Pts',(3.16784100521239,5.980220624714,34.6478435715163));
#17632=CARTESIAN_POINT('Ctrl Pts',(3.09917575053259,6.01559628526639,34.6514942595564));
#17633=CARTESIAN_POINT('Origin',(0.,0.,-3.69717978381041));
#17634=CARTESIAN_POINT('',(3.09917575053255,6.01559628526641,37.0457515827422));
#17635=CARTESIAN_POINT('',(3.09917575053261,6.01559628526638,36.6515495189894));
#17636=CARTESIAN_POINT('',(3.09917575053259,6.01559628526639,-3.69717978381041));
#17637=CARTESIAN_POINT('',(-6.76699911870181,0.00214833398699119,35.69717978381));
#17638=CARTESIAN_POINT('Ctrl Pts',(-6.767,1.16698816081859E-12,35.69717978381));
#17639=CARTESIAN_POINT('Ctrl Pts',(-6.76700000000003,-0.186007249414598,
35.705929295616));
#17640=CARTESIAN_POINT('Ctrl Pts',(-6.75932637295444,-0.37201435552654,
35.7146788074219));
#17641=CARTESIAN_POINT('Ctrl Pts',(-6.74400518266935,-0.557389537154144,
35.7234283192279));
#17642=CARTESIAN_POINT('Ctrl Pts',(-6.72868405709653,-0.742763935810719,
35.7321777940784));
#17643=CARTESIAN_POINT('Ctrl Pts',(-6.70571545652998,-0.927506129694582,
35.740927268929));
#17644=CARTESIAN_POINT('Ctrl Pts',(-6.67517739415654,-1.11098863924953,
35.7496767437795));
#17645=CARTESIAN_POINT('Ctrl Pts',(-6.64463945823072,-1.29447038906647,
35.7584261824015));
#17646=CARTESIAN_POINT('Ctrl Pts',(-6.60653217027124,-1.47669218228365,
35.7671756210235));
#17647=CARTESIAN_POINT('Ctrl Pts',(-6.56098496116673,-1.65703510504273,
35.7759250596455));
#17648=CARTESIAN_POINT('Ctrl Pts',(-6.51543793687469,-1.83737729604194,
35.7846744627657));
#17649=CARTESIAN_POINT('Ctrl Pts',(-6.46245112202579,-2.01584035397248,
35.793423865886));
#17650=CARTESIAN_POINT('Ctrl Pts',(-6.40220448416169,-2.19181813638359,
35.8021732690062));
#17651=CARTESIAN_POINT('Ctrl Pts',(-6.34195808575099,-2.36779521936179,
35.8109226373515));
#17652=CARTESIAN_POINT('Ctrl Pts',(-6.27445201489132,-2.54128677545082,
35.8196720056968));
#17653=CARTESIAN_POINT('Ctrl Pts',(-6.19991555136064,-2.71170355238114,
35.8284213740421));
#17654=CARTESIAN_POINT('Ctrl Pts',(-6.12537937788914,-2.88211966613336,
35.8371707083391));
#17655=CARTESIAN_POINT('Ctrl Pts',(-6.04381298133488,-3.04946076210699,
35.8459200426362));
#17656=CARTESIAN_POINT('Ctrl Pts',(-5.95549339426175,-3.21315848207099,
35.8546693769332));
#17657=CARTESIAN_POINT('Ctrl Pts',(-5.86717414355025,-3.37685557859871,
35.8634186779088));
#17658=CARTESIAN_POINT('Ctrl Pts',(-5.77210188986099,-3.53690907467538,
35.8721679788843));
#17659=CARTESIAN_POINT('Ctrl Pts',(-5.67059953466926,-3.69277536785123,
35.8809172798599));
#17660=CARTESIAN_POINT('Ctrl Pts',(-5.5690975576162,-3.84864108036004,35.8896665482407));
#17661=CARTESIAN_POINT('Ctrl Pts',(-5.46116568337921,-4.00031938104482,
35.8984158166214));
#17662=CARTESIAN_POINT('Ctrl Pts',(-5.34717048685964,-4.14729511663413,
35.9071650850022));
#17663=CARTESIAN_POINT('Ctrl Pts',(-5.23317570555359,-4.29427031688233,
35.9159143215148));
#17664=CARTESIAN_POINT('Ctrl Pts',(-5.11311782178639,-4.43654275987321,
35.9246635580274));
#17665=CARTESIAN_POINT('Ctrl Pts',(-4.9874045917184,-4.57362924147839,35.93341279454));
#17666=CARTESIAN_POINT('Ctrl Pts',(-4.86169180910634,-4.7107152351464,35.9421619999112));
#17667=CARTESIAN_POINT('Ctrl Pts',(-4.73032391415212,-4.84261509316739,
35.9509112052823));
#17668=CARTESIAN_POINT('Ctrl Pts',(-4.59374707237049,-4.9688808433175,35.9596604106534));
#17669=CARTESIAN_POINT('Ctrl Pts',(-4.45717070537167,-5.09514615452929,
35.9684095856097));
#17670=CARTESIAN_POINT('Ctrl Pts',(-4.31538563819284,-5.21577720253818,
35.9771587605659));
#17671=CARTESIAN_POINT('Ctrl Pts',(-4.16887341290435,-5.33036429028816,
35.9859079355221));
#17672=CARTESIAN_POINT('Ctrl Pts',(-4.02236168477091,-5.44495098921361,
35.99465708079));
#17673=CARTESIAN_POINT('Ctrl Pts',(-3.87112305634155,-5.55349359238958,
36.003406226058));
#17674=CARTESIAN_POINT('Ctrl Pts',(-3.7156711731641,-5.65562346102685,36.0121553713259));
#17675=CARTESIAN_POINT('Ctrl Pts',(-3.56021980456983,-5.75775299158965,
36.0209044876321));
#17676=CARTESIAN_POINT('Ctrl Pts',(-3.40055544862076,-5.85346967275534,
36.0296536039382));
#17677=CARTESIAN_POINT('Ctrl Pts',(-3.23722036323099,-5.94244842803727,
36.0384027202444));
#17678=CARTESIAN_POINT('Ctrl Pts',(-3.07388580495719,-6.03142689616643,
36.0471518083153));
#17679=CARTESIAN_POINT('Ctrl Pts',(-2.90688079257356,-6.1136673448499,36.0559008963863));
#17680=CARTESIAN_POINT('Ctrl Pts',(-2.7367725109424,-6.18889046787468,36.0646499844572));
#17681=CARTESIAN_POINT('Ctrl Pts',(-2.56666476416297,-6.26411335438412,
36.0733990450195));
#17682=CARTESIAN_POINT('Ctrl Pts',(-2.39345402971772,-6.33231884350411,
36.0821481055817));
#17683=CARTESIAN_POINT('Ctrl Pts',(-2.21772856473747,-6.39327529621144,
36.0908971661439));
#17684=CARTESIAN_POINT('Ctrl Pts',(-2.04200363767981,-6.45423156232173,
36.0996461999239));
#17685=CARTESIAN_POINT('Ctrl Pts',(-1.86376426619808,-6.50793874252137,
36.1083952337039));
#17686=CARTESIAN_POINT('Ctrl Pts',(-1.68361578194407,-6.55421443796195,
36.1171442674839));
#17687=CARTESIAN_POINT('Ctrl Pts',(-1.50346783419563,-6.6004899955875,36.1258932752081));
#17688=CARTESIAN_POINT('Ctrl Pts',(-1.32141106256918,-6.63933404145561,
36.1346422829324));
#17689=CARTESIAN_POINT('Ctrl Pts',(-1.13806375958692,-6.6706146552709,36.1433912906566));
#17690=CARTESIAN_POINT('Ctrl Pts',(-0.954716987415489,-6.70189517852533,
36.1521402730515));
#17691=CARTESIAN_POINT('Ctrl Pts',(-0.770079973806076,-6.72561226535872,
36.1608892554464));
#17692=CARTESIAN_POINT('Ctrl Pts',(-0.584779770548522,-6.74168536939816,
36.1696382378413));
#17693=CARTESIAN_POINT('Ctrl Pts',(-0.39149064755002,-6.75845143942416,
36.1787644185173));
#17694=CARTESIAN_POINT('Ctrl Pts',(-0.197480213100493,-6.76689975924038,
36.1878905991934));
#17695=CARTESIAN_POINT('Ctrl Pts',(-0.00346532629400725,-6.76699911271708,
36.1970167798694));
#17696=CARTESIAN_POINT('Ctrl Pts',(0.184486595299774,-6.76709536139763,
36.2058577673994));
#17697=CARTESIAN_POINT('Ctrl Pts',(0.372442378188871,-6.7593565972675,36.2146987549293));
#17698=CARTESIAN_POINT('Ctrl Pts',(0.559750217725649,-6.74380965728987,
36.2235397424592));
#17699=CARTESIAN_POINT('Ctrl Pts',(0.745129914461276,-6.72842275717214,
36.232289721057));
#17700=CARTESIAN_POINT('Ctrl Pts',(0.929874656317667,-6.70538772273424,
36.2410396996547));
#17701=CARTESIAN_POINT('Ctrl Pts',(1.11335688290121,-6.67478280180685,36.2497896782525));
#17702=CARTESIAN_POINT('Ctrl Pts',(1.29683723119207,-6.64417819417955,36.2585395672774));
#17703=CARTESIAN_POINT('Ctrl Pts',(1.47905480730593,-6.60600390229995,36.2672894563024));
#17704=CARTESIAN_POINT('Ctrl Pts',(1.65939064805172,-6.56038959797042,36.2760393453273));
#17705=CARTESIAN_POINT('Ctrl Pts',(1.83972470264625,-6.51477574543154,36.2847891476883));
#17706=CARTESIAN_POINT('Ctrl Pts',(2.01817678126204,-6.46172209819989,36.2935389500492));
#17707=CARTESIAN_POINT('Ctrl Pts',(2.19414072348031,-6.40140886723894,36.3022887524102));
#17708=CARTESIAN_POINT('Ctrl Pts',(2.3701029813244,-6.34109621361246,36.3110384710157));
#17709=CARTESIAN_POINT('Ctrl Pts',(2.54357687927248,-6.27352420825835,36.3197881896211));
#17710=CARTESIAN_POINT('Ctrl Pts',(2.71397317790297,-6.19892237325354,36.3285379082266));
#17711=CARTESIAN_POINT('Ctrl Pts',(2.88436790207525,-6.12432122756811,36.3372875459849));
#17712=CARTESIAN_POINT('Ctrl Pts',(3.05168482126578,-6.04269049717255,36.3460371837432));
#17713=CARTESIAN_POINT('Ctrl Pts',(3.21535561997707,-5.95430745234758,36.3547868215014));
#17714=CARTESIAN_POINT('Ctrl Pts',(3.37902496075585,-5.86592519481341,36.3635363813205));
#17715=CARTESIAN_POINT('Ctrl Pts',(3.53904799385165,-5.77079087940054,36.3722859411395));
#17716=CARTESIAN_POINT('Ctrl Pts',(3.6948811881526,-5.66922763746844,36.3810355009585));
#17717=CARTESIAN_POINT('Ctrl Pts',(3.85071304611103,-5.56766526648865,36.3897849857459));
#17718=CARTESIAN_POINT('Ctrl Pts',(4.00235489706232,-5.4596742358052,36.3985344705333));
#17719=CARTESIAN_POINT('Ctrl Pts',(4.14929168607912,-5.34562133936128,36.4072839553208));
#17720=CARTESIAN_POINT('Ctrl Pts',(4.29622726386008,-5.23156938308325,36.4160333679841));
#17721=CARTESIAN_POINT('Ctrl Pts',(4.4384576309231,-5.11145583676991,36.4247827806474));
#17722=CARTESIAN_POINT('Ctrl Pts',(4.57549970661197,-4.98568866203996,36.4335321933107));
#17723=CARTESIAN_POINT('Ctrl Pts',(4.71254069815517,-4.85992248225946,36.442281536757));
#17724=CARTESIAN_POINT('Ctrl Pts',(4.84439326931523,-4.72850295733787,36.4510308802033));
#17725=CARTESIAN_POINT('Ctrl Pts',(4.97060959434895,-4.59187644221468,36.4597802236496));
#17726=CARTESIAN_POINT('Ctrl Pts',(5.09682496280707,-4.45525096256444,36.4685295007859));
#17727=CARTESIAN_POINT('Ctrl Pts',(5.21740397616025,-4.31341878218101,36.4772787779222));
#17728=CARTESIAN_POINT('Ctrl Pts',(5.33193710452114,-4.16686161438447,36.4860280550585));
#17729=CARTESIAN_POINT('Ctrl Pts',(5.44646940289561,-4.02030550864273,36.4947772687915));
#17730=CARTESIAN_POINT('Ctrl Pts',(5.55495572749841,-3.86902470979881,36.5035264825245));
#17731=CARTESIAN_POINT('Ctrl Pts',(5.65702762491628,-3.71353301465519,36.5122756962574));
#17732=CARTESIAN_POINT('Ctrl Pts',(5.75909881655322,-3.5580423946662,36.5210248494935));
#17733=CARTESIAN_POINT('Ctrl Pts',(5.85475551250946,-3.39834117619271,36.5297740027297));
#17734=CARTESIAN_POINT('Ctrl Pts',(5.94367283728254,-3.23497174691677,36.5385231559658));
#17735=CARTESIAN_POINT('Ctrl Pts',(6.03258957676467,-3.0716033930066,36.5472722516113));
#17736=CARTESIAN_POINT('Ctrl Pts',(6.11476689685436,-2.90456712829185,36.5560213472569));
#17737=CARTESIAN_POINT('Ctrl Pts',(6.18992570525408,-2.73443024475572,36.5647704429024));
#17738=CARTESIAN_POINT('Ctrl Pts',(6.26508404388838,-2.56429442462687,36.5735194838634));
#17739=CARTESIAN_POINT('Ctrl Pts',(6.33322384283449,-2.39105828655639,36.5822685248245));
#17740=CARTESIAN_POINT('Ctrl Pts',(6.39411368720159,-2.21531017131718,36.5910175657855));
#17741=CARTESIAN_POINT('Ctrl Pts',(6.45500317121009,-2.0395630961914,36.5997665549679));
#17742=CARTESIAN_POINT('Ctrl Pts',(6.50864269270184,-1.86130434438246,36.6085155441503));
#17743=CARTESIAN_POINT('Ctrl Pts',(6.55485008446436,-1.68113930719546,36.6172645333327));
#17744=CARTESIAN_POINT('Ctrl Pts',(6.60199664749493,-1.49731239211445,36.6261913468621));
#17745=CARTESIAN_POINT('Ctrl Pts',(6.64140563640983,-1.31150116499281,36.6351181603915));
#17746=CARTESIAN_POINT('Ctrl Pts',(6.67293772282237,-1.12436255155276,36.6440449739208));
#17747=CARTESIAN_POINT('Ctrl Pts',(6.70384494949925,-0.940932395047478,
36.6527948880764));
#17748=CARTESIAN_POINT('Ctrl Pts',(6.72718449348974,-0.756227260502834,
36.6615448022319));
#17749=CARTESIAN_POINT('Ctrl Pts',(6.74287707373965,-0.570874564537798,
36.6702947163874));
#17750=CARTESIAN_POINT('Ctrl Pts',(6.75856934538692,-0.385525513628589,
36.6790444584714));
#17751=CARTESIAN_POINT('Ctrl Pts',(6.76661493004114,-0.199529212414354,
36.6877942005554));
#17752=CARTESIAN_POINT('Ctrl Pts',(6.76698649908907,-0.013517438596568,
36.6965439426393));
#17753=CARTESIAN_POINT('Ctrl Pts',(6.76735806132379,0.17249092444962,36.7052935242852));
#17754=CARTESIAN_POINT('Ctrl Pts',(6.76005588896269,0.358514472905227,36.7140431059311));
#17755=CARTESIAN_POINT('Ctrl Pts',(6.74510478454554,0.543921359666006,36.722792687577));
#17756=CARTESIAN_POINT('Ctrl Pts',(6.73015393440646,0.729325093154255,36.7315421204161));
#17757=CARTESIAN_POINT('Ctrl Pts',(6.70755443556845,0.914111900260174,36.7402915532551));
#17758=CARTESIAN_POINT('Ctrl Pts',(6.67738304682256,1.09765415591921,36.7490409860942));
#17759=CARTESIAN_POINT('Ctrl Pts',(6.64721213111786,1.28119353391662,36.7577902817555));
#17760=CARTESIAN_POINT('Ctrl Pts',(6.60946960955407,1.46348811673048,36.7665395774168));
#17761=CARTESIAN_POINT('Ctrl Pts',(6.56428366991083,1.64391876348622,36.7752888730781));
#17762=CARTESIAN_POINT('Ctrl Pts',(6.51909837867606,1.82434682110113,36.784038043189));
#17763=CARTESIAN_POINT('Ctrl Pts',(6.46646995271799,2.0029107182084,36.7927872132998));
#17764=CARTESIAN_POINT('Ctrl Pts',(6.40657713281416,2.17900400213096,36.8015363834106));
#17765=CARTESIAN_POINT('Ctrl Pts',(6.34668509278916,2.35509499310046,36.8102854395964));
#17766=CARTESIAN_POINT('Ctrl Pts',(6.27952894037372,2.52871516398505,36.8190344957822));
#17767=CARTESIAN_POINT('Ctrl Pts',(6.20533675061283,2.69927486771797,36.827783551968));
#17768=CARTESIAN_POINT('Ctrl Pts',(6.1283211790775,2.87632521636277,36.8368655532502));
#17769=CARTESIAN_POINT('Ctrl Pts',(6.04372366625912,3.05007728920327,36.8459475545325));
#17770=CARTESIAN_POINT('Ctrl Pts',(5.95185378007702,3.21989527478502,36.8550295558147));
#17771=CARTESIAN_POINT('Ctrl Pts',(5.86334450817198,3.38350129287052,36.8637793361219));
#17772=CARTESIAN_POINT('Ctrl Pts',(5.76808562057075,3.54345567125256,36.872529116429));
#17773=CARTESIAN_POINT('Ctrl Pts',(5.66640068804296,3.69921508465597,36.8812788967361));
#17774=CARTESIAN_POINT('Ctrl Pts',(5.56471941107727,3.85496889852566,36.8900283624896));
#17775=CARTESIAN_POINT('Ctrl Pts',(5.4566127081491,4.00652780919914,36.8987778282431));
#17776=CARTESIAN_POINT('Ctrl Pts',(5.34244776448903,4.153377045695,36.9075272939966));
#17777=CARTESIAN_POINT('Ctrl Pts',(5.22828631819376,4.30022178356516,36.9162764917161));
#17778=CARTESIAN_POINT('Ctrl Pts',(5.10806717843841,4.44235690972941,36.9250256894357));
#17779=CARTESIAN_POINT('Ctrl Pts',(4.98219864544483,4.57929969070902,36.9337748871553));
#17780=CARTESIAN_POINT('Ctrl Pts',(4.85633329943774,4.71623900430259,36.9425238633456));
#17781=CARTESIAN_POINT('Ctrl Pts',(4.72481904033382,4.84798602483876,36.9512728395358));
#17782=CARTESIAN_POINT('Ctrl Pts',(4.58810250736918,4.97409332259385,36.9600218157261));
#17783=CARTESIAN_POINT('Ctrl Pts',(4.45137708685356,5.10020881822385,36.9687713606622));
#17784=CARTESIAN_POINT('Ctrl Pts',(4.3094489263576,5.22068366308174,36.9775209055984));
#17785=CARTESIAN_POINT('Ctrl Pts',(4.16280009466365,5.33510865605081,36.9862704505346));
#17786=CARTESIAN_POINT('Ctrl Pts',(4.01615988348486,5.44952692273115,36.9950194811429));
#17787=CARTESIAN_POINT('Ctrl Pts',(3.86479978231921,5.55789587288842,37.0037685117512));
#17788=CARTESIAN_POINT('Ctrl Pts',(3.70923383580751,5.65984746714085,37.0125175423594));
#17789=CARTESIAN_POINT('Ctrl Pts',(3.55366577799218,5.76180044505581,37.0212666917075));
#17790=CARTESIAN_POINT('Ctrl Pts',(3.39389200026513,5.85733573571249,37.0300158410555));
#17791=CARTESIAN_POINT('Ctrl Pts',(3.23045513625709,5.94612887622108,37.0387649904035));
#17792=CARTESIAN_POINT('Ctrl Pts',(3.18695122151355,5.96976399206807,37.0410938545164));
#17793=CARTESIAN_POINT('Ctrl Pts',(3.1431879126255,5.99292165435392,37.0434227186293));
#17794=CARTESIAN_POINT('Ctrl Pts',(3.09917575053255,6.01559628526641,37.0457515827422));
#17795=CARTESIAN_POINT('Ctrl Pts',(3.09917575053259,6.01559628526639,35.0459310802154));
#17796=CARTESIAN_POINT('Ctrl Pts',(2.9440586973841,6.09551105793644,35.0541366393698));
#17797=CARTESIAN_POINT('Ctrl Pts',(2.78573265664416,6.16948200765193,35.0623421985241));
#17798=CARTESIAN_POINT('Ctrl Pts',(2.6246942276003,6.23724852892697,35.0705477576784));
#17799=CARTESIAN_POINT('Ctrl Pts',(2.46374070143196,6.30497932225462,35.0787489906879));
#17800=CARTESIAN_POINT('Ctrl Pts',(2.30007796525645,6.36651206492384,35.0869502236974));
#17801=CARTESIAN_POINT('Ctrl Pts',(2.13422506491495,6.4216331546024,35.0951514567069));
#17802=CARTESIAN_POINT('Ctrl Pts',(1.96189659516602,6.47890639501991,35.1036728990915));
#17803=CARTESIAN_POINT('Ctrl Pts',(1.78720384805667,6.52925703590783,35.1121943414761));
#17804=CARTESIAN_POINT('Ctrl Pts',(1.6107499787808,6.57250131273153,35.1207157838607));
#17805=CARTESIAN_POINT('Ctrl Pts',(1.44096982551859,6.61411003447263,35.1289149341543));
#17806=CARTESIAN_POINT('Ctrl Pts',(1.26955970154868,6.64914001105007,35.1371140844478));
#17807=CARTESIAN_POINT('Ctrl Pts',(1.09707021372699,6.6774790112851,35.1453132347414));
#17808=CARTESIAN_POINT('Ctrl Pts',(0.924561343545949,6.70582119592686,35.1535133063599));
#17809=CARTESIAN_POINT('Ctrl Pts',(0.750973221621192,6.72747084782639,35.1617133779785));
#17810=CARTESIAN_POINT('Ctrl Pts',(0.576864392437851,6.74236727512951,35.1699134495971));
#17811=CARTESIAN_POINT('Ctrl Pts',(0.402704413692092,6.75726807869397,35.1781159302266));
#17812=CARTESIAN_POINT('Ctrl Pts',(0.228023780045558,6.76541167489834,35.1863184108561));
#17813=CARTESIAN_POINT('Ctrl Pts',(0.0533839308849914,6.76678942748504,
35.1945208914856));
#17814=CARTESIAN_POINT('Ctrl Pts',(-0.121338906013691,6.76816783477094,
35.2027272698814));
#17815=CARTESIAN_POINT('Ctrl Pts',(-0.296020561820025,6.7627739909933,35.2109336482771));
#17816=CARTESIAN_POINT('Ctrl Pts',(-0.470101770653946,6.75065132600018,
35.2191400266729));
#17817=CARTESIAN_POINT('Ctrl Pts',(-0.644388886027253,6.73851432209012,
35.227356111728));
#17818=CARTESIAN_POINT('Ctrl Pts',(-0.81807377860967,6.7196326277004,35.235572196783));
#17819=CARTESIAN_POINT('Ctrl Pts',(-0.990603530442371,6.69410140687121,
35.243788281838));
#17820=CARTESIAN_POINT('Ctrl Pts',(-1.16325377716496,6.66855235502094,35.2520101050122));
#17821=CARTESIAN_POINT('Ctrl Pts',(-1.33474692428573,6.63634458684152,35.2602319281863));
#17822=CARTESIAN_POINT('Ctrl Pts',(-1.50454249032188,6.59762388249103,35.2684537513604));
#17823=CARTESIAN_POINT('Ctrl Pts',(-1.6745716687148,6.55884990445849,35.2766868864877));
#17824=CARTESIAN_POINT('Ctrl Pts',(-1.8428982578737,6.51354519028979,35.284920021615));
#17825=CARTESIAN_POINT('Ctrl Pts',(-2.00899827364353,6.46190489998865,35.2931531567423));
#17826=CARTESIAN_POINT('Ctrl Pts',(-2.05279672271923,6.44828801612187,35.2953241291407));
#17827=CARTESIAN_POINT('Ctrl Pts',(-2.09644047195137,6.43423086992658,35.297495101539));
#17828=CARTESIAN_POINT('Ctrl Pts',(-2.139920175324,6.41973758367438,35.2996660739374));
#17829=CARTESIAN_POINT('Ctrl Pts',(-2.30322433018449,6.3653026708535,35.3078199661041));
#17830=CARTESIAN_POINT('Ctrl Pts',(-2.46471757423055,6.30454336770894,35.3159738582709));
#17831=CARTESIAN_POINT('Ctrl Pts',(-2.623868021179,6.23759614013558,35.3241277504376));
#17832=CARTESIAN_POINT('Ctrl Pts',(-2.78282426011805,6.17073060688385,35.3322716925778));
#17833=CARTESIAN_POINT('Ctrl Pts',(-2.93944305928883,6.09769231987377,35.340415634718));
#17834=CARTESIAN_POINT('Ctrl Pts',(-3.09320666017572,6.01866775602746,35.3485595768583));
#17835=CARTESIAN_POINT('Ctrl Pts',(-3.24681499068139,5.93972299113281,35.3566952952512));
#17836=CARTESIAN_POINT('Ctrl Pts',(-3.39757353997227,5.85480414956821,35.3648310136441));
#17837=CARTESIAN_POINT('Ctrl Pts',(-3.54498355517324,5.7641461287472,35.372966732037));
#17838=CARTESIAN_POINT('Ctrl Pts',(-3.69227572357141,5.67356058439862,35.3810959463372));
#17839=CARTESIAN_POINT('Ctrl Pts',(-3.83622437802582,5.57724518699878,35.3892251606374));
#17840=CARTESIAN_POINT('Ctrl Pts',(-3.97635446585219,5.47548118085501,35.3973543749376));
#17841=CARTESIAN_POINT('Ctrl Pts',(-4.11640199089731,5.37377713270818,35.405478799613));
#17842=CARTESIAN_POINT('Ctrl Pts',(-4.25263513467597,5.26663108321617,35.4136032242885));
#17843=CARTESIAN_POINT('Ctrl Pts',(-4.38460700780134,5.15436808805303,35.4217276489639));
#17844=CARTESIAN_POINT('Ctrl Pts',(-4.51738003468018,5.04142358464255,35.4299013940981));
#17845=CARTESIAN_POINT('Ctrl Pts',(-4.64583956460938,4.92330000262571,35.4380751392323));
#17846=CARTESIAN_POINT('Ctrl Pts',(-4.76956309492173,4.80037049440569,35.4462488843664));
#17847=CARTESIAN_POINT('Ctrl Pts',(-4.89249433595027,4.67822819078433,35.4543702872286));
#17848=CARTESIAN_POINT('Ctrl Pts',(-5.01074980957345,4.55134160982569,35.4624916900908));
#17849=CARTESIAN_POINT('Ctrl Pts',(-5.12395124004177,4.42011455617096,35.4706130929529));
#17850=CARTESIAN_POINT('Ctrl Pts',(-5.23716142264873,4.28887735673132,35.4787351237192));
#17851=CARTESIAN_POINT('Ctrl Pts',(-5.34531654466242,4.15329929324313,35.4868571544854));
#17852=CARTESIAN_POINT('Ctrl Pts',(-5.44807806829093,4.013817928333,35.4949791852517));
#17853=CARTESIAN_POINT('Ctrl Pts',(-5.55086710506615,3.87429921898576,35.5031033905928));
#17854=CARTESIAN_POINT('Ctrl Pts',(-5.64825945106151,3.73087542184351,35.511227595934));
#17855=CARTESIAN_POINT('Ctrl Pts',(-5.73995944602269,3.58401374969668,35.5193518012751));
#17856=CARTESIAN_POINT('Ctrl Pts',(-5.83265202997786,3.43556240156926,35.5275639455175));
#17857=CARTESIAN_POINT('Ctrl Pts',(-5.91952810752149,3.28359864338214,35.5357760897599));
#17858=CARTESIAN_POINT('Ctrl Pts',(-6.0003299993453,3.12863051493092,35.5439882340023));
#17859=CARTESIAN_POINT('Ctrl Pts',(-6.08039425895217,2.97507707469507,35.5521254104188));
#17860=CARTESIAN_POINT('Ctrl Pts',(-6.15449467311389,2.81857424654053,35.5602625868353));
#17861=CARTESIAN_POINT('Ctrl Pts',(-6.22242921177155,2.65963600977505,35.5683997632517));
#17862=CARTESIAN_POINT('Ctrl Pts',(-6.29130257203203,2.4985013254714,35.5766493914071));
#17863=CARTESIAN_POINT('Ctrl Pts',(-6.35383825003811,2.33486379393832,35.5848990195625));
#17864=CARTESIAN_POINT('Ctrl Pts',(-6.40987824321453,2.16927405072873,35.5931486477179));
#17865=CARTESIAN_POINT('Ctrl Pts',(-6.46591823639095,2.00368430751914,35.6013982758733));
#17866=CARTESIAN_POINT('Ctrl Pts',(-6.51546249628877,1.836142739554,35.6096479040287));
#17867=CARTESIAN_POINT('Ctrl Pts',(-6.5584069576644,1.66720939826383,35.6178975321841));
#17868=CARTESIAN_POINT('Ctrl Pts',(-6.61564801371588,1.44203663912329,35.6288935352197));
#17869=CARTESIAN_POINT('Ctrl Pts',(-6.66130674986052,1.21384317140458,35.6398895382552));
#17870=CARTESIAN_POINT('Ctrl Pts',(-6.69512707799532,0.983647502662358,
35.6508855412908));
#17871=CARTESIAN_POINT('Ctrl Pts',(-6.72814535798224,0.758910917848252,
35.661620774418));
#17872=CARTESIAN_POINT('Ctrl Pts',(-6.74988016006797,0.532265633934366,
35.6723560075452));
#17873=CARTESIAN_POINT('Ctrl Pts',(-6.76013745111812,0.304681213713947,
35.6830912406724));
#17874=CARTESIAN_POINT('Ctrl Pts',(-6.7646245540288,0.205123278835854,35.6877874217182));
#17875=CARTESIAN_POINT('Ctrl Pts',(-6.76691581385178,0.105385939787265,
35.6924836027641));
#17876=CARTESIAN_POINT('Ctrl Pts',(-6.76699772244824,0.00555197085342392,
35.69717978381));
#17877=CARTESIAN_POINT('',(-6.76699973985247,0.00187638925443544,35.3028202162328));
#17878=CARTESIAN_POINT('Ctrl Pts',(3.09917575053259,6.01559628526639,34.6514942595564));
#17879=CARTESIAN_POINT('Ctrl Pts',(2.94591905660335,6.0945526192537,34.6596423743809));
#17880=CARTESIAN_POINT('Ctrl Pts',(2.78942067268773,6.1677630348461,34.6677904892054));
#17881=CARTESIAN_POINT('Ctrl Pts',(2.63015446617675,6.23494799369253,34.6759386040299));
#17882=CARTESIAN_POINT('Ctrl Pts',(2.47105778204377,6.30206144111015,34.6840780460302));
#17883=CARTESIAN_POINT('Ctrl Pts',(2.30919947399828,6.36316205833891,34.6922174880306));
#17884=CARTESIAN_POINT('Ctrl Pts',(2.14507860761712,6.41801579673527,34.7003569300309));
#17885=CARTESIAN_POINT('Ctrl Pts',(1.98109793576011,6.47282267823937,34.7084894191969));
#17886=CARTESIAN_POINT('Ctrl Pts',(1.81485889836932,6.52139319002899,34.7166219083629));
#17887=CARTESIAN_POINT('Ctrl Pts',(1.64688117360616,6.56354107170981,34.7247543975289));
#17888=CARTESIAN_POINT('Ctrl Pts',(1.47901164815922,6.60566180471968,34.7328816483232));
#17889=CARTESIAN_POINT('Ctrl Pts',(1.30940601892574,6.64136805707052,34.7410088991174));
#17890=CARTESIAN_POINT('Ctrl Pts',(1.13859978220374,6.67052318307684,34.7491361499117));
#17891=CARTESIAN_POINT('Ctrl Pts',(0.967867693566158,6.69966565265571,34.7572598726141));
#17892=CARTESIAN_POINT('Ctrl Pts',(0.795936395311186,6.72226259879266,34.7653835953166));
#17893=CARTESIAN_POINT('Ctrl Pts',(0.623352247553659,6.73822832616036,34.7735073180191));
#17894=CARTESIAN_POINT('Ctrl Pts',(0.450776092652785,6.75419331411038,34.7816306644892));
#17895=CARTESIAN_POINT('Ctrl Pts',(0.27754751151336,6.76352765156302,34.7897540109592));
#17896=CARTESIAN_POINT('Ctrl Pts',(0.10421895937072,6.76619741128706,34.7978773574293));
#17897=CARTESIAN_POINT('Ctrl Pts',(-0.0691143255496477,6.76886724390953,
34.8060009257093));
#17898=CARTESIAN_POINT('Ctrl Pts',(-0.242547221102038,6.76487212990511,
34.8141244939893));
#17899=CARTESIAN_POINT('Ctrl Pts',(-0.415526524812408,6.75423028236211,
34.8222480622693));
#17900=CARTESIAN_POINT('Ctrl Pts',(-0.588543460688567,6.74358611965329,
34.8303733978559));
#17901=CARTESIAN_POINT('Ctrl Pts',(-0.761106243098924,6.7262923662018,34.8384987334425));
#17902=CARTESIAN_POINT('Ctrl Pts',(-0.932666087647813,6.70241918779718,
34.8466240690291));
#17903=CARTESIAN_POINT('Ctrl Pts',(-1.10429589693067,6.67853627354451,34.8547527182521));
#17904=CARTESIAN_POINT('Ctrl Pts',(-1.27492159193006,6.6480686416746,34.8628813674751));
#17905=CARTESIAN_POINT('Ctrl Pts',(-1.44400392512547,6.61113769817437,34.871010016698));
#17906=CARTESIAN_POINT('Ctrl Pts',(-1.61328476000066,6.57416339796038,34.8791482089081));
#17907=CARTESIAN_POINT('Ctrl Pts',(-1.7810182570976,6.53071071045453,34.8872864011182));
#17908=CARTESIAN_POINT('Ctrl Pts',(-1.94667882281563,6.48095136232337,34.8954245933283));
#17909=CARTESIAN_POINT('Ctrl Pts',(-2.11244759646717,6.43115951185099,34.9035681013295));
#17910=CARTESIAN_POINT('Ctrl Pts',(-2.27614039622114,6.37505291156961,34.9117116093307));
#17911=CARTESIAN_POINT('Ctrl Pts',(-2.43725129985825,6.31285158239439,34.9198551173319));
#17912=CARTESIAN_POINT('Ctrl Pts',(-2.59860229952536,6.25055755749305,34.9280107612215));
#17913=CARTESIAN_POINT('Ctrl Pts',(-2.75736338394079,6.18215080816633,34.9361664051111));
#17914=CARTESIAN_POINT('Ctrl Pts',(-2.91305202609664,6.10789791116831,34.9443220490006));
#17915=CARTESIAN_POINT('Ctrl Pts',(-3.00228537832362,6.06533966915433,34.9489964776151));
#17916=CARTESIAN_POINT('Ctrl Pts',(-3.09050991945001,6.02086176861545,34.9536709062295));
#17917=CARTESIAN_POINT('Ctrl Pts',(-3.17763918594097,5.97452075098685,34.9583453348439));
#17918=CARTESIAN_POINT('Ctrl Pts',(-3.33109957183084,5.89290052469292,34.9665783849759));
#17919=CARTESIAN_POINT('Ctrl Pts',(-3.4816375613256,5.80524455240668,34.974811435108));
#17920=CARTESIAN_POINT('Ctrl Pts',(-3.62874575691539,5.71178546793108,34.98304448524));
#17921=CARTESIAN_POINT('Ctrl Pts',(-3.77567876925723,5.61843767885884,34.9912677310748));
#17922=CARTESIAN_POINT('Ctrl Pts',(-3.91918982129634,5.51930072852775,34.9994909769097));
#17923=CARTESIAN_POINT('Ctrl Pts',(-4.05879438461281,5.41465392646987,35.0077142227446));
#17924=CARTESIAN_POINT('Ctrl Pts',(-4.1982606425083,5.3101107973842,35.0159293218581));
#17925=CARTESIAN_POINT('Ctrl Pts',(-4.33382783447221,5.20006890075457,35.0241444209716));
#17926=CARTESIAN_POINT('Ctrl Pts',(-4.46503872804362,5.08485183236155,35.0323595200851));
#17927=CARTESIAN_POINT('Ctrl Pts',(-4.59614588440986,4.96972585622724,35.040568124224));
#17928=CARTESIAN_POINT('Ctrl Pts',(-4.72290333451079,4.84943309318149,35.0487767283629));
#17929=CARTESIAN_POINT('Ctrl Pts',(-4.84488531226018,4.72433861096403,35.0569853325018));
#17930=CARTESIAN_POINT('Ctrl Pts',(-4.96679524911309,4.59931800784586,35.0651890887508));
#17931=CARTESIAN_POINT('Ctrl Pts',(-5.08393508270115,4.46950159067045,35.0733928449997));
#17932=CARTESIAN_POINT('Ctrl Pts',(-5.19591438652508,4.33529268768578,35.0815966012487));
#17933=CARTESIAN_POINT('Ctrl Pts',(-5.3078605584955,4.20112349373268,35.089797930213));
#17934=CARTESIAN_POINT('Ctrl Pts',(-5.41464901003014,4.06256467497881,35.0979992591773));
#17935=CARTESIAN_POINT('Ctrl Pts',(-5.51592809443204,3.92005436914532,35.1062005881416));
#17936=CARTESIAN_POINT('Ctrl Pts',(-5.61719321148133,3.7775637168435,35.1144007860643));
#17937=CARTESIAN_POINT('Ctrl Pts',(-5.71295026651222,3.63112295428702,35.122600983987));
#17938=CARTESIAN_POINT('Ctrl Pts',(-5.80288962786727,3.48120108106247,35.1308011819097));
#17939=CARTESIAN_POINT('Ctrl Pts',(-5.89283288456784,3.33127271460192,35.1390017349896));
#17940=CARTESIAN_POINT('Ctrl Pts',(-5.97695776123205,3.17786324432855,35.1472022880694));
#17941=CARTESIAN_POINT('Ctrl Pts',(-6.05499944232427,3.02146831084704,35.1554028411492));
#17942=CARTESIAN_POINT('Ctrl Pts',(-6.13305864614557,2.86503826195012,35.1636052355025));
#17943=CARTESIAN_POINT('Ctrl Pts',(-6.20503177404148,2.70562173526347,35.1718076298557));
#17944=CARTESIAN_POINT('Ctrl Pts',(-6.27070119280544,2.54373653324168,35.1800100242089));
#17945=CARTESIAN_POINT('Ctrl Pts',(-6.33643202401997,2.38169994009822,35.1882200892427));
#17946=CARTESIAN_POINT('Ctrl Pts',(-6.39584723337748,2.21719039157581,35.1964301542766));
#17947=CARTESIAN_POINT('Ctrl Pts',(-6.44877802302472,2.05074401370658,35.2046402193104));
#17948=CARTESIAN_POINT('Ctrl Pts',(-6.50173414440882,1.88421797755389,35.2128542135357));
#17949=CARTESIAN_POINT('Ctrl Pts',(-6.54819956334234,1.71575360909952,35.221068207761));
#17950=CARTESIAN_POINT('Ctrl Pts',(-6.58805614454478,1.54589949101675,35.2292822019863));
#17951=CARTESIAN_POINT('Ctrl Pts',(-6.62796706354206,1.37581380519926,35.2375073946215));
#17952=CARTESIAN_POINT('Ctrl Pts',(-6.66125106982199,1.20433493500494,35.2457325872567));
#17953=CARTESIAN_POINT('Ctrl Pts',(-6.68784146855085,1.03202010229044,35.2539577798919));
#17954=CARTESIAN_POINT('Ctrl Pts',(-6.7117541571757,0.877057742298748,35.2613546780118));
#17955=CARTESIAN_POINT('Ctrl Pts',(-6.73025415764975,0.721419572584288,
35.2687515761317));
#17956=CARTESIAN_POINT('Ctrl Pts',(-6.74332896696352,0.565511665052691,
35.2761484742516));
#17957=CARTESIAN_POINT('Ctrl Pts',(-6.75904402005099,0.378120707003798,
35.2850390548977));
#17958=CARTESIAN_POINT('Ctrl Pts',(-6.76694755464435,0.190076741669039,
35.2939296355438));
#17959=CARTESIAN_POINT('Ctrl Pts',(-6.76699973985222,0.00187639016204831,
35.3028202161899));
#17960=CARTESIAN_POINT('Ctrl Pts',(-6.76699973985247,0.00187638925439036,
35.3028202162328));
#17961=CARTESIAN_POINT('Ctrl Pts',(-6.76704855127815,-0.17415686403976,
35.3111360234152));
#17962=CARTESIAN_POINT('Ctrl Pts',(-6.76022425514039,-0.350411533394409,
35.3194518305977));
#17963=CARTESIAN_POINT('Ctrl Pts',(-6.74650123491233,-0.526317477694271,
35.3277676377801));
#17964=CARTESIAN_POINT('Ctrl Pts',(-6.73279357865191,-0.702026481875204,
35.3360741347822));
#17965=CARTESIAN_POINT('Ctrl Pts',(-6.71220261027407,-0.877387194927201,
35.3443806317844));
#17966=CARTESIAN_POINT('Ctrl Pts',(-6.6847547233564,-1.05182854523171,35.3526871287865));
#17967=CARTESIAN_POINT('Ctrl Pts',(-6.65733965931409,-1.22606129417046,
35.3609836926701));
#17968=CARTESIAN_POINT('Ctrl Pts',(-6.62308407785982,-1.39937653084823,
35.3692802565536));
#17969=CARTESIAN_POINT('Ctrl Pts',(-6.5820662189394,-1.57120758956186,35.3775768204372));
#17970=CARTESIAN_POINT('Ctrl Pts',(-6.54107691905235,-1.74291900943844,
35.3858676077675));
#17971=CARTESIAN_POINT('Ctrl Pts',(-6.49333479971102,-1.91314797307148,
35.3941583950978));
#17972=CARTESIAN_POINT('Ctrl Pts',(-6.43896942157368,-2.08133653887091,
35.4024491824282));
#17973=CARTESIAN_POINT('Ctrl Pts',(-6.38463862630875,-2.24941811665863,
35.4107346958278));
#17974=CARTESIAN_POINT('Ctrl Pts',(-6.3236930770421,-2.41546155410251,35.4190202092273));
#17975=CARTESIAN_POINT('Ctrl Pts',(-6.25631258088812,-2.57892262199181,
35.4273057226269));
#17976=CARTESIAN_POINT('Ctrl Pts',(-6.23531946562246,-2.62985066846694,
35.4298871630698));
#17977=CARTESIAN_POINT('Ctrl Pts',(-6.21370207339749,-2.68052815658692,
35.4324686035126));
#17978=CARTESIAN_POINT('Ctrl Pts',(-6.19146682236525,-2.73093895712636,
35.4350500439555));
#17979=CARTESIAN_POINT('Ctrl Pts',(-6.11742721885216,-2.89879834757379,
35.4436458015031));
#17980=CARTESIAN_POINT('Ctrl Pts',(-6.03660075632427,-3.06354650195075,
35.4522415590507));
#17981=CARTESIAN_POINT('Ctrl Pts',(-5.94928238480897,-3.2246438727093,35.4608373165982));
#17982=CARTESIAN_POINT('Ctrl Pts',(-5.86188254228419,-3.38589155279215,
35.4694410942799));
#17983=CARTESIAN_POINT('Ctrl Pts',(-5.76797884592166,-3.54348138173558,
35.4780448719615));
#17984=CARTESIAN_POINT('Ctrl Pts',(-5.66791063371377,-3.69690114125796,
35.4866486496431));
#17985=CARTESIAN_POINT('Ctrl Pts',(-5.56390965326238,-3.85635043148607,
35.4955905633111));
#17986=CARTESIAN_POINT('Ctrl Pts',(-5.45325003331208,-4.01129494083088,
35.5045324769791));
#17987=CARTESIAN_POINT('Ctrl Pts',(-5.33635924956896,-4.161196818169,35.5134743906471));
#17988=CARTESIAN_POINT('Ctrl Pts',(-5.2235824459241,-4.30582288743815,35.5221015929778));
#17989=CARTESIAN_POINT('Ctrl Pts',(-5.10500584471209,-4.44575503210426,
35.5307287953086));
#17990=CARTESIAN_POINT('Ctrl Pts',(-4.98105186195777,-4.58054705777455,
35.5393559976393));
#17991=CARTESIAN_POINT('Ctrl Pts',(-4.85697983200792,-4.71546745221731,
35.5479914160597));
#17992=CARTESIAN_POINT('Ctrl Pts',(-4.72752041134947,-4.84523773852067,
35.5566268344801));
#17993=CARTESIAN_POINT('Ctrl Pts',(-4.59313160217126,-4.96944977690043,
35.5652622529005));
#17994=CARTESIAN_POINT('Ctrl Pts',(-4.4585442526691,-5.0938453208748,35.5739104289216));
#17995=CARTESIAN_POINT('Ctrl Pts',(-4.31901319114098,-5.21266600657686,
35.5825586049427));
#17996=CARTESIAN_POINT('Ctrl Pts',(-4.17502923641397,-5.32554409192982,
35.5912067809639));
#17997=CARTESIAN_POINT('Ctrl Pts',(-4.15979627994705,-5.33748616536092,
35.5921217251957));
#17998=CARTESIAN_POINT('Ctrl Pts',(-4.14451350921705,-5.34936176450257,
35.5930366694274));
#17999=CARTESIAN_POINT('Ctrl Pts',(-4.12918152370299,-5.36117048267539,
35.5939516136592));
#18000=CARTESIAN_POINT('Ctrl Pts',(-3.99133618395422,-5.46733916950572,
35.6021776062006));
#18001=CARTESIAN_POINT('Ctrl Pts',(-3.84921261207773,-5.56832741115146,
35.6104035987419));
#18002=CARTESIAN_POINT('Ctrl Pts',(-3.70323664277618,-5.66377324471944,
35.6186295912833));
#18003=CARTESIAN_POINT('Ctrl Pts',(-3.55741371041034,-5.75911901566777,
35.6268469599347));
#18004=CARTESIAN_POINT('Ctrl Pts',(-3.40774672066166,-5.8489337549284,35.6350643285861));
#18005=CARTESIAN_POINT('Ctrl Pts',(-3.25469406681355,-5.93289604927043,
35.6432816972375));
#18006=CARTESIAN_POINT('Ctrl Pts',(-3.10177124371692,-6.0167871204909,35.6514920952999));
#18007=CARTESIAN_POINT('Ctrl Pts',(-2.94546878880561,-6.09483546287145,
35.6597024933623));
#18008=CARTESIAN_POINT('Ctrl Pts',(-2.78627360760646,-6.16676320151469,
35.6679128914247));
#18009=CARTESIAN_POINT('Ctrl Pts',(-2.62718162241656,-6.23864431402562,
35.6761179672135));
#18010=CARTESIAN_POINT('Ctrl Pts',(-2.46520097147916,-6.30441257896438,
35.6843230430023));
#18011=CARTESIAN_POINT('Ctrl Pts',(-2.30084275109753,-6.36383623569321,
35.692528118791));
#18012=CARTESIAN_POINT('Ctrl Pts',(-2.13655820216616,-6.42323325653514,
35.7007295167605));
#18013=CARTESIAN_POINT('Ctrl Pts',(-1.96989854324486,-6.47629121346023,
35.70893091473));
#18014=CARTESIAN_POINT('Ctrl Pts',(-1.80139450711859,-6.52282659816455,
35.7171323126995));
#18015=CARTESIAN_POINT('Ctrl Pts',(-1.63290366963153,-6.56935833783006,
35.7253330682672));
#18016=CARTESIAN_POINT('Ctrl Pts',(-1.46256908546389,-6.6093684192243,35.7335338238349));
#18017=CARTESIAN_POINT('Ctrl Pts',(-1.29093666061151,-6.64272320199248,
35.7417345794026));
#18018=CARTESIAN_POINT('Ctrl Pts',(-1.1193051075701,-6.67607781533425,35.7499352933144));
#18019=CARTESIAN_POINT('Ctrl Pts',(-0.946376078563808,-6.70277712797335,
35.7581360072262));
#18020=CARTESIAN_POINT('Ctrl Pts',(-0.772705567099336,-6.72273866118368,
35.766336721138));
#18021=CARTESIAN_POINT('Ctrl Pts',(-0.599004464377042,-6.74270371052581,
35.7745388795676));
#18022=CARTESIAN_POINT('Ctrl Pts',(-0.424561975015007,-6.75592857496403,
35.7827410379972));
#18023=CARTESIAN_POINT('Ctrl Pts',(-0.249939166465919,-6.76238267277639,
35.7909431964268));
#18024=CARTESIAN_POINT('Ctrl Pts',(-0.0752539525814367,-6.76883907710381,
35.7991482860798));
#18025=CARTESIAN_POINT('Ctrl Pts',(0.0996113509594036,-6.76851988142677,
35.8073533757327));
#18026=CARTESIAN_POINT('Ctrl Pts',(0.274095664471448,-6.76144663269022,
35.8155584653856));
#18027=CARTESIAN_POINT('Ctrl Pts',(0.448779305682482,-6.75436530360326,
35.8237729283834));
#18028=CARTESIAN_POINT('Ctrl Pts',(0.623080728898286,-6.7405145213614,35.8319873913812));
#18029=CARTESIAN_POINT('Ctrl Pts',(0.796442896387099,-6.71996783569643,
35.840201854379));
#18030=CARTESIAN_POINT('Ctrl Pts',(0.969907775480884,-6.6994089767696,35.8484211841865));
#18031=CARTESIAN_POINT('Ctrl Pts',(1.14243193618498,-6.6721463622853,35.856640513994));
#18032=CARTESIAN_POINT('Ctrl Pts',(1.3134686276419,-6.63830469052156,35.8648598438014));
#18033=CARTESIAN_POINT('Ctrl Pts',(1.48477033008232,-6.60441058313923,35.8730919089621));
#18034=CARTESIAN_POINT('Ctrl Pts',(1.65457960914523,-6.56391713025827,35.8813239741228));
#18035=CARTESIAN_POINT('Ctrl Pts',(1.82236367117798,-6.5169992826431,35.8895560392835));
#18036=CARTESIAN_POINT('Ctrl Pts',(1.9731800336904,-6.4748261523201,35.8969556105447));
#18037=CARTESIAN_POINT('Ctrl Pts',(2.12236013454246,-6.42746302867524,35.9043551818058));
#18038=CARTESIAN_POINT('Ctrl Pts',(2.26953171457694,-6.37506978758111,35.911754753067));
#18039=CARTESIAN_POINT('Ctrl Pts',(2.4317372880176,-6.31732442863275,35.9199102114738));
#18040=CARTESIAN_POINT('Ctrl Pts',(2.5920021076197,-6.25329016858809,35.9280656698806));
#18041=CARTESIAN_POINT('Ctrl Pts',(2.74979703189377,-6.18311452937662,35.9362211282874));
#18042=CARTESIAN_POINT('Ctrl Pts',(2.90739989900286,-6.11302430314265,35.9443666604293));
#18043=CARTESIAN_POINT('Ctrl Pts',(3.062538524441,-6.03680772369536,35.9525121925711));
#18044=CARTESIAN_POINT('Ctrl Pts',(3.21469893288176,-5.95466201987391,35.960657724713));
#18045=CARTESIAN_POINT('Ctrl Pts',(3.36670613838588,-5.87259902457821,35.9687950555135));
#18046=CARTESIAN_POINT('Ctrl Pts',(3.51574077739738,-5.78461896195355,35.9769323863141));
#18047=CARTESIAN_POINT('Ctrl Pts',(3.66130888248412,-5.69096707660859,35.9850697171147));
#18048=CARTESIAN_POINT('Ctrl Pts',(3.80676101369243,-5.59738980357214,35.9932005649167));
#18049=CARTESIAN_POINT('Ctrl Pts',(3.94875180407487,-5.49814990200906,36.0013314127187));
#18050=CARTESIAN_POINT('Ctrl Pts',(4.08681194261969,-5.39353846242531,36.0094622605207));
#18051=CARTESIAN_POINT('Ctrl Pts',(4.22479109079321,-5.28898839116569,36.0175883385145));
#18052=CARTESIAN_POINT('Ctrl Pts',(4.3588438885813,-5.17907327744657,36.0257144165083));
#18053=CARTESIAN_POINT('Ctrl Pts',(4.48853008911084,-5.06412743117179,36.0338404945021));
#18054=CARTESIAN_POINT('Ctrl Pts',(4.61867613322107,-4.94877400792029,36.0419953860843));
#18055=CARTESIAN_POINT('Ctrl Pts',(4.74442424754717,-4.82835431686768,36.0501502776665));
#18056=CARTESIAN_POINT('Ctrl Pts',(4.86536263050205,-4.7032473328238,36.0583051692487));
#18057=CARTESIAN_POINT('Ctrl Pts',(4.98582939604845,-4.57862822227513,36.066428259605));
#18058=CARTESIAN_POINT('Ctrl Pts',(5.1015236317425,-4.44935858744685,36.0745513499613));
#18059=CARTESIAN_POINT('Ctrl Pts',(5.21207521702403,-4.31584996635471,36.0826744403176));
#18060=CARTESIAN_POINT('Ctrl Pts',(5.32263548332115,-4.18233086155563,36.0907981685361));
#18061=CARTESIAN_POINT('Ctrl Pts',(5.42805206148019,-4.04457238920789,36.0989218967546));
#18062=CARTESIAN_POINT('Ctrl Pts',(5.52799524678218,-3.90301903038579,36.107045624973));
#18063=CARTESIAN_POINT('Ctrl Pts',(5.62796529415142,-3.76142762578967,36.1151715366334));
#18064=CARTESIAN_POINT('Ctrl Pts',(5.72245880851381,-3.616039602499,36.1232974482937));
#18065=CARTESIAN_POINT('Ctrl Pts',(5.81118955509305,-3.46732821561176,36.131423359954));
#18066=CARTESIAN_POINT('Ctrl Pts',(5.90048774401992,-3.31766580394733,36.1396012376641));
#18067=CARTESIAN_POINT('Ctrl Pts',(5.98394900987722,-3.16463769718322,36.1477791153741));
#18068=CARTESIAN_POINT('Ctrl Pts',(6.06132904545269,-3.00875043876217,36.1559569930842));
#18069=CARTESIAN_POINT('Ctrl Pts',(6.13833976290137,-2.85360719641508,36.1640958395576));
#18070=CARTESIAN_POINT('Ctrl Pts',(6.20932707781422,-2.69563239375103,36.1722346860311));
#18071=CARTESIAN_POINT('Ctrl Pts',(6.27409909513282,-2.53534406825849,36.1803735325045));
#18072=CARTESIAN_POINT('Ctrl Pts',(6.33933705045781,-2.37390270745969,36.1885709258329));
#18073=CARTESIAN_POINT('Ctrl Pts',(6.39826982357931,-2.21011476910446,36.1967683191613));
#18074=CARTESIAN_POINT('Ctrl Pts',(6.45075295252284,-2.04452325629177,36.2049657124896));
#18075=CARTESIAN_POINT('Ctrl Pts',(6.50323608146636,-1.87893174347908,36.213163105818));
#18076=CARTESIAN_POINT('Ctrl Pts',(6.54926952645588,-1.7115370313218,36.2213604991463));
#18077=CARTESIAN_POINT('Ctrl Pts',(6.5887615325862,-1.54289029639584,36.2295578924747));
#18078=CARTESIAN_POINT('Ctrl Pts',(6.62839236357748,-1.3736507235307,36.2377841018117));
#18079=CARTESIAN_POINT('Ctrl Pts',(6.66155374818316,-1.20264664996418,36.2460103111486));
#18080=CARTESIAN_POINT('Ctrl Pts',(6.68808915414159,-1.03041373547409,36.2542365204856));
#18081=CARTESIAN_POINT('Ctrl Pts',(6.71459474870817,-0.858374317285196,
36.2624534880288));
#18082=CARTESIAN_POINT('Ctrl Pts',(6.73448913354669,-0.68510915845815,36.270670455572));
#18083=CARTESIAN_POINT('Ctrl Pts',(6.74766605066327,-0.511167163192595,
36.2788874231152));
#18084=CARTESIAN_POINT('Ctrl Pts',(6.76083080879079,-0.337385672755159,
36.2870968084586));
#18085=CARTESIAN_POINT('Ctrl Pts',(6.76729041689434,-0.162928945058542,
36.2953061938019));
#18086=CARTESIAN_POINT('Ctrl Pts',(6.76698997898025,0.0116457881213388,
36.3035155791453));
#18087=CARTESIAN_POINT('Ctrl Pts',(6.76668975801404,0.186094459915643,36.3117190364459));
#18088=CARTESIAN_POINT('Ctrl Pts',(6.75963921468863,0.360660610282066,36.3199224937465));
#18089=CARTESIAN_POINT('Ctrl Pts',(6.74583541268007,0.534783680595766,36.3281259510471));
#18090=CARTESIAN_POINT('Ctrl Pts',(6.73203880946492,0.708815944332309,36.3363251301789));
#18091=CARTESIAN_POINT('Ctrl Pts',(6.71149599205064,0.88240523168416,36.3445243093107));
#18092=CARTESIAN_POINT('Ctrl Pts',(6.68425608562888,1.0549926927393,36.3527234884425));
#18093=CARTESIAN_POINT('Ctrl Pts',(6.65702131179242,1.22754763459811,36.3609211226723));
#18094=CARTESIAN_POINT('Ctrl Pts',(6.6230920121863,1.39910077130668,36.3691187569021));
#18095=CARTESIAN_POINT('Ctrl Pts',(6.58256902214978,1.56909976376078,36.3773163911319));
#18096=CARTESIAN_POINT('Ctrl Pts',(6.54204895710705,1.73908648550145,36.3855134336475));
#18097=CARTESIAN_POINT('Ctrl Pts',(6.49493623180321,1.90751893729221,36.3937104761631));
#18098=CARTESIAN_POINT('Ctrl Pts',(6.44138251058095,2.07385639627768,36.4019075186787));
#18099=CARTESIAN_POINT('Ctrl Pts',(6.38782292162592,2.24021208039742,36.4101054593216));
#18100=CARTESIAN_POINT('Ctrl Pts',(6.32782104069586,2.40447197290469,36.4183033999644));
#18101=CARTESIAN_POINT('Ctrl Pts',(6.26157799339354,2.56611185115726,36.4265013406072));
#18102=CARTESIAN_POINT('Ctrl Pts',(6.19531564841639,2.72779881772985,36.4347016694432));
#18103=CARTESIAN_POINT('Ctrl Pts',(6.12280865150704,2.88686391793369,36.4429019982792));
#18104=CARTESIAN_POINT('Ctrl Pts',(6.04430574102376,3.04280415226272,36.4511023271151));
#18105=CARTESIAN_POINT('Ctrl Pts',(5.96572102847087,3.19890688036204,36.4593112009065));
#18106=CARTESIAN_POINT('Ctrl Pts',(5.88112808148358,3.35187791641154,36.467520074698));
#18107=CARTESIAN_POINT('Ctrl Pts',(5.79082145492598,3.50123919165329,36.4757289484894));
#18108=CARTESIAN_POINT('Ctrl Pts',(5.70046636179806,3.65068062744389,36.4839422278928));
#18109=CARTESIAN_POINT('Ctrl Pts',(5.60439167312652,3.79650814108492,36.4921555072962));
#18110=CARTESIAN_POINT('Ctrl Pts',(5.50293447000345,3.93827388824697,36.5003687866996));
#18111=CARTESIAN_POINT('Ctrl Pts',(5.40132886977468,4.0802469900957,36.5085940793151));
#18112=CARTESIAN_POINT('Ctrl Pts',(5.29432524174133,4.21814616946329,36.5168193719305));
#18113=CARTESIAN_POINT('Ctrl Pts',(5.18230084647513,4.35155684055984,36.5250446645459));
#18114=CARTESIAN_POINT('Ctrl Pts',(5.08098823782267,4.47221076668682,36.5324834536581));
#18115=CARTESIAN_POINT('Ctrl Pts',(4.97556975815014,4.58919384948255,36.5399222427702));
#18116=CARTESIAN_POINT('Ctrl Pts',(4.8663490095192,4.70222674033819,36.5473610318823));
#18117=CARTESIAN_POINT('Ctrl Pts',(4.74553618816832,4.82725630313545,36.5555893320115));
#18118=CARTESIAN_POINT('Ctrl Pts',(4.61973284761794,4.94780166435287,36.5638176321407));
#18119=CARTESIAN_POINT('Ctrl Pts',(4.4893047183625,5.06344074179685,36.5720459322699));
#18120=CARTESIAN_POINT('Ctrl Pts',(4.35906136466715,5.17891599510699,36.5802625754906));
#18121=CARTESIAN_POINT('Ctrl Pts',(4.22420654514427,5.28949858003894,36.5884792187114));
#18122=CARTESIAN_POINT('Ctrl Pts',(4.08514403561056,5.3948018692363,36.5966958619321));
#18123=CARTESIAN_POINT('Ctrl Pts',(3.94619570525636,5.50001869772473,36.6049057587653));
#18124=CARTESIAN_POINT('Ctrl Pts',(3.80304684589757,5.59996464364973,36.6131156555985));
#18125=CARTESIAN_POINT('Ctrl Pts',(3.65613618718165,5.6942916311672,36.6213255524317));
#18126=CARTESIAN_POINT('Ctrl Pts',(3.50934064317129,5.78854470693798,36.6295290162404));
#18127=CARTESIAN_POINT('Ctrl Pts',(3.35878947344755,5.87718740374395,36.6377324800492));
#18128=CARTESIAN_POINT('Ctrl Pts',(3.20495227163709,5.95991358465274,36.6459359438579));
#18129=CARTESIAN_POINT('Ctrl Pts',(3.16986235065928,5.97878324112545,36.6478071355684));
#18130=CARTESIAN_POINT('Ctrl Pts',(3.1346015831711,5.99734524642513,36.6496783272789));
#18131=CARTESIAN_POINT('Ctrl Pts',(3.09917575053261,6.01559628526638,36.6515495189894));
#18132=CARTESIAN_POINT('Origin',(0.,0.,-3.69717978381041));
#18133=CARTESIAN_POINT('',(3.09917575053254,6.01559628526642,39.0455765095777));
#18134=CARTESIAN_POINT('',(3.09917575053265,6.01559628526636,38.651392015122));
#18135=CARTESIAN_POINT('',(3.09917575053259,6.01559628526639,-3.69717978381041));
#18136=CARTESIAN_POINT('',(-6.767,1.02740353117442E-12,37.6971797838101));
#18137=CARTESIAN_POINT('Ctrl Pts',(-6.7669999895289,-0.000376451654302756,
37.6971797838101));
#18138=CARTESIAN_POINT('Ctrl Pts',(-6.76698972560559,-0.184878148371141,
37.7058050730204));
#18139=CARTESIAN_POINT('Ctrl Pts',(-6.75942954819334,-0.369194955863458,
37.7144303622308));
#18140=CARTESIAN_POINT('Ctrl Pts',(-6.74439035844876,-0.552709410869264,
37.7230556514411));
#18141=CARTESIAN_POINT('Ctrl Pts',(-6.72932680744503,-0.736521132102261,
37.7316949123421));
#18142=CARTESIAN_POINT('Ctrl Pts',(-6.70676007374303,-0.919527610808517,
37.740334173243));
#18143=CARTESIAN_POINT('Ctrl Pts',(-6.67681236999359,-1.101120145988,37.7489734341439));
#18144=CARTESIAN_POINT('Ctrl Pts',(-6.64678371593247,-1.28320353590694,
37.7576360474484));
#18145=CARTESIAN_POINT('Ctrl Pts',(-6.60933423103168,-1.46386504386166,
37.7662986607528));
#18146=CARTESIAN_POINT('Ctrl Pts',(-6.56463702324489,-1.64250715463966,
37.7749612740573));
#18147=CARTESIAN_POINT('Ctrl Pts',(-6.51987617494603,-1.82140361856344,
37.7836362213122));
#18148=CARTESIAN_POINT('Ctrl Pts',(-6.46784708064659,-1.99827466048662,
37.7923111685671));
#18149=CARTESIAN_POINT('Ctrl Pts',(-6.40877185034757,-2.17254053361327,
37.800986115822));
#18150=CARTESIAN_POINT('Ctrl Pts',(-6.34955095524285,-2.34723610298352,
37.8096824533364));
#18151=CARTESIAN_POINT('Ctrl Pts',(-6.28324927916287,-2.51931337808984,
37.8183787908509));
#18152=CARTESIAN_POINT('Ctrl Pts',(-6.21013697863793,-2.68821273461639,
37.8270751283653));
#18153=CARTESIAN_POINT('Ctrl Pts',(-6.15845308467603,-2.8076095580001,37.8332226655475));
#18154=CARTESIAN_POINT('Ctrl Pts',(-6.10336673855936,-2.92541880724379,
37.8393702027297));
#18155=CARTESIAN_POINT('Ctrl Pts',(-6.04498666341758,-3.04145117322366,
37.8455177399119));
#18156=CARTESIAN_POINT('Ctrl Pts',(-5.96687922318279,-3.1966923418769,37.8537426075895));
#18157=CARTESIAN_POINT('Ctrl Pts',(-5.88267816686097,-3.34914070709008,
37.8619674752671));
#18158=CARTESIAN_POINT('Ctrl Pts',(-5.79260661415228,-3.49828495318481,
37.8701923429446));
#18159=CARTESIAN_POINT('Ctrl Pts',(-5.70263653712959,-3.64726117159235,
37.8784079443882));
#18160=CARTESIAN_POINT('Ctrl Pts',(-5.60680931720374,-3.79294037893727,
37.8866235458317));
#18161=CARTESIAN_POINT('Ctrl Pts',(-5.50539515313227,-3.93483331386067,
37.8948391472752));
#18162=CARTESIAN_POINT('Ctrl Pts',(-5.40407486732728,-4.07659489964878,
37.9030471436034));
#18163=CARTESIAN_POINT('Ctrl Pts',(-5.29717814439985,-4.21457690309378,
37.9112551399315));
#18164=CARTESIAN_POINT('Ctrl Pts',(-5.18501994507776,-4.34831659026178,
37.9194631362596));
#18165=CARTESIAN_POINT('Ctrl Pts',(-5.07294304213086,-4.4819593380009,37.927665183131));
#18166=CARTESIAN_POINT('Ctrl Pts',(-4.95561248858411,-4.61136562047138,
37.9358672300025));
#18167=CARTESIAN_POINT('Ctrl Pts',(-4.83338525976377,-4.73610345439141,
37.9440692768739));
#18168=CARTESIAN_POINT('Ctrl Pts',(-4.71122208139883,-4.86077592222941,
37.9522670256455));
#18169=CARTESIAN_POINT('Ctrl Pts',(-4.58416759013228,-4.98078455948131,
37.960464774417));
#18170=CARTESIAN_POINT('Ctrl Pts',(-4.45261762527738,-5.09573206547099,
37.9686625231886));
#18171=CARTESIAN_POINT('Ctrl Pts',(-4.32109275093618,-5.21065764753256,
37.9768587084042));
#18172=CARTESIAN_POINT('Ctrl Pts',(-4.18507437668023,-5.32052378059402,
37.9850548936199));
#18173=CARTESIAN_POINT('Ctrl Pts',(-4.04499385664279,-5.42497130865427,
37.9932510788355));
#18174=CARTESIAN_POINT('Ctrl Pts',(-3.90492369944608,-5.52941110992213,
38.0014466577158));
#18175=CARTESIAN_POINT('Ctrl Pts',(-3.7607922820659,-5.62843288929932,38.0096422365962));
#18176=CARTESIAN_POINT('Ctrl Pts',(-3.61306252342612,-5.72171899011247,
38.0178378154765));
#18177=CARTESIAN_POINT('Ctrl Pts',(-3.46531681582039,-5.81501516213172,
38.0260342791549));
#18178=CARTESIAN_POINT('Ctrl Pts',(-3.3139722964519,-5.90257423027229,38.0342307428334));
#18179=CARTESIAN_POINT('Ctrl Pts',(-3.15951926684773,-5.98412291003602,
38.0424272065118));
#18180=CARTESIAN_POINT('Ctrl Pts',(-3.00502146141335,-6.0656952307076,38.0506260463396));
#18181=CARTESIAN_POINT('Ctrl Pts',(-2.84741366799579,-6.1412535248539,38.0588248861674));
#18182=CARTESIAN_POINT('Ctrl Pts',(-2.68720912256893,-6.21057132086754,
38.0670237259952));
#18183=CARTESIAN_POINT('Ctrl Pts',(-2.52683723893663,-6.27996152129117,
38.0752311297444));
#18184=CARTESIAN_POINT('Ctrl Pts',(-2.36386351407683,-6.34309805802945,
38.0834385334936));
#18185=CARTESIAN_POINT('Ctrl Pts',(-2.19882036682686,-6.39980296528162,
38.0916459372429));
#18186=CARTESIAN_POINT('Ctrl Pts',(-2.03368881373325,-6.4565382466829,38.0998577373119));
#18187=CARTESIAN_POINT('Ctrl Pts',(-1.86648597173678,-6.50683492739292,
38.1080695373809));
#18188=CARTESIAN_POINT('Ctrl Pts',(-1.69775751610964,-6.55056550356481,
38.1162813374499));
#18189=CARTESIAN_POINT('Ctrl Pts',(-1.52878066861958,-6.59436045725524,
38.1245052264361));
#18190=CARTESIAN_POINT('Ctrl Pts',(-1.35827406968175,-6.63156991222203,
38.1327291154222));
#18191=CARTESIAN_POINT('Ctrl Pts',(-1.18679291955195,-6.66211764877365,
38.1409530044084));
#18192=CARTESIAN_POINT('Ctrl Pts',(-1.02834730136684,-6.69034322924366,
38.1485517356585));
#18193=CARTESIAN_POINT('Ctrl Pts',(-0.869069958548886,-6.71288195291813,
38.1561504669086));
#18194=CARTESIAN_POINT('Ctrl Pts',(-0.709400254238555,-6.7297132390085,
38.1637491981587));
#18195=CARTESIAN_POINT('Ctrl Pts',(-0.536574152570794,-6.74793138235397,
38.1719740464807));
#18196=CARTESIAN_POINT('Ctrl Pts',(-0.362803248484585,-6.75951328236136,
38.1801988948027));
#18197=CARTESIAN_POINT('Ctrl Pts',(-0.188638322026488,-6.76437022814859,
38.1884237431248));
#18198=CARTESIAN_POINT('Ctrl Pts',(-0.0146695438915345,-6.76922170393799,
38.196639328444));
#18199=CARTESIAN_POINT('Ctrl Pts',(0.159692017619453,-6.76736329694443,
38.2048549137632));
#18200=CARTESIAN_POINT('Ctrl Pts',(0.333888685743401,-6.75875782563132,
38.2130704990824));
#18201=CARTESIAN_POINT('Ctrl Pts',(0.50792416937496,-6.75016031697638,38.2212784825056));
#18202=CARTESIAN_POINT('Ctrl Pts',(0.681794707400922,-6.73482819479659,
38.2294864659289));
#18203=CARTESIAN_POINT('Ctrl Pts',(0.854940742096523,-6.71277627569275,
38.2376944493521));
#18204=CARTESIAN_POINT('Ctrl Pts',(1.02796134171457,-6.69074033202946,38.2458964865286));
#18205=CARTESIAN_POINT('Ctrl Pts',(1.20025812897806,-6.66199433299192,38.2540985237052));
#18206=CARTESIAN_POINT('Ctrl Pts',(1.37127470334437,-6.62660506503653,38.2623005608817));
#18207=CARTESIAN_POINT('Ctrl Pts',(1.54220172695864,-6.59123432824148,38.2704983031611));
#18208=CARTESIAN_POINT('Ctrl Pts',(1.71184952265965,-6.54922732512061,38.2786960454405));
#18209=CARTESIAN_POINT('Ctrl Pts',(1.87966985817477,-6.50070228700479,38.2868937877199));
#18210=CARTESIAN_POINT('Ctrl Pts',(2.04745828543029,-6.45218647512193,38.2950899713342));
#18211=CARTESIAN_POINT('Ctrl Pts',(2.21341959856338,-6.39715519033401,38.3032861549486));
#18212=CARTESIAN_POINT('Ctrl Pts',(2.37701845635905,-6.33577716291604,38.3114823385629));
#18213=CARTESIAN_POINT('Ctrl Pts',(2.5406052709962,-6.27440365377726,38.3196779188238));
#18214=CARTESIAN_POINT('Ctrl Pts',(2.70182964036839,-6.20668445767194,38.3278734990847));
#18215=CARTESIAN_POINT('Ctrl Pts',(2.86017407227692,-6.13283729413025,38.3360690793456));
#18216=CARTESIAN_POINT('Ctrl Pts',(3.01853565672223,-6.05898213115232,38.3442655473863));
#18217=CARTESIAN_POINT('Ctrl Pts',(3.17401635690134,-5.97899782992739,38.352462015427));
#18218=CARTESIAN_POINT('Ctrl Pts',(3.3261212073716,-5.89314913385644,38.3606584834677));
#18219=CARTESIAN_POINT('Ctrl Pts',(3.47827020827584,-5.80727551907201,38.3688573306411));
#18220=CARTESIAN_POINT('Ctrl Pts',(3.62704109525103,-5.71553429516912,38.3770561778145));
#18221=CARTESIAN_POINT('Ctrl Pts',(3.77196588758327,-5.61823480667266,38.3852550249879));
#18222=CARTESIAN_POINT('Ctrl Pts',(3.91704214041628,-5.52083363074911,38.3934624407538));
#18223=CARTESIAN_POINT('Ctrl Pts',(4.05826396977074,-5.4178627850371,38.4016698565198));
#18224=CARTESIAN_POINT('Ctrl Pts',(4.19519383168902,-5.30967397441297,38.4098772722858));
#18225=CARTESIAN_POINT('Ctrl Pts',(4.3321970831972,-5.20142717839156,38.4180890869379));
#18226=CARTESIAN_POINT('Ctrl Pts',(4.46490350900989,-5.08795707524879,38.42630090159));
#18227=CARTESIAN_POINT('Ctrl Pts',(4.59291085173824,-4.96965380162291,38.4345127162422));
#18228=CARTESIAN_POINT('Ctrl Pts',(4.72110670473902,-4.85117630844163,38.4427366240398));
#18229=CARTESIAN_POINT('Ctrl Pts',(4.84458939110564,-4.72785167406962,38.4509605318374));
#18230=CARTESIAN_POINT('Ctrl Pts',(4.96299464867785,-4.60010577239209,38.459184439635));
#18231=CARTESIAN_POINT('Ctrl Pts',(5.07239891993161,-4.48207091849077,38.4667831785585));
#18232=CARTESIAN_POINT('Ctrl Pts',(5.17746867850984,-4.36026198476384,38.4743819174819));
#18233=CARTESIAN_POINT('Ctrl Pts',(5.277949092835,-4.23503747013438,38.4819806564054));
#18234=CARTESIAN_POINT('Ctrl Pts',(5.3857319860596,-4.10071218316122,38.4901316385797));
#18235=CARTESIAN_POINT('Ctrl Pts',(5.4885529214214,-3.96205854079507,38.498282620754));
#18236=CARTESIAN_POINT('Ctrl Pts',(5.58604061641682,-3.8194815396519,38.5064336029282));
#18237=CARTESIAN_POINT('Ctrl Pts',(5.6834150704192,-3.6770701549098,38.5145751169813));
#18238=CARTESIAN_POINT('Ctrl Pts',(5.77546841148473,-3.53074478191807,38.5227166310343));
#18239=CARTESIAN_POINT('Ctrl Pts',(5.86186854422283,-3.3809445677578,38.5308581450874));
#18240=CARTESIAN_POINT('Ctrl Pts',(5.94818649695584,-3.23128683697077,38.5389919152904));
#18241=CARTESIAN_POINT('Ctrl Pts',(6.02886176488743,-3.07816115961845,38.5471256854935));
#18242=CARTESIAN_POINT('Ctrl Pts',(6.10360465212269,-2.92203683251705,38.5552594556965));
#18243=CARTESIAN_POINT('Ctrl Pts',(6.17829216717965,-2.76602816784719,38.5633872001145));
#18244=CARTESIAN_POINT('Ctrl Pts',(6.24705589525814,-2.60702560525452,38.5715149445325));
#18245=CARTESIAN_POINT('Ctrl Pts',(6.30965133453841,-2.44552428664238,38.5796426889505));
#18246=CARTESIAN_POINT('Ctrl Pts',(6.37221356111953,-2.28410865949224,38.5877661208446));
#18247=CARTESIAN_POINT('Ctrl Pts',(6.42861388498426,-2.12019725695791,38.5958895527386));
#18248=CARTESIAN_POINT('Ctrl Pts',(6.478655346468,-1.95430650146839,38.6040129846326));
#18249=CARTESIAN_POINT('Ctrl Pts',(6.52901425130072,-1.78736340027538,38.6121879483835));
#18250=CARTESIAN_POINT('Ctrl Pts',(6.57293318221682,-1.61841608794561,38.6203629121343));
#18251=CARTESIAN_POINT('Ctrl Pts',(6.61026179986248,-1.44800826561137,38.6285378758851));
#18252=CARTESIAN_POINT('Ctrl Pts',(6.64734669787008,-1.27871304094087,38.6366594650582));
#18253=CARTESIAN_POINT('Ctrl Pts',(6.67792702986911,-1.10797668812534,38.6447810542312));
#18254=CARTESIAN_POINT('Ctrl Pts',(6.70190635199328,-0.936344086921117,
38.6529026434042));
#18255=CARTESIAN_POINT('Ctrl Pts',(6.72588883987977,-0.764688826693477,
38.6610253047936));
#18256=CARTESIAN_POINT('Ctrl Pts',(6.74326853143352,-0.592137444899972,
38.6691479661829));
#18257=CARTESIAN_POINT('Ctrl Pts',(6.75400071760543,-0.419241346464561,
38.6772706275723));
#18258=CARTESIAN_POINT('Ctrl Pts',(6.76473636437172,-0.246289497666847,
38.6853959081145));
#18259=CARTESIAN_POINT('Ctrl Pts',(6.76882021474938,-0.0729930759797391,
38.6935211886568));
#18260=CARTESIAN_POINT('Ctrl Pts',(6.76625967295635,0.100095145360026,38.701646469199));
#18261=CARTESIAN_POINT('Ctrl Pts',(6.76367123459179,0.275069126955801,38.7098602729868));
#18262=CARTESIAN_POINT('Ctrl Pts',(6.75429278297422,0.449829960960584,38.7180740767746));
#18263=CARTESIAN_POINT('Ctrl Pts',(6.73818582979381,0.623811448408874,38.7262878805624));
#18264=CARTESIAN_POINT('Ctrl Pts',(6.7222248955591,0.796215691974586,38.7344272214175));
#18265=CARTESIAN_POINT('Ctrl Pts',(6.69965706508996,0.967854307981028,38.7425665622727));
#18266=CARTESIAN_POINT('Ctrl Pts',(6.6705937051536,1.13818654919355,38.7507059031279));
#18267=CARTESIAN_POINT('Ctrl Pts',(6.64113151506911,1.3108562225937,38.758956938382));
#18268=CARTESIAN_POINT('Ctrl Pts',(6.60499431030248,1.48218302291829,38.767207973636));
#18269=CARTESIAN_POINT('Ctrl Pts',(6.56235025601427,1.65161984651114,38.7754590088901));
#18270=CARTESIAN_POINT('Ctrl Pts',(6.51970620172607,1.82105667010392,38.7837100441442));
#18271=CARTESIAN_POINT('Ctrl Pts',(6.47055547032833,1.98860316748763,38.7919610793983));
#18272=CARTESIAN_POINT('Ctrl Pts',(6.41511645767085,2.15373392844164,38.8002121146524));
#18273=CARTESIAN_POINT('Ctrl Pts',(6.35979709247321,2.31850830721741,38.8084453426736));
#18274=CARTESIAN_POINT('Ctrl Pts',(6.29804399928013,2.48139190946777,38.8166785706948));
#18275=CARTESIAN_POINT('Ctrl Pts',(6.23000316624065,2.64184586011968,38.824911798716));
#18276=CARTESIAN_POINT('Ctrl Pts',(6.16204578460794,2.80210301559281,38.8331349287647));
#18277=CARTESIAN_POINT('Ctrl Pts',(6.08781615935948,2.95993612690317,38.8413580588134));
#18278=CARTESIAN_POINT('Ctrl Pts',(6.00751009732845,3.114821251773,38.8495811888621));
#18279=CARTESIAN_POINT('Ctrl Pts',(5.92730567465883,3.26951034629613,38.8577939113069));
#18280=CARTESIAN_POINT('Ctrl Pts',(5.84104030739634,3.42125857489348,38.8660066337517));
#18281=CARTESIAN_POINT('Ctrl Pts',(5.74895779903885,3.56956204944954,38.8742193561965));
#18282=CARTESIAN_POINT('Ctrl Pts',(5.65694254141812,3.7177572133383,38.8824260806331));
#18283=CARTESIAN_POINT('Ctrl Pts',(5.55911878981143,3.86251232953619,38.8906328050697));
#18284=CARTESIAN_POINT('Ctrl Pts',(5.45577646498682,4.0033476196923,38.8988395295064));
#18285=CARTESIAN_POINT('Ctrl Pts',(5.3524908650151,4.14410560501586,38.9070417492521));
#18286=CARTESIAN_POINT('Ctrl Pts',(5.24369293567096,4.28094776110854,38.9152439689977));
#18287=CARTESIAN_POINT('Ctrl Pts',(5.12971618532012,4.41342280526859,38.9234461887434));
#18288=CARTESIAN_POINT('Ctrl Pts',(5.01578131994848,4.54584916656609,38.9316453942796));
#18289=CARTESIAN_POINT('Ctrl Pts',(4.89667165805555,4.67391134162312,38.9398445998157));
#18290=CARTESIAN_POINT('Ctrl Pts',(4.77276134030782,4.79719065583839,38.9480438053519));
#18291=CARTESIAN_POINT('Ctrl Pts',(4.64884851108807,4.9204724687362,38.9562431770734));
#18292=CARTESIAN_POINT('Ctrl Pts',(4.52013507833853,5.03897096712496,38.9644425487949));
#18293=CARTESIAN_POINT('Ctrl Pts',(4.38703272241468,5.15230364909357,38.9726419205164));
#18294=CARTESIAN_POINT('Ctrl Pts',(4.2539342249196,5.26563304572527,38.9808410545509));
#18295=CARTESIAN_POINT('Ctrl Pts',(4.11644733341651,5.37379669510969,38.9890401885855));
#18296=CARTESIAN_POINT('Ctrl Pts',(3.97501729072259,5.47645200275292,38.99723932262));
#18297=CARTESIAN_POINT('Ctrl Pts',(3.83350849451294,5.57916447269513,39.0054430222378));
#18298=CARTESIAN_POINT('Ctrl Pts',(3.68805245071846,5.67636226201041,39.0136467218556));
#18299=CARTESIAN_POINT('Ctrl Pts',(3.53912450002771,5.76774538041543,39.0218504214734));
#18300=CARTESIAN_POINT('Ctrl Pts',(3.39555197202584,5.85584237809284,39.0297591175081));
#18301=CARTESIAN_POINT('Ctrl Pts',(3.24875316198388,5.93853548124723,39.0376678135429));
#18302=CARTESIAN_POINT('Ctrl Pts',(3.09917575053254,6.01559628526642,39.0455765095776));
#18303=CARTESIAN_POINT('Ctrl Pts',(3.09917575053255,6.01559628526641,37.0457515827422));
#18304=CARTESIAN_POINT('Ctrl Pts',(2.93382384459258,6.10078395293763,37.0545010306546));
#18305=CARTESIAN_POINT('Ctrl Pts',(2.76495772122973,6.17915010267054,37.0632504785671));
#18306=CARTESIAN_POINT('Ctrl Pts',(2.59315093316697,6.25042856433183,37.0719999264795));
#18307=CARTESIAN_POINT('Ctrl Pts',(2.42134553245598,6.32170645041459,37.0807493037395));
#18308=CARTESIAN_POINT('Ctrl Pts',(2.24659977927567,6.38589665313466,37.0894986809995));
#18309=CARTESIAN_POINT('Ctrl Pts',(2.0695071868989,6.44278115439085,37.0982480582595));
#18310=CARTESIAN_POINT('Ctrl Pts',(1.89241596572836,6.49966521519731,37.1069973677741));
#18311=CARTESIAN_POINT('Ctrl Pts',(1.71297821457177,6.54924360009551,37.1157466772888));
#18312=CARTESIAN_POINT('Ctrl Pts',(1.53180337335828,6.5913479217356,37.1244959868034));
#18313=CARTESIAN_POINT('Ctrl Pts',(1.35062987477768,6.63345193135308,37.1332452314796));
#18314=CARTESIAN_POINT('Ctrl Pts',(1.16771959102939,6.6680819236824,37.1419944761557));
#18315=CARTESIAN_POINT('Ctrl Pts',(0.983693746906732,6.6951202836317,37.1507437208318));
#18316=CARTESIAN_POINT('Ctrl Pts',(0.799669205419833,6.72215845218867,37.159492903576));
#18317=CARTESIAN_POINT('Ctrl Pts',(0.614529402873514,6.74160505424578,37.1682420863202));
#18318=CARTESIAN_POINT('Ctrl Pts',(0.428903127363362,6.75339404354121,37.1769912690643));
#18319=CARTESIAN_POINT('Ctrl Pts',(0.243278104164028,6.7651829533033,37.1857403927829));
#18320=CARTESIAN_POINT('Ctrl Pts',(0.0571669005393018,6.76931433552276,
37.1944895165015));
#18321=CARTESIAN_POINT('Ctrl Pts',(-0.128798404777293,6.76577415902473,
37.2032386402202));
#18322=CARTESIAN_POINT('Ctrl Pts',(-0.314762517258765,6.76223400523443,
37.2119877078194));
#18323=CARTESIAN_POINT('Ctrl Pts',(-0.500580446819064,6.75102239665092,
37.2207367754186));
#18324=CARTESIAN_POINT('Ctrl Pts',(-0.685621118842053,6.73217741012503,
37.2294858430178));
#18325=CARTESIAN_POINT('Ctrl Pts',(-0.870660665414095,6.71333253821777,
37.2382348574035));
#18326=CARTESIAN_POINT('Ctrl Pts',(-1.05492267885464,6.68685441030616,37.2469838717893));
#18327=CARTESIAN_POINT('Ctrl Pts',(-1.23778137635245,6.65283295028179,37.2557328861751));
#18328=CARTESIAN_POINT('Ctrl Pts',(-1.42999922978842,6.61707018861866,37.2649296965425));
#18329=CARTESIAN_POINT('Ctrl Pts',(-1.62066601233693,6.57297172934414,37.2741265069099));
#18330=CARTESIAN_POINT('Ctrl Pts',(-1.80906628500386,6.52070304311294,37.2833233172773));
#18331=CARTESIAN_POINT('Ctrl Pts',(-1.98831342545523,6.47097374915032,37.2920733150151));
#18332=CARTESIAN_POINT('Ctrl Pts',(-2.16550875896693,6.41384933989531,37.3008233127528));
#18333=CARTESIAN_POINT('Ctrl Pts',(-2.34005036713999,6.3495238624048,37.3095733104906));
#18334=CARTESIAN_POINT('Ctrl Pts',(-2.51458843547074,6.28519968948602,37.3183231307715));
#18335=CARTESIAN_POINT('Ctrl Pts',(-2.68647261718038,6.21367483971106,37.3270729510523));
#18336=CARTESIAN_POINT('Ctrl Pts',(-2.85511905908712,6.13519226743853,37.3358227713332));
#18337=CARTESIAN_POINT('Ctrl Pts',(-3.02376230488866,6.05671118252946,37.3445724257917));
#18338=CARTESIAN_POINT('Ctrl Pts',(-3.18916767379887,5.97127275992642,37.3533220802503));
#18339=CARTESIAN_POINT('Ctrl Pts',(-3.35077334102771,5.87916720438006,37.3620717347088));
#18340=CARTESIAN_POINT('Ctrl Pts',(-3.5123761603735,5.78706327195654,37.3708212349772));
#18341=CARTESIAN_POINT('Ctrl Pts',(-3.6701791630228,5.68829258362311,37.3795707352457));
#18342=CARTESIAN_POINT('Ctrl Pts',(-3.82364636566442,5.58319061741056,37.3883202355141));
#18343=CARTESIAN_POINT('Ctrl Pts',(-3.97711106778777,5.47809036367717,37.3970695932226));
#18344=CARTESIAN_POINT('Ctrl Pts',(-4.12623987481906,5.36665920043241,37.405818950931));
#18345=CARTESIAN_POINT('Ctrl Pts',(-4.27052628213908,5.24927559512352,37.4145683086394));
#18346=CARTESIAN_POINT('Ctrl Pts',(-4.41481053024952,5.13189374643059,37.4233175354159));
#18347=CARTESIAN_POINT('Ctrl Pts',(-4.55425230136499,5.00855981477381,37.4320667621925));
#18348=CARTESIAN_POINT('Ctrl Pts',(-4.68837800630513,4.8796926819211,37.440815988969));
#18349=CARTESIAN_POINT('Ctrl Pts',(-4.8225018822886,4.75082730631844,37.4495650964398));
#18350=CARTESIAN_POINT('Ctrl Pts',(-4.95130963052933,4.61642907903561,37.4583142039107));
#18351=CARTESIAN_POINT('Ctrl Pts',(-5.07436379033335,4.47695444731726,37.4670633113815));
#18352=CARTESIAN_POINT('Ctrl Pts',(-5.19741643562761,4.33748153220638,37.4758123111712));
#18353=CARTESIAN_POINT('Ctrl Pts',(-5.31471544462718,4.19293255254658,37.484561310961));
#18354=CARTESIAN_POINT('Ctrl Pts',(-5.42586245275563,4.0437984177969,37.4933103107507));
#18355=CARTESIAN_POINT('Ctrl Pts',(-5.53702160019089,3.89464799484434,37.5020602660929));
#18356=CARTESIAN_POINT('Ctrl Pts',(-5.64202723081188,3.74091164443945,37.510810221435));
#18357=CARTESIAN_POINT('Ctrl Pts',(-5.74052265232905,3.58311159163332,37.5195601767772));
#18358=CARTESIAN_POINT('Ctrl Pts',(-5.83901427066862,3.42531763191879,37.5283097942596));
#18359=CARTESIAN_POINT('Ctrl Pts',(-5.93099603115689,3.26346052695704,37.5370594117421));
#18360=CARTESIAN_POINT('Ctrl Pts',(-6.01615550622709,3.09809004467164,37.5458090292245));
#18361=CARTESIAN_POINT('Ctrl Pts',(-6.10131214578765,2.932725068639,37.5545583553756));
#18362=CARTESIAN_POINT('Ctrl Pts',(-6.17964682328723,2.76384720416951,37.5633076815267));
#18363=CARTESIAN_POINT('Ctrl Pts',(-6.25089348288547,2.59203002791634,37.5720570076778));
#18364=CARTESIAN_POINT('Ctrl Pts',(-6.32213814889322,2.42021765937052,37.5808060890094));
#18365=CARTESIAN_POINT('Ctrl Pts',(-6.38629508412584,2.24546640831922,37.589555170341));
#18366=CARTESIAN_POINT('Ctrl Pts',(-6.44314639819817,2.06836976660026,37.5983042516726));
#18367=CARTESIAN_POINT('Ctrl Pts',(-6.50000285283708,1.8912571115825,37.607054124107));
#18368=CARTESIAN_POINT('Ctrl Pts',(-6.54955227673259,1.71179891440219,37.6158039965414));
#18369=CARTESIAN_POINT('Ctrl Pts',(-6.59162635926396,1.53060476278385,37.6245538689758));
#18370=CARTESIAN_POINT('Ctrl Pts',(-6.63369752055207,1.34942319164646,37.6333031338983));
#18371=CARTESIAN_POINT('Ctrl Pts',(-6.66829431424263,1.16650618642651,37.6420523988208));
#18372=CARTESIAN_POINT('Ctrl Pts',(-6.69529923745425,0.982474997617998,
37.6508016637433));
#18373=CARTESIAN_POINT('Ctrl Pts',(-6.72230554731451,0.798434359177128,
37.659551377923));
#18374=CARTESIAN_POINT('Ctrl Pts',(-6.74171916496709,0.61327970623967,37.6683010921027));
#18375=CARTESIAN_POINT('Ctrl Pts',(-6.75347414817279,0.427639953654658,
37.6770508062824));
#18376=CARTESIAN_POINT('Ctrl Pts',(-6.76248837758747,0.285283364197911,
37.6837604654583));
#18377=CARTESIAN_POINT('Ctrl Pts',(-6.76699999999998,0.142641701104516,
37.6904701246342));
#18378=CARTESIAN_POINT('Ctrl Pts',(-6.767,1.02740346869295E-12,37.6971797838101));
#18379=CARTESIAN_POINT('',(-6.76798064037177,0.0012455647848279,37.3045171512176));
#18380=CARTESIAN_POINT('Ctrl Pts',(3.09917575053261,6.01559628526638,36.6515495189894));
#18381=CARTESIAN_POINT('Ctrl Pts',(2.94396117623734,6.09556129986739,36.6597479494324));
#18382=CARTESIAN_POINT('Ctrl Pts',(2.78557597437919,6.1695531728888,36.6679463798753));
#18383=CARTESIAN_POINT('Ctrl Pts',(2.62452199755003,6.23732100219125,36.6761448103182));
#18384=CARTESIAN_POINT('Ctrl Pts',(2.46348890435358,6.30508004413876,36.6843421776827));
#18385=CARTESIAN_POINT('Ctrl Pts',(2.29978805308302,6.36661650452126,36.6925395450472));
#18386=CARTESIAN_POINT('Ctrl Pts',(2.1339428144838,6.42172695343807,36.7007369124117));
#18387=CARTESIAN_POINT('Ctrl Pts',(1.9681026353072,6.47683572110642,36.7089340297));
#18388=CARTESIAN_POINT('Ctrl Pts',(1.80011853925938,6.5255187538798,36.7171311469883));
#18389=CARTESIAN_POINT('Ctrl Pts',(1.63053057587416,6.56762202331555,36.7253282642766));
#18390=CARTESIAN_POINT('Ctrl Pts',(1.46091696375125,6.60973166051286,36.7335266213092));
#18391=CARTESIAN_POINT('Ctrl Pts',(1.28969934923995,6.64525946555615,36.7417249783418));
#18392=CARTESIAN_POINT('Ctrl Pts',(1.11742958154676,6.67410219657178,36.7499233353744));
#18393=CARTESIAN_POINT('Ctrl Pts',(0.945102449594142,6.70295453195344,36.758124422385));
#18394=CARTESIAN_POINT('Ctrl Pts',(0.771722820188464,6.72511730005566,36.7663255093956));
#18395=CARTESIAN_POINT('Ctrl Pts',(0.59784934942649,6.74053893656808,36.7745265964062));
#18396=CARTESIAN_POINT('Ctrl Pts',(0.423791854826353,6.75597689499971,36.7827363632661));
#18397=CARTESIAN_POINT('Ctrl Pts',(0.249239832417566,6.76465943836995,36.7909461301259));
#18398=CARTESIAN_POINT('Ctrl Pts',(0.0747546027331646,6.7665870828188,36.7991558969858));
#18399=CARTESIAN_POINT('Ctrl Pts',(-0.0998307939834776,6.76851583387377,
36.8073703768404));
#18400=CARTESIAN_POINT('Ctrl Pts',(-0.274348963605343,6.76368196601679,
36.8155848566951));
#18401=CARTESIAN_POINT('Ctrl Pts',(-0.448242117126577,6.75213803209279,
36.8237993365497));
#18402=CARTESIAN_POINT('Ctrl Pts',(-0.622378968351616,6.74057792024498,
36.8320253283578));
#18403=CARTESIAN_POINT('Ctrl Pts',(-0.795888697323502,6.72228899251469,
36.8402513201658));
#18404=CARTESIAN_POINT('Ctrl Pts',(-0.968221020471342,6.69737538559079,
36.8484773119738));
#18405=CARTESIAN_POINT('Ctrl Pts',(-1.08474943022036,6.680529195956,36.8540395984125));
#18406=CARTESIAN_POINT('Ctrl Pts',(-1.20073970968487,6.66065510271486,36.8596018848513));
#18407=CARTESIAN_POINT('Ctrl Pts',(-1.31602549799756,6.63779827116042,36.86516417129));
#18408=CARTESIAN_POINT('Ctrl Pts',(-1.48499807432253,6.60429737073804,36.8733167275033));
#18409=CARTESIAN_POINT('Ctrl Pts',(-1.65295490583598,6.56428777962686,36.8814692837165));
#18410=CARTESIAN_POINT('Ctrl Pts',(-1.81935102344975,6.51784096564747,36.8896218399298));
#18411=CARTESIAN_POINT('Ctrl Pts',(-1.98555436714975,6.47144796142183,36.8977649512101));
#18412=CARTESIAN_POINT('Ctrl Pts',(-2.1502002476918,6.41863267682765,36.9059080624905));
#18413=CARTESIAN_POINT('Ctrl Pts',(-2.31275175379891,6.35951793183257,36.9140511737708));
#18414=CARTESIAN_POINT('Ctrl Pts',(-2.4751491144978,6.30045924455556,36.9221865630482));
#18415=CARTESIAN_POINT('Ctrl Pts',(-2.63545571358102,6.23511311381613,36.9303219523256));
#18416=CARTESIAN_POINT('Ctrl Pts',(-2.79314772817954,6.16365271316981,36.9384573416029));
#18417=CARTESIAN_POINT('Ctrl Pts',(-2.95072334045501,6.09224506190754,36.9465867256415));
#18418=CARTESIAN_POINT('Ctrl Pts',(-3.10568787962654,6.01473227781286,36.95471610968));
#18419=CARTESIAN_POINT('Ctrl Pts',(-3.25753551730379,5.93133638849664,36.9628454937185));
#18420=CARTESIAN_POINT('Ctrl Pts',(-3.40930296202517,5.84798454176794,36.9709705845106));
#18421=CARTESIAN_POINT('Ctrl Pts',(-3.55795646378905,5.75875595303,36.9790956753026));
#18422=CARTESIAN_POINT('Ctrl Pts',(-3.70301292002846,5.66391951868159,36.9872207660947));
#18423=CARTESIAN_POINT('Ctrl Pts',(-3.84862308820951,5.56872107310279,36.9953768721198));
#18424=CARTESIAN_POINT('Ctrl Pts',(-3.99060835947779,5.46787204544738,37.003532978145));
#18425=CARTESIAN_POINT('Ctrl Pts',(-4.128507246566,5.36168974438582,37.0116890841701));
#18426=CARTESIAN_POINT('Ctrl Pts',(-4.26585111557264,5.255934807883,37.0198123633435));
#18427=CARTESIAN_POINT('Ctrl Pts',(-4.39914115454755,5.14488969097722,37.0279356425169));
#18428=CARTESIAN_POINT('Ctrl Pts',(-4.52795285153677,5.02890962080847,37.0360589216903));
#18429=CARTESIAN_POINT('Ctrl Pts',(-4.65678170089149,4.91291410691373,37.0441832825469));
#18430=CARTESIAN_POINT('Ctrl Pts',(-4.78113074859226,4.79198257568056,37.0523076434036));
#18431=CARTESIAN_POINT('Ctrl Pts',(-4.90061089322392,4.66650853135565,37.0604320042602));
#18432=CARTESIAN_POINT('Ctrl Pts',(-5.02012967935872,4.54099390701895,37.0685589926456));
#18433=CARTESIAN_POINT('Ctrl Pts',(-5.13477617461776,4.41093410891703,37.076685981031));
#18434=CARTESIAN_POINT('Ctrl Pts',(-5.24420029377589,4.27675721531639,37.0848129694164));
#18435=CARTESIAN_POINT('Ctrl Pts',(-5.3543318274073,4.14171288337363,37.0929924978565));
#18436=CARTESIAN_POINT('Ctrl Pts',(-5.45917298917913,4.00249832951863,37.1011720262966));
#18437=CARTESIAN_POINT('Ctrl Pts',(-5.55841052770631,3.85958047013969,37.1093515547367));
#18438=CARTESIAN_POINT('Ctrl Pts',(-5.657180724671,3.71733565703638,37.1174925631404));
#18439=CARTESIAN_POINT('Ctrl Pts',(-5.75039982084009,3.57142268597552,37.125633571544));
#18440=CARTESIAN_POINT('Ctrl Pts',(-5.83780485202429,3.42232720669454,37.1337745799477));
#18441=CARTESIAN_POINT('Ctrl Pts',(-5.92583023233854,3.27217353603015,37.141973368406));
#18442=CARTESIAN_POINT('Ctrl Pts',(-6.00795853652428,3.11879234879113,37.1501721568644));
#18443=CARTESIAN_POINT('Ctrl Pts',(-6.08397035698332,2.96270040593853,37.1583709453227));
#18444=CARTESIAN_POINT('Ctrl Pts',(-6.15998217744236,2.80660846308593,37.166569733781));
#18445=CARTESIAN_POINT('Ctrl Pts',(-6.22987742386527,2.64780613061743,37.1747685222393));
#18446=CARTESIAN_POINT('Ctrl Pts',(-6.29348772503758,2.48682553766871,37.1829673106977));
#18447=CARTESIAN_POINT('Ctrl Pts',(-6.37097762342811,2.2907194108222,37.192955052822));
#18448=CARTESIAN_POINT('Ctrl Pts',(-6.43934951496975,2.09085568620677,37.2029427949464));
#18449=CARTESIAN_POINT('Ctrl Pts',(-6.4982789485285,1.88803064252446,37.2129305370707));
#18450=CARTESIAN_POINT('Ctrl Pts',(-6.55421706784962,1.69550119145653,37.2224112918814));
#18451=CARTESIAN_POINT('Ctrl Pts',(-6.60164731541451,1.50030373926963,37.231892046692));
#18452=CARTESIAN_POINT('Ctrl Pts',(-6.6403394713027,1.30314262682923,37.2413728015027));
#18453=CARTESIAN_POINT('Ctrl Pts',(-6.67886840719424,1.10681322395306,37.2508135624507));
#18454=CARTESIAN_POINT('Ctrl Pts',(-6.70873272479008,0.908536806826755,
37.2602543233986));
#18455=CARTESIAN_POINT('Ctrl Pts',(-6.72975228847598,0.709029714294338,
37.2696950843466));
#18456=CARTESIAN_POINT('Ctrl Pts',(-6.75062773480303,0.51089051101398,37.2790711161901));
#18457=CARTESIAN_POINT('Ctrl Pts',(-6.76277921401833,0.311537577722562,
37.2884471480337));
#18458=CARTESIAN_POINT('Ctrl Pts',(-6.7660781861477,0.111691445224431,37.2978231798772));
#18459=CARTESIAN_POINT('Ctrl Pts',(-6.76666425794581,0.0761882103907818,
37.2994888586481));
#18460=CARTESIAN_POINT('Ctrl Pts',(-6.7669710646382,0.040669455310506,37.301154537419));
#18461=CARTESIAN_POINT('Ctrl Pts',(-6.76699804845725,0.00513927774541282,
37.3028202161899));
#18462=CARTESIAN_POINT('Ctrl Pts',(-6.767,8.48442082414717E-13,37.3028202161899));
#18463=CARTESIAN_POINT('Ctrl Pts',(-6.76700000000002,-0.18600724941485,
37.3115697279959));
#18464=CARTESIAN_POINT('Ctrl Pts',(-6.75932637295443,-0.372014355526724,
37.3203192398018));
#18465=CARTESIAN_POINT('Ctrl Pts',(-6.74400518266934,-0.557389537154261,
37.3290687516078));
#18466=CARTESIAN_POINT('Ctrl Pts',(-6.72868405709653,-0.742763935810769,
37.3378182264583));
#18467=CARTESIAN_POINT('Ctrl Pts',(-6.70571545652998,-0.927506129694568,
37.3465677013089));
#18468=CARTESIAN_POINT('Ctrl Pts',(-6.67517739415655,-1.11098863924945,
37.3553171761594));
#18469=CARTESIAN_POINT('Ctrl Pts',(-6.64463945823072,-1.29447038906648,
37.3640666147814));
#18470=CARTESIAN_POINT('Ctrl Pts',(-6.60653217027122,-1.47669218228375,
37.3728160534034));
#18471=CARTESIAN_POINT('Ctrl Pts',(-6.56098496116669,-1.65703510504292,
37.3815654920254));
#18472=CARTESIAN_POINT('Ctrl Pts',(-6.51543793687462,-1.83737729604219,
37.3903148951456));
#18473=CARTESIAN_POINT('Ctrl Pts',(-6.4624511220257,-2.01584035397278,37.3990642982659));
#18474=CARTESIAN_POINT('Ctrl Pts',(-6.40220448416156,-2.19181813638394,
37.4078137013861));
#18475=CARTESIAN_POINT('Ctrl Pts',(-6.34195808575086,-2.36779521936214,
37.4165630697314));
#18476=CARTESIAN_POINT('Ctrl Pts',(-6.27445201489118,-2.54128677545116,
37.4253124380767));
#18477=CARTESIAN_POINT('Ctrl Pts',(-6.19991555136049,-2.71170355238148,
37.434061806422));
#18478=CARTESIAN_POINT('Ctrl Pts',(-6.125379377889,-2.88211966613366,37.442811140719));
#18479=CARTESIAN_POINT('Ctrl Pts',(-6.04381298133475,-3.04946076210725,
37.4515604750161));
#18480=CARTESIAN_POINT('Ctrl Pts',(-5.95549339426162,-3.21315848207122,
37.4603098093131));
#18481=CARTESIAN_POINT('Ctrl Pts',(-5.86717414355011,-3.37685557859897,
37.4690591102887));
#18482=CARTESIAN_POINT('Ctrl Pts',(-5.77210188986082,-3.53690907467566,
37.4778084112642));
#18483=CARTESIAN_POINT('Ctrl Pts',(-5.67059953466907,-3.69277536785153,
37.4865577122398));
#18484=CARTESIAN_POINT('Ctrl Pts',(-5.56909755761611,-3.84864108036016,
37.4953069806205));
#18485=CARTESIAN_POINT('Ctrl Pts',(-5.46116568337923,-4.00031938104478,
37.5040562490013));
#18486=CARTESIAN_POINT('Ctrl Pts',(-5.34717048685978,-4.14729511663394,
37.512805517382));
#18487=CARTESIAN_POINT('Ctrl Pts',(-5.23317570555368,-4.29427031688223,
37.5215547538947));
#18488=CARTESIAN_POINT('Ctrl Pts',(-5.11311782178643,-4.43654275987318,
37.5303039904073));
#18489=CARTESIAN_POINT('Ctrl Pts',(-4.98740459171838,-4.57362924147842,
37.5390532269199));
#18490=CARTESIAN_POINT('Ctrl Pts',(-4.8616918091064,-4.71071523514633,37.547802432291));
#18491=CARTESIAN_POINT('Ctrl Pts',(-4.73032391415227,-4.84261509316724,
37.5565516376622));
#18492=CARTESIAN_POINT('Ctrl Pts',(-4.59374707237074,-4.96888084331726,
37.5653008430333));
#18493=CARTESIAN_POINT('Ctrl Pts',(-4.4571707053716,-5.09514615452937,37.5740500179895));
#18494=CARTESIAN_POINT('Ctrl Pts',(-4.31538563819243,-5.21577720253853,
37.5827991929458));
#18495=CARTESIAN_POINT('Ctrl Pts',(-4.16887341290358,-5.33036429028877,
37.591548367902));
#18496=CARTESIAN_POINT('Ctrl Pts',(-4.02236168477022,-5.44495098921411,
37.6002975131699));
#18497=CARTESIAN_POINT('Ctrl Pts',(-3.87112305634095,-5.55349359239,37.6090466584379));
#18498=CARTESIAN_POINT('Ctrl Pts',(-3.7156711731636,-5.65562346102718,37.6177958037058));
#18499=CARTESIAN_POINT('Ctrl Pts',(-3.56021980456936,-5.75775299158994,
37.626544920012));
#18500=CARTESIAN_POINT('Ctrl Pts',(-3.40055544862031,-5.8534696727556,37.6352940363181));
#18501=CARTESIAN_POINT('Ctrl Pts',(-3.23722036323056,-5.94244842803751,
37.6440431526243));
#18502=CARTESIAN_POINT('Ctrl Pts',(-3.07388580495718,-6.03142689616642,
37.6527922406952));
#18503=CARTESIAN_POINT('Ctrl Pts',(-2.90688079257399,-6.11366734484968,
37.6615413287661));
#18504=CARTESIAN_POINT('Ctrl Pts',(-2.73677251094328,-6.18889046787429,
37.6702904168371));
#18505=CARTESIAN_POINT('Ctrl Pts',(-2.56666476416375,-6.2641133543838,37.6790394773993));
#18506=CARTESIAN_POINT('Ctrl Pts',(-2.39345402971839,-6.33231884350386,
37.6877885379615));
#18507=CARTESIAN_POINT('Ctrl Pts',(-2.21772856473802,-6.39327529621125,
37.6965375985237));
#18508=CARTESIAN_POINT('Ctrl Pts',(-2.04200363768062,-6.45423156232146,
37.7052866323037));
#18509=CARTESIAN_POINT('Ctrl Pts',(-1.86376426619915,-6.50793874252106,
37.7140356660837));
#18510=CARTESIAN_POINT('Ctrl Pts',(-1.6836157819454,-6.55421443796161,37.7227846998637));
#18511=CARTESIAN_POINT('Ctrl Pts',(-1.50346783419716,-6.60048999558714,
37.7315337075879));
#18512=CARTESIAN_POINT('Ctrl Pts',(-1.3214110625709,-6.63933404145526,37.7402827153121));
#18513=CARTESIAN_POINT('Ctrl Pts',(-1.13806375958884,-6.67061465527057,
37.7490317230364));
#18514=CARTESIAN_POINT('Ctrl Pts',(-0.954716987417457,-6.70189517852505,
37.7577807054313));
#18515=CARTESIAN_POINT('Ctrl Pts',(-0.770079973808082,-6.72561226535849,
37.7665296878261));
#18516=CARTESIAN_POINT('Ctrl Pts',(-0.584779770550568,-6.74168536939798,
37.775278670221));
#18517=CARTESIAN_POINT('Ctrl Pts',(-0.391490647552041,-6.75845143942405,
37.7844048508971));
#18518=CARTESIAN_POINT('Ctrl Pts',(-0.197480213102489,-6.76689975924032,
37.7935310315731));
#18519=CARTESIAN_POINT('Ctrl Pts',(-0.00346532629597262,-6.76699911271708,
37.8026572122492));
#18520=CARTESIAN_POINT('Ctrl Pts',(0.184486595297806,-6.76709536139768,
37.8114981997791));
#18521=CARTESIAN_POINT('Ctrl Pts',(0.372442378186903,-6.75935659726761,
37.820339187309));
#18522=CARTESIAN_POINT('Ctrl Pts',(0.559750217723683,-6.74380965729003,
37.829180174839));
#18523=CARTESIAN_POINT('Ctrl Pts',(0.745129914459311,-6.72842275717236,
37.8379301534367));
#18524=CARTESIAN_POINT('Ctrl Pts',(0.929874656315701,-6.70538772273452,
37.8466801320345));
#18525=CARTESIAN_POINT('Ctrl Pts',(1.11335688289925,-6.67478280180718,37.8554301106323));
#18526=CARTESIAN_POINT('Ctrl Pts',(1.29683723118999,-6.64417819417995,37.8641799996572));
#18527=CARTESIAN_POINT('Ctrl Pts',(1.47905480730373,-6.60600390230044,37.8729298886821));
#18528=CARTESIAN_POINT('Ctrl Pts',(1.65939064804941,-6.56038959797101,37.8816797777071));
#18529=CARTESIAN_POINT('Ctrl Pts',(1.83972470264399,-6.51477574543218,37.890429580068));
#18530=CARTESIAN_POINT('Ctrl Pts',(2.01817678125983,-6.46172209820058,37.899179382429));
#18531=CARTESIAN_POINT('Ctrl Pts',(2.19414072347815,-6.40140886723968,37.9079291847899));
#18532=CARTESIAN_POINT('Ctrl Pts',(2.37010298132229,-6.34109621361325,37.9166789033954));
#18533=CARTESIAN_POINT('Ctrl Pts',(2.54357687927041,-6.27352420825919,37.9254286220009));
#18534=CARTESIAN_POINT('Ctrl Pts',(2.71397317790095,-6.19892237325442,37.9341783406064));
#18535=CARTESIAN_POINT('Ctrl Pts',(2.88436790207325,-6.12432122756905,37.9429279783647));
#18536=CARTESIAN_POINT('Ctrl Pts',(3.05168482126381,-6.04269049717354,37.9516776161229));
#18537=CARTESIAN_POINT('Ctrl Pts',(3.21535561997512,-5.95430745234863,37.9604272538812));
#18538=CARTESIAN_POINT('Ctrl Pts',(3.37902496075404,-5.86592519481446,37.9691768137002));
#18539=CARTESIAN_POINT('Ctrl Pts',(3.53904799384998,-5.77079087940157,37.9779263735192));
#18540=CARTESIAN_POINT('Ctrl Pts',(3.69488118815106,-5.66922763746945,37.9866759333382));
#18541=CARTESIAN_POINT('Ctrl Pts',(3.85071304610952,-5.5676652664897,37.9954254181257));
#18542=CARTESIAN_POINT('Ctrl Pts',(4.00235489706083,-5.45967423580629,38.0041749029131));
#18543=CARTESIAN_POINT('Ctrl Pts',(4.14929168607766,-5.34562133936241,38.0129243877005));
#18544=CARTESIAN_POINT('Ctrl Pts',(4.29622726385859,-5.23156938308446,38.0216738003638));
#18545=CARTESIAN_POINT('Ctrl Pts',(4.4384576309216,-5.11145583677121,38.0304232130271));
#18546=CARTESIAN_POINT('Ctrl Pts',(4.57549970661046,-4.98568866204134,38.0391726256904));
#18547=CARTESIAN_POINT('Ctrl Pts',(4.71254069815386,-4.85992248226073,38.0479219691368));
#18548=CARTESIAN_POINT('Ctrl Pts',(4.84439326931412,-4.72850295733903,38.0566713125831));
#18549=CARTESIAN_POINT('Ctrl Pts',(4.97060959434801,-4.5918764422157,38.0654206560294));
#18550=CARTESIAN_POINT('Ctrl Pts',(5.09682496280622,-4.45525096256542,38.0741699331657));
#18551=CARTESIAN_POINT('Ctrl Pts',(5.21740397615949,-4.31341878218193,38.082919210302));
#18552=CARTESIAN_POINT('Ctrl Pts',(5.33193710452046,-4.16686161438534,38.0916684874383));
#18553=CARTESIAN_POINT('Ctrl Pts',(5.44646940289493,-4.02030550864364,38.1004177011713));
#18554=CARTESIAN_POINT('Ctrl Pts',(5.55495572749773,-3.86902470979978,38.1091669149043));
#18555=CARTESIAN_POINT('Ctrl Pts',(5.65702762491562,-3.7135330146562,38.1179161286372));
#18556=CARTESIAN_POINT('Ctrl Pts',(5.75909881655262,-3.55804239466718,38.1266652818733));
#18557=CARTESIAN_POINT('Ctrl Pts',(5.85475551250892,-3.39834117619365,38.1354144351095));
#18558=CARTESIAN_POINT('Ctrl Pts',(5.94367283728205,-3.23497174691767,38.1441635883456));
#18559=CARTESIAN_POINT('Ctrl Pts',(6.03258957676428,-3.07160339300738,38.1529126839911));
#18560=CARTESIAN_POINT('Ctrl Pts',(6.11476689685406,-2.90456712829249,38.1616617796367));
#18561=CARTESIAN_POINT('Ctrl Pts',(6.18992570525385,-2.73443024475622,38.1704108752822));
#18562=CARTESIAN_POINT('Ctrl Pts',(6.26508404388818,-2.56429442462735,38.1791599162432));
#18563=CARTESIAN_POINT('Ctrl Pts',(6.33322384283431,-2.39105828655686,38.1879089572043));
#18564=CARTESIAN_POINT('Ctrl Pts',(6.39411368720143,-2.21531017131763,38.1966579981653));
#18565=CARTESIAN_POINT('Ctrl Pts',(6.45500317120991,-2.03956309619194,38.2054069873477));
#18566=CARTESIAN_POINT('Ctrl Pts',(6.50864269270166,-1.8613043443831,38.2141559765301));
#18567=CARTESIAN_POINT('Ctrl Pts',(6.55485008446417,-1.6811393071962,38.2229049657125));
#18568=CARTESIAN_POINT('Ctrl Pts',(6.60199664749477,-1.49731239211517,38.2318317792419));
#18569=CARTESIAN_POINT('Ctrl Pts',(6.6414056364097,-1.31150116499351,38.2407585927713));
#18570=CARTESIAN_POINT('Ctrl Pts',(6.67293772282226,-1.12436255155342,38.2496854063006));
#18571=CARTESIAN_POINT('Ctrl Pts',(6.70384494949916,-0.940932395048121,
38.2584353204561));
#18572=CARTESIAN_POINT('Ctrl Pts',(6.72718449348967,-0.756227260503447,
38.2671852346117));
#18573=CARTESIAN_POINT('Ctrl Pts',(6.7428770737396,-0.570874564538384,38.2759351487672));
#18574=CARTESIAN_POINT('Ctrl Pts',(6.75856934538689,-0.385525513629147,
38.2846848908512));
#18575=CARTESIAN_POINT('Ctrl Pts',(6.76661493004113,-0.199529212414885,
38.2934346329352));
#18576=CARTESIAN_POINT('Ctrl Pts',(6.76698649908907,-0.0135174385970706,
38.3021843750191));
#18577=CARTESIAN_POINT('Ctrl Pts',(6.76735806132381,0.172490924449114,38.310933956665));
#18578=CARTESIAN_POINT('Ctrl Pts',(6.76005588896272,0.358514472904719,38.3196835383109));
#18579=CARTESIAN_POINT('Ctrl Pts',(6.74510478454558,0.543921359665496,38.3284331199568));
#18580=CARTESIAN_POINT('Ctrl Pts',(6.73015393440652,0.729325093153743,38.3371825527959));
#18581=CARTESIAN_POINT('Ctrl Pts',(6.70755443556852,0.91411190025966,38.3459319856349));
#18582=CARTESIAN_POINT('Ctrl Pts',(6.67738304682264,1.09765415591869,38.354681418474));
#18583=CARTESIAN_POINT('Ctrl Pts',(6.64721213111796,1.28119353391607,38.3634307141353));
#18584=CARTESIAN_POINT('Ctrl Pts',(6.6094696095542,1.4634881167299,38.3721800097966));
#18585=CARTESIAN_POINT('Ctrl Pts',(6.56428366991098,1.64391876348561,38.380929305458));
#18586=CARTESIAN_POINT('Ctrl Pts',(6.51909837867623,1.82434682110053,38.3896784755688));
#18587=CARTESIAN_POINT('Ctrl Pts',(6.46646995271818,2.0029107182078,38.3984276456796));
#18588=CARTESIAN_POINT('Ctrl Pts',(6.40657713281436,2.17900400213036,38.4071768157904));
#18589=CARTESIAN_POINT('Ctrl Pts',(6.34668509278937,2.35509499309989,38.4159258719762));
#18590=CARTESIAN_POINT('Ctrl Pts',(6.27952894037393,2.52871516398452,38.424674928162));
#18591=CARTESIAN_POINT('Ctrl Pts',(6.20533675061305,2.69927486771747,38.4334239843477));
#18592=CARTESIAN_POINT('Ctrl Pts',(6.12832117907774,2.87632521636227,38.44250598563));
#18593=CARTESIAN_POINT('Ctrl Pts',(6.04372366625937,3.05007728920278,38.4515879869123));
#18594=CARTESIAN_POINT('Ctrl Pts',(5.95185378007728,3.21989527478453,38.4606699881945));
#18595=CARTESIAN_POINT('Ctrl Pts',(5.86334450817225,3.38350129287004,38.4694197685017));
#18596=CARTESIAN_POINT('Ctrl Pts',(5.76808562057104,3.54345567125209,38.4781695488088));
#18597=CARTESIAN_POINT('Ctrl Pts',(5.66640068804327,3.6992150846555,38.4869193291159));
#18598=CARTESIAN_POINT('Ctrl Pts',(5.56471941107758,3.85496889852522,38.4956687948694));
#18599=CARTESIAN_POINT('Ctrl Pts',(5.4566127081494,4.00652780919873,38.5044182606229));
#18600=CARTESIAN_POINT('Ctrl Pts',(5.34244776448933,4.15337704569462,38.5131677263764));
#18601=CARTESIAN_POINT('Ctrl Pts',(5.22828631819406,4.30022178356479,38.5219169240959));
#18602=CARTESIAN_POINT('Ctrl Pts',(5.10806717843873,4.44235690972905,38.5306661218156));
#18603=CARTESIAN_POINT('Ctrl Pts',(4.98219864544516,4.57929969070866,38.5394153195352));
#18604=CARTESIAN_POINT('Ctrl Pts',(4.8563332994381,4.71623900430222,38.5481642957254));
#18605=CARTESIAN_POINT('Ctrl Pts',(4.72481904033422,4.84798602483837,38.5569132719156));
#18606=CARTESIAN_POINT('Ctrl Pts',(4.58810250736961,4.97409332259345,38.5656622481059));
#18607=CARTESIAN_POINT('Ctrl Pts',(4.45137708685396,5.1002088182235,38.574411793042));
#18608=CARTESIAN_POINT('Ctrl Pts',(4.30944892635796,5.22068366308144,38.5831613379782));
#18609=CARTESIAN_POINT('Ctrl Pts',(4.16280009466397,5.33510865605056,38.5919108829144));
#18610=CARTESIAN_POINT('Ctrl Pts',(4.01615988348529,5.44952692273083,38.6006599135227));
#18611=CARTESIAN_POINT('Ctrl Pts',(3.86479978231976,5.55789587288803,38.609408944131));
#18612=CARTESIAN_POINT('Ctrl Pts',(3.70923383580818,5.65984746714041,38.6181579747392));
#18613=CARTESIAN_POINT('Ctrl Pts',(3.55366577799287,5.76180044505539,38.6269071240872));
#18614=CARTESIAN_POINT('Ctrl Pts',(3.39389200026583,5.85733573571208,38.6356562734353));
#18615=CARTESIAN_POINT('Ctrl Pts',(3.2304551362578,5.9461288762207,38.6444054227833));
#18616=CARTESIAN_POINT('Ctrl Pts',(3.18695122151406,5.96976399206779,38.6467342868962));
#18617=CARTESIAN_POINT('Ctrl Pts',(3.14318791262581,5.99292165435376,38.6490631510091));
#18618=CARTESIAN_POINT('Ctrl Pts',(3.09917575053265,6.01559628526636,38.651392015122));
#18619=CARTESIAN_POINT('Origin',(0.,0.,-3.69717978381041));
#18620=CARTESIAN_POINT('',(3.09917575053253,6.01559628526642,41.0457515827422));
#18621=CARTESIAN_POINT('',(3.09917575053255,6.01559628526641,40.6512265384361));
#18622=CARTESIAN_POINT('',(3.09917575053259,6.01559628526639,-3.69717978381041));
#18623=CARTESIAN_POINT('',(-6.767,1.16999332856575E-12,39.69717978381));
#18624=CARTESIAN_POINT('Ctrl Pts',(-6.767,1.16999331250164E-12,39.69717978381));
#18625=CARTESIAN_POINT('Ctrl Pts',(-6.76700000000003,-0.186007249414499,
39.705929295616));
#18626=CARTESIAN_POINT('Ctrl Pts',(-6.75932637295445,-0.372014355526342,
39.7146788074219));
#18627=CARTESIAN_POINT('Ctrl Pts',(-6.74400518266938,-0.55738953715385,
39.7234283192278));
#18628=CARTESIAN_POINT('Ctrl Pts',(-6.72868405709659,-0.742763935810203,
39.7321777940784));
#18629=CARTESIAN_POINT('Ctrl Pts',(-6.70571545653008,-0.927506129693848,
39.7409272689289));
#18630=CARTESIAN_POINT('Ctrl Pts',(-6.6751773941567,-1.11098863924858,39.7496767437795));
#18631=CARTESIAN_POINT('Ctrl Pts',(-6.6446394582309,-1.29447038906552,39.7584261824015));
#18632=CARTESIAN_POINT('Ctrl Pts',(-6.60653217027145,-1.47669218228271,
39.7671756210234));
#18633=CARTESIAN_POINT('Ctrl Pts',(-6.56098496116697,-1.65703510504179,
39.7759250596454));
#18634=CARTESIAN_POINT('Ctrl Pts',(-6.51543793687492,-1.83737729604111,
39.7846744627657));
#18635=CARTESIAN_POINT('Ctrl Pts',(-6.46245112202602,-2.01584035397174,
39.7934238658859));
#18636=CARTESIAN_POINT('Ctrl Pts',(-6.40220448416191,-2.19181813638294,
39.8021732690062));
#18637=CARTESIAN_POINT('Ctrl Pts',(-6.34195808575127,-2.36779521936106,
39.8109226373515));
#18638=CARTESIAN_POINT('Ctrl Pts',(-6.27445201489165,-2.54128677545001,
39.8196720056967));
#18639=CARTESIAN_POINT('Ctrl Pts',(-6.19991555136103,-2.71170355238025,
39.828421374042));
#18640=CARTESIAN_POINT('Ctrl Pts',(-6.12537937788953,-2.88211966613253,
39.8371707083391));
#18641=CARTESIAN_POINT('Ctrl Pts',(-6.04381298133527,-3.04946076210623,
39.8459200426361));
#18642=CARTESIAN_POINT('Ctrl Pts',(-5.95549339426212,-3.2131584820703,39.8546693769332));
#18643=CARTESIAN_POINT('Ctrl Pts',(-5.86717414355061,-3.37685557859809,
39.8634186779087));
#18644=CARTESIAN_POINT('Ctrl Pts',(-5.77210188986133,-3.53690907467482,
39.8721679788843));
#18645=CARTESIAN_POINT('Ctrl Pts',(-5.67059953466958,-3.69277536785074,
39.8809172798599));
#18646=CARTESIAN_POINT('Ctrl Pts',(-5.56909755761669,-3.84864108035931,
39.8896665482406));
#18647=CARTESIAN_POINT('Ctrl Pts',(-5.4611656833799,-4.00031938104387,39.8984158166214));
#18648=CARTESIAN_POINT('Ctrl Pts',(-5.34717048686053,-4.14729511663298,
39.9071650850021));
#18649=CARTESIAN_POINT('Ctrl Pts',(-5.23317570555455,-4.29427031688116,
39.9159143215147));
#18650=CARTESIAN_POINT('Ctrl Pts',(-5.11311782178743,-4.43654275987201,
39.9246635580273));
#18651=CARTESIAN_POINT('Ctrl Pts',(-4.98740459171952,-4.57362924147717,
39.93341279454));
#18652=CARTESIAN_POINT('Ctrl Pts',(-4.86169180910768,-4.710715235145,39.9421619999111));
#18653=CARTESIAN_POINT('Ctrl Pts',(-4.7303239141537,-4.84261509316583,39.9509112052822));
#18654=CARTESIAN_POINT('Ctrl Pts',(-4.59374707237233,-4.96888084331579,
39.9596604106533));
#18655=CARTESIAN_POINT('Ctrl Pts',(-4.45717070537335,-5.09514615452783,
39.9684095856095));
#18656=CARTESIAN_POINT('Ctrl Pts',(-4.31538563819435,-5.21577720253694,
39.9771587605658));
#18657=CARTESIAN_POINT('Ctrl Pts',(-4.16887341290566,-5.33036429028714,
39.985907935522));
#18658=CARTESIAN_POINT('Ctrl Pts',(-4.02236168477252,-5.44495098921241,
39.9946570807899));
#18659=CARTESIAN_POINT('Ctrl Pts',(-3.87112305634348,-5.55349359238823,
40.0034062260578));
#18660=CARTESIAN_POINT('Ctrl Pts',(-3.71567117316636,-5.65562346102536,
40.0121553713258));
#18661=CARTESIAN_POINT('Ctrl Pts',(-3.56021980457203,-5.75775299158829,
40.0209044876319));
#18662=CARTESIAN_POINT('Ctrl Pts',(-3.40055544862289,-5.85346967275411,
40.0296536039381));
#18663=CARTESIAN_POINT('Ctrl Pts',(-3.23722036323303,-5.94244842803616,
40.0384027202442));
#18664=CARTESIAN_POINT('Ctrl Pts',(-3.07388580495955,-6.03142689616522,
40.0471518083152));
#18665=CARTESIAN_POINT('Ctrl Pts',(-2.90688079257624,-6.11366734484862,
40.0559008963861));
#18666=CARTESIAN_POINT('Ctrl Pts',(-2.73677251094541,-6.18889046787335,
40.0646499844571));
#18667=CARTESIAN_POINT('Ctrl Pts',(-2.56666476416557,-6.26411335438307,
40.0733990450193));
#18668=CARTESIAN_POINT('Ctrl Pts',(-2.39345402971991,-6.3323188435033,40.0821481055815));
#18669=CARTESIAN_POINT('Ctrl Pts',(-2.21772856473922,-6.39327529621084,
40.0908971661438));
#18670=CARTESIAN_POINT('Ctrl Pts',(-2.04200363768161,-6.45423156232116,
40.0996461999238));
#18671=CARTESIAN_POINT('Ctrl Pts',(-1.86376426619992,-6.50793874252085,
40.1083952337038));
#18672=CARTESIAN_POINT('Ctrl Pts',(-1.68361578194596,-6.55421443796147,
40.1171442674838));
#18673=CARTESIAN_POINT('Ctrl Pts',(-1.50346783419762,-6.60048999558704,
40.125893275208));
#18674=CARTESIAN_POINT('Ctrl Pts',(-1.32141106257128,-6.63933404145519,
40.1346422829322));
#18675=CARTESIAN_POINT('Ctrl Pts',(-1.13806375958912,-6.67061465527052,
40.1433912906565));
#18676=CARTESIAN_POINT('Ctrl Pts',(-0.954716987417324,-6.70189517852508,
40.1521402730514));
#18677=CARTESIAN_POINT('Ctrl Pts',(-0.770079973807532,-6.72561226535856,
40.1608892554463));
#18678=CARTESIAN_POINT('Ctrl Pts',(-0.584779770549598,-6.74168536939807,
40.1696382378412));
#18679=CARTESIAN_POINT('Ctrl Pts',(-0.391490647551099,-6.7584514394241,
40.1787644185172));
#18680=CARTESIAN_POINT('Ctrl Pts',(-0.197480213101576,-6.76689975924034,
40.1878905991933));
#18681=CARTESIAN_POINT('Ctrl Pts',(-0.00346532629509061,-6.76699911271708,
40.1970167798694));
#18682=CARTESIAN_POINT('Ctrl Pts',(0.184486595298722,-6.76709536139766,
40.2058577673993));
#18683=CARTESIAN_POINT('Ctrl Pts',(0.372442378187854,-6.75935659726755,
40.2146987549292));
#18684=CARTESIAN_POINT('Ctrl Pts',(0.559750217724665,-6.74380965728995,
40.2235397424591));
#18685=CARTESIAN_POINT('Ctrl Pts',(0.745129914460262,-6.72842275717225,
40.2322897210569));
#18686=CARTESIAN_POINT('Ctrl Pts',(0.929874656316616,-6.70538772273439,
40.2410396996547));
#18687=CARTESIAN_POINT('Ctrl Pts',(1.11335688290013,-6.67478280180703,40.2497896782524));
#18688=CARTESIAN_POINT('Ctrl Pts',(1.29683723119084,-6.64417819417979,40.2585395672774));
#18689=CARTESIAN_POINT('Ctrl Pts',(1.47905480730455,-6.60600390230026,40.2672894563023));
#18690=CARTESIAN_POINT('Ctrl Pts',(1.6593906480502,-6.56038959797081,40.2760393453272));
#18691=CARTESIAN_POINT('Ctrl Pts',(1.83972470264474,-6.51477574543197,40.2847891476882));
#18692=CARTESIAN_POINT('Ctrl Pts',(2.01817678126054,-6.46172209820035,40.2935389500491));
#18693=CARTESIAN_POINT('Ctrl Pts',(2.19414072347883,-6.40140886723945,40.3022887524101));
#18694=CARTESIAN_POINT('Ctrl Pts',(2.37010298132305,-6.34109621361297,40.3110384710156));
#18695=CARTESIAN_POINT('Ctrl Pts',(2.54357687927126,-6.27352420825885,40.3197881896211));
#18696=CARTESIAN_POINT('Ctrl Pts',(2.71397317790188,-6.19892237325401,40.3285379082266));
#18697=CARTESIAN_POINT('Ctrl Pts',(2.88436790207409,-6.12432122756865,40.3372875459848));
#18698=CARTESIAN_POINT('Ctrl Pts',(3.05168482126455,-6.04269049717317,40.3460371837431));
#18699=CARTESIAN_POINT('Ctrl Pts',(3.21535561997577,-5.95430745234828,40.3547868215013));
#18700=CARTESIAN_POINT('Ctrl Pts',(3.37902496075465,-5.8659251948141,40.3635363813204));
#18701=CARTESIAN_POINT('Ctrl Pts',(3.53904799385056,-5.77079087940121,40.3722859411394));
#18702=CARTESIAN_POINT('Ctrl Pts',(3.69488118815161,-5.66922763746909,40.3810355009584));
#18703=CARTESIAN_POINT('Ctrl Pts',(3.85071304611008,-5.56766526648931,40.3897849857458));
#18704=CARTESIAN_POINT('Ctrl Pts',(4.00235489706141,-5.45967423580587,40.3985344705333));
#18705=CARTESIAN_POINT('Ctrl Pts',(4.14929168607826,-5.34562133936195,40.4072839553207));
#18706=CARTESIAN_POINT('Ctrl Pts',(4.29622726385915,-5.23156938308401,40.416033367984));
#18707=CARTESIAN_POINT('Ctrl Pts',(4.43845763092212,-5.11145583677076,40.4247827806473));
#18708=CARTESIAN_POINT('Ctrl Pts',(4.57549970661095,-4.9856886620409,40.4335321933106));
#18709=CARTESIAN_POINT('Ctrl Pts',(4.71254069815417,-4.85992248226042,40.4422815367569));
#18710=CARTESIAN_POINT('Ctrl Pts',(4.84439326931427,-4.72850295733886,40.4510308802032));
#18711=CARTESIAN_POINT('Ctrl Pts',(4.97060959434801,-4.5918764422157,40.4597802236496));
#18712=CARTESIAN_POINT('Ctrl Pts',(5.09682496280611,-4.45525096256553,40.4685295007858));
#18713=CARTESIAN_POINT('Ctrl Pts',(5.21740397615928,-4.31341878218217,40.4772787779221));
#18714=CARTESIAN_POINT('Ctrl Pts',(5.33193710452017,-4.16686161438571,40.4860280550584));
#18715=CARTESIAN_POINT('Ctrl Pts',(5.44646940289463,-4.02030550864405,40.4947772687914));
#18716=CARTESIAN_POINT('Ctrl Pts',(5.55495572749743,-3.86902470980022,40.5035264825244));
#18717=CARTESIAN_POINT('Ctrl Pts',(5.65702762491531,-3.71353301465667,40.5122756962573));
#18718=CARTESIAN_POINT('Ctrl Pts',(5.75909881655234,-3.55804239466763,40.5210248494934));
#18719=CARTESIAN_POINT('Ctrl Pts',(5.85475551250867,-3.39834117619407,40.5297740027295));
#18720=CARTESIAN_POINT('Ctrl Pts',(5.94367283728183,-3.23497174691808,40.5385231559657));
#18721=CARTESIAN_POINT('Ctrl Pts',(6.03258957676403,-3.07160339300787,40.5472722516112));
#18722=CARTESIAN_POINT('Ctrl Pts',(6.11476689685378,-2.90456712829307,40.5560213472568));
#18723=CARTESIAN_POINT('Ctrl Pts',(6.18992570525356,-2.7344302447569,40.5647704429023));
#18724=CARTESIAN_POINT('Ctrl Pts',(6.26508404388792,-2.56429442462801,40.5735194838633));
#18725=CARTESIAN_POINT('Ctrl Pts',(6.33322384283407,-2.39105828655749,40.5822685248244));
#18726=CARTESIAN_POINT('Ctrl Pts',(6.39411368720122,-2.21531017131823,40.5910175657854));
#18727=CARTESIAN_POINT('Ctrl Pts',(6.45500317120969,-2.03956309619263,40.5997665549678));
#18728=CARTESIAN_POINT('Ctrl Pts',(6.50864269270143,-1.86130434438389,40.6085155441502));
#18729=CARTESIAN_POINT('Ctrl Pts',(6.55485008446394,-1.68113930719709,40.6172645333326));
#18730=CARTESIAN_POINT('Ctrl Pts',(6.60199664749458,-1.49731239211603,40.626191346862));
#18731=CARTESIAN_POINT('Ctrl Pts',(6.64140563640953,-1.31150116499434,40.6351181603913));
#18732=CARTESIAN_POINT('Ctrl Pts',(6.67293772282212,-1.12436255155423,40.6440449739207));
#18733=CARTESIAN_POINT('Ctrl Pts',(6.70384494949903,-0.94093239504902,40.6527948880762));
#18734=CARTESIAN_POINT('Ctrl Pts',(6.72718449348956,-0.756227260504442,
40.6615448022318));
#18735=CARTESIAN_POINT('Ctrl Pts',(6.74287707373951,-0.570874564539475,
40.6702947163873));
#18736=CARTESIAN_POINT('Ctrl Pts',(6.75856934538683,-0.38552551363027,40.6790444584713));
#18737=CARTESIAN_POINT('Ctrl Pts',(6.76661493004109,-0.199529212416038,
40.6877942005552));
#18738=CARTESIAN_POINT('Ctrl Pts',(6.76698649908907,-0.0135174385982532,
40.6965439426392));
#18739=CARTESIAN_POINT('Ctrl Pts',(6.76735806132384,0.172490924447966,40.7052935242851));
#18740=CARTESIAN_POINT('Ctrl Pts',(6.76005588896278,0.358514472903606,40.714043105931));
#18741=CARTESIAN_POINT('Ctrl Pts',(6.74510478454567,0.54392135966442,40.7227926875769));
#18742=CARTESIAN_POINT('Ctrl Pts',(6.73015393440664,0.72932509315264,40.7315421204159));
#18743=CARTESIAN_POINT('Ctrl Pts',(6.70755443556867,0.914111900258532,40.740291553255));
#18744=CARTESIAN_POINT('Ctrl Pts',(6.67738304682283,1.09765415591754,40.749040986094));
#18745=CARTESIAN_POINT('Ctrl Pts',(6.6472121311182,1.28119353391484,40.7577902817554));
#18746=CARTESIAN_POINT('Ctrl Pts',(6.60946960955449,1.46348811672858,40.7665395774167));
#18747=CARTESIAN_POINT('Ctrl Pts',(6.56428366991133,1.64391876348421,40.775288873078));
#18748=CARTESIAN_POINT('Ctrl Pts',(6.51909837867661,1.82434682109917,40.7840380431888));
#18749=CARTESIAN_POINT('Ctrl Pts',(6.46646995271858,2.00291071820648,40.7927872132997));
#18750=CARTESIAN_POINT('Ctrl Pts',(6.4065771328148,2.17900400212908,40.8015363834105));
#18751=CARTESIAN_POINT('Ctrl Pts',(6.34668509278983,2.35509499309866,40.8102854395963));
#18752=CARTESIAN_POINT('Ctrl Pts',(6.27952894037441,2.52871516398333,40.819034495782));
#18753=CARTESIAN_POINT('Ctrl Pts',(6.20533675061354,2.69927486771633,40.8277835519678));
#18754=CARTESIAN_POINT('Ctrl Pts',(6.12832117907822,2.87632521636124,40.8368655532501));
#18755=CARTESIAN_POINT('Ctrl Pts',(6.04372366625984,3.05007728920185,40.8459475545324));
#18756=CARTESIAN_POINT('Ctrl Pts',(5.95185378007773,3.2198952747837,40.8550295558146));
#18757=CARTESIAN_POINT('Ctrl Pts',(5.86334450817268,3.38350129286931,40.8637793361217));
#18758=CARTESIAN_POINT('Ctrl Pts',(5.76808562057143,3.54345567125145,40.8725291164289));
#18759=CARTESIAN_POINT('Ctrl Pts',(5.66640068804362,3.69921508465496,40.881278896736));
#18760=CARTESIAN_POINT('Ctrl Pts',(5.56471941107797,3.85496889852466,40.8900283624895));
#18761=CARTESIAN_POINT('Ctrl Pts',(5.45661270814982,4.00652780919816,40.898777828243));
#18762=CARTESIAN_POINT('Ctrl Pts',(5.34244776448978,4.15337704569404,40.9075272939964));
#18763=CARTESIAN_POINT('Ctrl Pts',(5.22828631819447,4.3002217835643,40.916276491716));
#18764=CARTESIAN_POINT('Ctrl Pts',(5.10806717843909,4.44235690972864,40.9250256894356));
#18765=CARTESIAN_POINT('Ctrl Pts',(4.98219864544546,4.57929969070834,40.9337748871553));
#18766=CARTESIAN_POINT('Ctrl Pts',(4.85633329943826,4.71623900430207,40.9425238633455));
#18767=CARTESIAN_POINT('Ctrl Pts',(4.72481904033422,4.84798602483838,40.9512728395357));
#18768=CARTESIAN_POINT('Ctrl Pts',(4.58810250736944,4.97409332259361,40.960021815726));
#18769=CARTESIAN_POINT('Ctrl Pts',(4.45137708685385,5.1002088182236,40.9687713606622));
#18770=CARTESIAN_POINT('Ctrl Pts',(4.30944892635792,5.22068366308147,40.9775209055984));
#18771=CARTESIAN_POINT('Ctrl Pts',(4.162800094664,5.33510865605054,40.9862704505345));
#18772=CARTESIAN_POINT('Ctrl Pts',(4.01615988348534,5.44952692273078,40.9950194811428));
#18773=CARTESIAN_POINT('Ctrl Pts',(3.86479978231984,5.55789587288798,41.0037685117511));
#18774=CARTESIAN_POINT('Ctrl Pts',(3.70923383580829,5.65984746714034,41.0125175423593));
#18775=CARTESIAN_POINT('Ctrl Pts',(3.5536657779929,5.76180044505538,41.0212666917074));
#18776=CARTESIAN_POINT('Ctrl Pts',(3.39389200026577,5.85733573571212,41.0300158410554));
#18777=CARTESIAN_POINT('Ctrl Pts',(3.23045513625766,5.94612887622078,41.0387649904034));
#18778=CARTESIAN_POINT('Ctrl Pts',(3.18695122151392,5.96976399206787,41.0410938545163));
#18779=CARTESIAN_POINT('Ctrl Pts',(3.14318791262567,5.99292165435383,41.0434227186293));
#18780=CARTESIAN_POINT('Ctrl Pts',(3.09917575053253,6.01559628526642,41.0457515827422));
#18781=CARTESIAN_POINT('Ctrl Pts',(3.09917575053254,6.01559628526642,39.0455765095776));
#18782=CARTESIAN_POINT('Ctrl Pts',(2.94385435927471,6.09561633091081,39.0537889104959));
#18783=CARTESIAN_POINT('Ctrl Pts',(2.78553706128792,6.16956278200781,39.0620013114142));
#18784=CARTESIAN_POINT('Ctrl Pts',(2.62474477414606,6.23722725821282,39.0702137123324));
#18785=CARTESIAN_POINT('Ctrl Pts',(2.46373037286765,6.30498520430357,39.0784374576402));
#18786=CARTESIAN_POINT('Ctrl Pts',(2.30023448502693,6.36644370565575,39.086661202948));
#18787=CARTESIAN_POINT('Ctrl Pts',(2.13479521821867,6.42144363646297,39.0948849482558));
#18788=CARTESIAN_POINT('Ctrl Pts',(1.9768168502074,6.47396320740453,39.1027378231369));
#18789=CARTESIAN_POINT('Ctrl Pts',(1.8170668025288,6.52059390228783,39.110590698018));
#18790=CARTESIAN_POINT('Ctrl Pts',(1.65602197365155,6.56124075330141,39.1184435728991));
#18791=CARTESIAN_POINT('Ctrl Pts',(1.47871771179268,6.60599139798894,39.1270892909515));
#18792=CARTESIAN_POINT('Ctrl Pts',(1.2994398801499,6.64359094358373,39.1357350090038));
#18793=CARTESIAN_POINT('Ctrl Pts',(1.1187787795732,6.67387616324851,39.1443807270562));
#18794=CARTESIAN_POINT('Ctrl Pts',(0.938349611031916,6.70412250286321,39.1530153457685));
#18795=CARTESIAN_POINT('Ctrl Pts',(0.756541014008898,6.72707319072024,39.1616499644808));
#18796=CARTESIAN_POINT('Ctrl Pts',(0.573955540286112,6.74261551905304,39.1702845831931));
#18797=CARTESIAN_POINT('Ctrl Pts',(0.384921856918772,6.75870674204548,39.1792241430956));
#18798=CARTESIAN_POINT('Ctrl Pts',(0.19505572705101,6.76685667977349,39.1881637029981));
#18799=CARTESIAN_POINT('Ctrl Pts',(0.0050371983657768,6.76699812521273,
39.1971032629005));
#18800=CARTESIAN_POINT('Ctrl Pts',(-0.177990118787014,6.76713436655428,
39.205713916171));
#18801=CARTESIAN_POINT('Ctrl Pts',(-0.361158472792682,6.75984085858258,
39.2143245694415));
#18802=CARTESIAN_POINT('Ctrl Pts',(-0.543854620886027,6.74511016598995,
39.2229352227119));
#18803=CARTESIAN_POINT('Ctrl Pts',(-0.726377834852708,6.73039341698335,
39.231537725423));
#18804=CARTESIAN_POINT('Ctrl Pts',(-0.908429431051354,6.70825354324155,
39.2401402281341));
#18805=CARTESIAN_POINT('Ctrl Pts',(-1.08939709403731,6.67873513260581,39.2487427308452));
#18806=CARTESIAN_POINT('Ctrl Pts',(-1.27016108156082,6.64924994434713,39.2573355516126));
#18807=CARTESIAN_POINT('Ctrl Pts',(-1.44984326925202,6.61240283520988,39.26592837238));
#18808=CARTESIAN_POINT('Ctrl Pts',(-1.62783717121543,6.56829012331287,39.2745211931475));
#18809=CARTESIAN_POINT('Ctrl Pts',(-1.6488145610587,6.56309123984383,39.2755338961059));
#18810=CARTESIAN_POINT('Ctrl Pts',(-1.66976850853207,6.55779149843397,39.2765465990642));
#18811=CARTESIAN_POINT('Ctrl Pts',(-1.69069802736641,6.5523911040367,39.2775593020226));
#18812=CARTESIAN_POINT('Ctrl Pts',(-1.86833610740447,6.50655556907902,39.2861545597827));
#18813=CARTESIAN_POINT('Ctrl Pts',(-2.04400450180928,6.45351909298188,39.2947498175428));
#18814=CARTESIAN_POINT('Ctrl Pts',(-2.21712304950587,6.39348530797951,39.3033450753028));
#18815=CARTESIAN_POINT('Ctrl Pts',(-2.39040371538069,6.33339530388341,39.3119483821573));
#18816=CARTESIAN_POINT('Ctrl Pts',(-2.5611294798661,6.26629501151802,39.3205516890117));
#18817=CARTESIAN_POINT('Ctrl Pts',(-2.7287399612937,6.19243629144773,39.3291549958662));
#18818=CARTESIAN_POINT('Ctrl Pts',(-2.903299631403,6.11551536323158,39.3381149988061));
#18819=CARTESIAN_POINT('Ctrl Pts',(-3.07447984919786,6.03126381812536,39.3470750017461));
#18820=CARTESIAN_POINT('Ctrl Pts',(-3.24167696116458,5.94001847467285,39.3560350046861));
#18821=CARTESIAN_POINT('Ctrl Pts',(-3.40265718392653,5.85216590627502,39.3646618478909));
#18822=CARTESIAN_POINT('Ctrl Pts',(-3.55994493731526,5.75783045377207,39.3732886910956));
#18823=CARTESIAN_POINT('Ctrl Pts',(-3.71303159681705,5.65735674684196,39.3819155343004));
#18824=CARTESIAN_POINT('Ctrl Pts',(-3.86626456846748,5.55678701244616,39.3905506225865));
#18825=CARTESIAN_POINT('Ctrl Pts',(-4.01528818196723,5.45006748831492,39.3991857108726));
#18826=CARTESIAN_POINT('Ctrl Pts',(-4.15962561129012,5.33758407651807,39.4078207991588));
#18827=CARTESIAN_POINT('Ctrl Pts',(-4.30417741066163,5.2249336042812,39.4164687122839));
#18828=CARTESIAN_POINT('Ctrl Pts',(-4.44402888199815,5.10650233121538,39.4251166254091));
#18829=CARTESIAN_POINT('Ctrl Pts',(-4.57873775253373,4.98271508251499,39.4337645385342));
#18830=CARTESIAN_POINT('Ctrl Pts',(-4.59385003711008,4.96882803764671,39.4347347027381));
#18831=CARTESIAN_POINT('Ctrl Pts',(-4.60889763973489,4.95487362194797,39.435704866942));
#18832=CARTESIAN_POINT('Ctrl Pts',(-4.62387996649728,4.94085246242236,39.4366750311459));
#18833=CARTESIAN_POINT('Ctrl Pts',(-4.74854157233275,4.82418832274242,39.4447473572604));
#18834=CARTESIAN_POINT('Ctrl Pts',(-4.86898185269501,4.70261880533513,39.4528196833749));
#18835=CARTESIAN_POINT('Ctrl Pts',(-4.98478223331834,4.5764871994133,39.4608920094894));
#18836=CARTESIAN_POINT('Ctrl Pts',(-5.10045796800315,4.45049135981895,39.4689556466629));
#18837=CARTESIAN_POINT('Ctrl Pts',(-5.21150349247123,4.31994347684868,39.4770192838365));
#18838=CARTESIAN_POINT('Ctrl Pts',(-5.3175343112745,4.18522614065458,39.4850829210101));
#18839=CARTESIAN_POINT('Ctrl Pts',(-5.42347421070832,4.05062432196188,39.4931396437713));
#18840=CARTESIAN_POINT('Ctrl Pts',(-5.52440773430764,3.91186045804607,39.5011963665325));
#18841=CARTESIAN_POINT('Ctrl Pts',(-5.61998826768889,3.76935284512331,39.5092530892937));
#18842=CARTESIAN_POINT('Ctrl Pts',(-5.71550638463916,3.62693829316467,39.5173045508174));
#18843=CARTESIAN_POINT('Ctrl Pts',(-5.80567826454077,3.48078516888765,39.5253560123412));
#18844=CARTESIAN_POINT('Ctrl Pts',(-5.89019860143735,3.33134348808788,39.5334074738649));
#18845=CARTESIAN_POINT('Ctrl Pts',(-5.97468943816998,3.18195396697233,39.5414561251842));
#18846=CARTESIAN_POINT('Ctrl Pts',(-6.05353247338711,3.02927849746071,39.5495047765034));
#18847=CARTESIAN_POINT('Ctrl Pts',(-6.1264666303992,2.87379463890605,39.5575534278226));
#18848=CARTESIAN_POINT('Ctrl Pts',(-6.19938975985999,2.718334289312,39.565600862196));
#18849=CARTESIAN_POINT('Ctrl Pts',(-6.26640563102561,2.56006673359669,39.5736482965695));
#18850=CARTESIAN_POINT('Ctrl Pts',(-6.32729996666182,2.39949247381219,39.5816957309429));
#18851=CARTESIAN_POINT('Ctrl Pts',(-6.388197141872,2.23891072626247,39.5897435405776));
#18852=CARTESIAN_POINT('Ctrl Pts',(-6.44297208213749,2.07602240984482,39.5977913502123));
#18853=CARTESIAN_POINT('Ctrl Pts',(-6.49145938811474,1.91134612575982,39.6058391598469));
#18854=CARTESIAN_POINT('Ctrl Pts',(-6.53997991942607,1.74655699926286,39.6138924841449));
#18855=CARTESIAN_POINT('Ctrl Pts',(-6.58220410403456,1.57997781601481,39.6219458084428));
#18856=CARTESIAN_POINT('Ctrl Pts',(-6.61801684346878,1.4121409489012,39.6299991327407));
#18857=CARTESIAN_POINT('Ctrl Pts',(-6.65384226337064,1.24424465461178,39.6380553085356));
#18858=CARTESIAN_POINT('Ctrl Pts',(-6.68325165017052,1.07509015652775,39.6461114843305));
#18859=CARTESIAN_POINT('Ctrl Pts',(-6.70618148458003,0.90521759587185,39.6541676601254));
#18860=CARTESIAN_POINT('Ctrl Pts',(-6.72913758268588,0.735150464192443,
39.6622330634163));
#18861=CARTESIAN_POINT('Ctrl Pts',(-6.74559926635269,0.564363998166427,
39.6702984667071));
#18862=CARTESIAN_POINT('Ctrl Pts',(-6.75555504822545,0.393401817987186,
39.678363869998));
#18863=CARTESIAN_POINT('Ctrl Pts',(-6.76319043194,0.262285863155353,39.6845494664409));
#18864=CARTESIAN_POINT('Ctrl Pts',(-6.76700023386168,0.131066634845332,
39.6907350628838));
#18865=CARTESIAN_POINT('Ctrl Pts',(-6.76699999998923,-1.20737753336487E-5,
39.6969206593267));
#18866=CARTESIAN_POINT('',(-6.76699932393892,-0.00129874070200122,39.3028202161899));
#18867=CARTESIAN_POINT('Ctrl Pts',(3.09917575053265,6.01559628526636,38.651392015122));
#18868=CARTESIAN_POINT('Ctrl Pts',(2.93382384459268,6.10078395293758,38.6601414630345));
#18869=CARTESIAN_POINT('Ctrl Pts',(2.76495772122984,6.17915010267049,38.6688909109469));
#18870=CARTESIAN_POINT('Ctrl Pts',(2.59315093316708,6.25042856433179,38.6776403588593));
#18871=CARTESIAN_POINT('Ctrl Pts',(2.4213455324561,6.32170645041454,38.6863897361193));
#18872=CARTESIAN_POINT('Ctrl Pts',(2.24659977927579,6.38589665313462,38.6951391133793));
#18873=CARTESIAN_POINT('Ctrl Pts',(2.06950718689902,6.44278115439081,38.7038884906393));
#18874=CARTESIAN_POINT('Ctrl Pts',(1.89241596572834,6.49966521519732,38.712637800154));
#18875=CARTESIAN_POINT('Ctrl Pts',(1.71297821457159,6.54924360009556,38.7213871096686));
#18876=CARTESIAN_POINT('Ctrl Pts',(1.53180337335795,6.59134792173568,38.7301364191833));
#18877=CARTESIAN_POINT('Ctrl Pts',(1.35062987477735,6.63345193135314,38.7388856638594));
#18878=CARTESIAN_POINT('Ctrl Pts',(1.16771959102906,6.66808192368246,38.7476349085355));
#18879=CARTESIAN_POINT('Ctrl Pts',(0.983693746906403,6.69512028363175,38.7563841532117));
#18880=CARTESIAN_POINT('Ctrl Pts',(0.799669205419443,6.72215845218872,38.7651333359558));
#18881=CARTESIAN_POINT('Ctrl Pts',(0.614529402873063,6.74160505424583,38.7738825187));
#18882=CARTESIAN_POINT('Ctrl Pts',(0.428903127362849,6.75339404354125,38.7826317014442));
#18883=CARTESIAN_POINT('Ctrl Pts',(0.243278104163518,6.76518295330331,38.7913808251628));
#18884=CARTESIAN_POINT('Ctrl Pts',(0.0571669005387937,6.76931433552276,
38.8001299488814));
#18885=CARTESIAN_POINT('Ctrl Pts',(-0.128798404777798,6.76577415902472,
38.8088790726));
#18886=CARTESIAN_POINT('Ctrl Pts',(-0.314762517259266,6.7622340052344,38.8176281401992));
#18887=CARTESIAN_POINT('Ctrl Pts',(-0.500580446819561,6.75102239665088,
38.8263772077984));
#18888=CARTESIAN_POINT('Ctrl Pts',(-0.685621118842547,6.73217741012498,
38.8351262753976));
#18889=CARTESIAN_POINT('Ctrl Pts',(-0.870660665414616,6.71333253821771,
38.8438752897834));
#18890=CARTESIAN_POINT('Ctrl Pts',(-1.05492267885518,6.68685441030608,38.8526243041692));
#18891=CARTESIAN_POINT('Ctrl Pts',(-1.23778137635303,6.65283295028168,38.861373318555));
#18892=CARTESIAN_POINT('Ctrl Pts',(-1.42999922978899,6.61707018861854,38.8705701289224));
#18893=CARTESIAN_POINT('Ctrl Pts',(-1.62066601233749,6.572971729344,38.8797669392898));
#18894=CARTESIAN_POINT('Ctrl Pts',(-1.80906628500441,6.52070304311279,38.8889637496572));
#18895=CARTESIAN_POINT('Ctrl Pts',(-1.98831342545575,6.47097374915016,38.8977137473949));
#18896=CARTESIAN_POINT('Ctrl Pts',(-2.16550875896742,6.41384933989515,38.9064637451327));
#18897=CARTESIAN_POINT('Ctrl Pts',(-2.34005036714043,6.34952386240464,38.9152137428704));
#18898=CARTESIAN_POINT('Ctrl Pts',(-2.51458843547124,6.28519968948582,38.9239635631513));
#18899=CARTESIAN_POINT('Ctrl Pts',(-2.68647261718093,6.21367483971083,38.9327133834322));
#18900=CARTESIAN_POINT('Ctrl Pts',(-2.85511905908771,6.13519226743825,38.941463203713));
#18901=CARTESIAN_POINT('Ctrl Pts',(-3.02376230488915,6.05671118252921,38.9502128581716));
#18902=CARTESIAN_POINT('Ctrl Pts',(-3.18916767379927,5.9712727599262,38.9589625126301));
#18903=CARTESIAN_POINT('Ctrl Pts',(-3.35077334102802,5.87916720437988,38.9677121670886));
#18904=CARTESIAN_POINT('Ctrl Pts',(-3.51237616037378,5.78706327195637,38.9764616673571));
#18905=CARTESIAN_POINT('Ctrl Pts',(-3.67017916302305,5.68829258362295,38.9852111676255));
#18906=CARTESIAN_POINT('Ctrl Pts',(-3.82364636566463,5.58319061741042,38.9939606678939));
#18907=CARTESIAN_POINT('Ctrl Pts',(-3.97711106778813,5.47809036367691,39.0027100256024));
#18908=CARTESIAN_POINT('Ctrl Pts',(-4.12623987481956,5.36665920043203,39.0114593833108));
#18909=CARTESIAN_POINT('Ctrl Pts',(-4.27052628213971,5.249275595123,39.0202087410193));
#18910=CARTESIAN_POINT('Ctrl Pts',(-4.41481053025004,5.13189374643013,39.0289579677958));
#18911=CARTESIAN_POINT('Ctrl Pts',(-4.55425230136541,5.00855981477343,39.0377071945723));
#18912=CARTESIAN_POINT('Ctrl Pts',(-4.68837800630544,4.8796926819208,39.0464564213488));
#18913=CARTESIAN_POINT('Ctrl Pts',(-4.82250188228895,4.75082730631809,39.0552055288196));
#18914=CARTESIAN_POINT('Ctrl Pts',(-4.95130963052971,4.61642907903521,39.0639546362905));
#18915=CARTESIAN_POINT('Ctrl Pts',(-5.07436379033376,4.4769544473168,39.0727037437613));
#18916=CARTESIAN_POINT('Ctrl Pts',(-5.1974164356282,4.3374815322057,39.0814527435511));
#18917=CARTESIAN_POINT('Ctrl Pts',(-5.31471544462792,4.19293255254566,39.0902017433408));
#18918=CARTESIAN_POINT('Ctrl Pts',(-5.4258624527565,4.04379841779572,39.0989507431306));
#18919=CARTESIAN_POINT('Ctrl Pts',(-5.53702160019171,3.89464799484317,39.1077006984727));
#18920=CARTESIAN_POINT('Ctrl Pts',(-5.64202723081265,3.74091164443829,39.1164506538149));
#18921=CARTESIAN_POINT('Ctrl Pts',(-5.74052265232977,3.58311159163217,39.1252006091571));
#18922=CARTESIAN_POINT('Ctrl Pts',(-5.83901427066932,3.42531763191759,39.1339502266395));
#18923=CARTESIAN_POINT('Ctrl Pts',(-5.93099603115758,3.2634605269558,39.142699844122));
#18924=CARTESIAN_POINT('Ctrl Pts',(-6.01615550622775,3.09809004467035,39.1514494616044));
#18925=CARTESIAN_POINT('Ctrl Pts',(-6.10131214578811,2.93272506863801,39.1601987877555));
#18926=CARTESIAN_POINT('Ctrl Pts',(-6.17964682328752,2.76384720416884,39.1689481139066));
#18927=CARTESIAN_POINT('Ctrl Pts',(-6.25089348288561,2.59203002791599,39.1776974400577));
#18928=CARTESIAN_POINT('Ctrl Pts',(-6.32213814889322,2.42021765937049,39.1864465213892));
#18929=CARTESIAN_POINT('Ctrl Pts',(-6.38629508412572,2.24546640831952,39.1951956027208));
#18930=CARTESIAN_POINT('Ctrl Pts',(-6.44314639819796,2.06836976660091,39.2039446840524));
#18931=CARTESIAN_POINT('Ctrl Pts',(-6.50000285283688,1.89125711158319,39.2126945564868));
#18932=CARTESIAN_POINT('Ctrl Pts',(-6.5495522767324,1.71179891440291,39.2214444289211));
#18933=CARTESIAN_POINT('Ctrl Pts',(-6.59162635926378,1.53060476278461,39.2301943013555));
#18934=CARTESIAN_POINT('Ctrl Pts',(-6.63369752055195,1.34942319164708,39.2389435662781));
#18935=CARTESIAN_POINT('Ctrl Pts',(-6.66829431424256,1.16650618642698,39.2476928312006));
#18936=CARTESIAN_POINT('Ctrl Pts',(-6.69529923745421,0.982474997618313,
39.2564420961231));
#18937=CARTESIAN_POINT('Ctrl Pts',(-6.72230554731447,0.798434359177479,
39.2651918103028));
#18938=CARTESIAN_POINT('Ctrl Pts',(-6.74171916496706,0.613279706240057,
39.2739415244825));
#18939=CARTESIAN_POINT('Ctrl Pts',(-6.75347414817277,0.42763995365508,39.2826912386622));
#18940=CARTESIAN_POINT('Ctrl Pts',(-6.76248837758746,0.285283364198185,
39.2894008978381));
#18941=CARTESIAN_POINT('Ctrl Pts',(-6.76699999999998,0.142641701104637,
39.296110557014));
#18942=CARTESIAN_POINT('Ctrl Pts',(-6.767,9.97351951862395E-13,39.3028202161899));
#18943=CARTESIAN_POINT('Ctrl Pts',(-6.76699633264442,-0.00704513853499345,
39.3028202161899));
#18944=CARTESIAN_POINT('Ctrl Pts',(-6.76678563109908,-0.209428182884763,
39.3123086093829));
#18945=CARTESIAN_POINT('Ctrl Pts',(-6.75749211943877,-0.411404992939795,
39.3217970025758));
#18946=CARTESIAN_POINT('Ctrl Pts',(-6.73924769947695,-0.612233162361049,
39.3312853957688));
#18947=CARTESIAN_POINT('Ctrl Pts',(-6.72089665210696,-0.814235048855196,
39.3408292427814));
#18948=CARTESIAN_POINT('Ctrl Pts',(-6.69348987512733,-1.01507473245287,
39.350373089794));
#18949=CARTESIAN_POINT('Ctrl Pts',(-6.65721041637865,-1.214017492485,39.3599169368065));
#18950=CARTESIAN_POINT('Ctrl Pts',(-6.62065693333061,-1.41446289760368,
39.369532869955));
#18951=CARTESIAN_POINT('Ctrl Pts',(-6.57509630764718,-1.61298251877728,
39.3791488031034));
#18952=CARTESIAN_POINT('Ctrl Pts',(-6.52076377595837,-1.80884736176085,
39.3887647362518));
#18953=CARTESIAN_POINT('Ctrl Pts',(-6.48530923539211,-1.9366584135417,39.3950395863517));
#18954=CARTESIAN_POINT('Ctrl Pts',(-6.44612043584999,-2.06333947643613,
39.4013144364515));
#18955=CARTESIAN_POINT('Ctrl Pts',(-6.40327340508318,-2.18869337728117,
39.4075892865513));
#18956=CARTESIAN_POINT('Ctrl Pts',(-6.3470550497922,-2.35316662102052,39.4158223366834));
#18957=CARTESIAN_POINT('Ctrl Pts',(-6.28441350000255,-2.51571289750371,
39.4240553868154));
#18958=CARTESIAN_POINT('Ctrl Pts',(-6.2154978737592,-2.67579430848018,39.4322884369474));
#18959=CARTESIAN_POINT('Ctrl Pts',(-6.14666431543332,-2.83568508710315,
39.4405116827823));
#18960=CARTESIAN_POINT('Ctrl Pts',(-6.07157169842181,-2.9931165193161,39.4487349286171));
#18961=CARTESIAN_POINT('Ctrl Pts',(-5.99041885552366,-3.14756587466993,
39.456958174452));
#18962=CARTESIAN_POINT('Ctrl Pts',(-5.90934641027032,-3.30186221795454,
39.4651732735655));
#18963=CARTESIAN_POINT('Ctrl Pts',(-5.8222258612897,-3.45318205305921,39.473388372679));
#18964=CARTESIAN_POINT('Ctrl Pts',(-5.72930409986526,-3.60102256744763,
39.4816034717925));
#18965=CARTESIAN_POINT('Ctrl Pts',(-5.63645580371146,-3.74874619701559,
39.4898120759314));
#18966=CARTESIAN_POINT('Ctrl Pts',(-5.53781562029324,-3.89299568302011,
39.4980206800703));
#18967=CARTESIAN_POINT('Ctrl Pts',(-5.43367638296984,-4.03329269520027,
39.5062292842092));
#18968=CARTESIAN_POINT('Ctrl Pts',(-5.3295986488634,-4.17350684987348,39.5144330404582));
#18969=CARTESIAN_POINT('Ctrl Pts',(-5.22002854355738,-4.30977289408286,
39.5226367967072));
#18970=CARTESIAN_POINT('Ctrl Pts',(-5.10530228676486,-4.44164131383361,
39.5308405529561));
#18971=CARTESIAN_POINT('Ctrl Pts',(-4.99060997457976,-4.57347071704301,
39.5390418819204));
#18972=CARTESIAN_POINT('Ctrl Pts',(-4.87076478168693,-4.70090481521211,
39.5472432108847));
#18973=CARTESIAN_POINT('Ctrl Pts',(-4.74614345313542,-4.82352685514031,
39.555444539849));
#18974=CARTESIAN_POINT('Ctrl Pts',(-4.62153931105492,-4.9461319843185,39.5636447377717));
#18975=CARTESIAN_POINT('Ctrl Pts',(-4.49216059990032,-5.06392612520121,
39.5718449356944));
#18976=CARTESIAN_POINT('Ctrl Pts',(-4.35842120621914,-5.17652910637807,
39.5800451336172));
#18977=CARTESIAN_POINT('Ctrl Pts',(-4.22467602017784,-5.28913696448011,
39.588245686697));
#18978=CARTESIAN_POINT('Ctrl Pts',(-4.08657004939793,-5.39655298413444,
39.5964462397769));
#18979=CARTESIAN_POINT('Ctrl Pts',(-3.94455059937957,-5.49843701145464,
39.6046467928567));
#18980=CARTESIAN_POINT('Ctrl Pts',(-3.8024992616789,-5.6003439148351,39.6128491872099));
#18981=CARTESIAN_POINT('Ctrl Pts',(-3.65653298568674,-5.69671614316347,
39.6210515815632));
#18982=CARTESIAN_POINT('Ctrl Pts',(-3.50712844921679,-5.78725660746906,
39.6292539759164));
#18983=CARTESIAN_POINT('Ctrl Pts',(-3.35758419324149,-5.87788174302483,
39.6374640409502));
#18984=CARTESIAN_POINT('Ctrl Pts',(-3.20459555953907,-5.96266403254292,
39.6456741059841));
#18985=CARTESIAN_POINT('Ctrl Pts',(-3.04866507112388,-6.04135169346308,
39.6538841710179));
#18986=CARTESIAN_POINT('Ctrl Pts',(-2.8926599571431,-6.12007701290186,39.6620981652432));
#18987=CARTESIAN_POINT('Ctrl Pts',(-2.73371050698783,-6.19270173934441,
39.6703121594686));
#18988=CARTESIAN_POINT('Ctrl Pts',(-2.57233958649055,-6.25902213223229,
39.6785261536939));
#18989=CARTESIAN_POINT('Ctrl Pts',(-2.41074866368255,-6.3254329419043,39.6867513463291));
#18990=CARTESIAN_POINT('Ctrl Pts',(-2.24673000941149,-6.38552211770407,
39.6949765389643));
#18991=CARTESIAN_POINT('Ctrl Pts',(-2.08082318680931,-6.43913533521674,
39.7032017315995));
#18992=CARTESIAN_POINT('Ctrl Pts',(-1.93162353658767,-6.48734958689539,
39.7105986297193));
#18993=CARTESIAN_POINT('Ctrl Pts',(-1.78089722348275,-6.53032712087692,
39.7179955278392));
#18994=CARTESIAN_POINT('Ctrl Pts',(-1.62904318274137,-6.56799111667821,
39.725392425959));
#18995=CARTESIAN_POINT('Ctrl Pts',(-1.45154649068435,-6.61201519816949,
39.7340383924499));
#18996=CARTESIAN_POINT('Ctrl Pts',(-1.27210607238131,-6.6488791593914,39.7426843589408));
#18997=CARTESIAN_POINT('Ctrl Pts',(-1.0913129970232,-6.67842233933496,39.7513303254317));
#18998=CARTESIAN_POINT('Ctrl Pts',(-0.910751180586849,-6.70792772953506,
39.7599652325561));
#18999=CARTESIAN_POINT('Ctrl Pts',(-0.728840456798993,-6.7301309624288,
39.7686001396804));
#19000=CARTESIAN_POINT('Ctrl Pts',(-0.546183922364777,-6.744921950842,39.7772350468048));
#19001=CARTESIAN_POINT('Ctrl Pts',(-0.357463338412182,-6.76020398813249,
39.7861566258763));
#19002=CARTESIAN_POINT('Ctrl Pts',(-0.167946876348377,-6.76757305659514,
39.7950782049478));
#19003=CARTESIAN_POINT('Ctrl Pts',(0.0216892493982601,-6.76696524126292,
39.8039997840193));
#19004=CARTESIAN_POINT('Ctrl Pts',(0.204724993366466,-6.76637858125239,
39.812610842995));
#19005=CARTESIAN_POINT('Ctrl Pts',(0.387871866214309,-6.75836091852008,
39.8212219019707));
#19006=CARTESIAN_POINT('Ctrl Pts',(0.570516541991954,-6.74290737555497,
39.8298329609464));
#19007=CARTESIAN_POINT('Ctrl Pts',(0.752988975408527,-6.72746840599429,
39.838435899296));
#19008=CARTESIAN_POINT('Ctrl Pts',(0.934959853108263,-6.70460756267172,
39.8470388376455));
#19009=CARTESIAN_POINT('Ctrl Pts',(1.11581699663422,-6.6743719876871,39.8556417759951));
#19010=CARTESIAN_POINT('Ctrl Pts',(1.29647162199824,-6.64417026955187,39.8642350810438));
#19011=CARTESIAN_POINT('Ctrl Pts',(1.47601470102438,-6.60661034439889,39.8728283860926));
#19012=CARTESIAN_POINT('Ctrl Pts',(1.65384009905333,-6.56179106088904,39.8814216911414));
#19013=CARTESIAN_POINT('Ctrl Pts',(1.67365275909974,-6.55679745908892,39.8823791259819));
#19014=CARTESIAN_POINT('Ctrl Pts',(1.69344410338551,-6.55171379529251,39.8833365608225));
#19015=CARTESIAN_POINT('Ctrl Pts',(1.71321329922587,-6.54654024591277,39.884293995663));
#19016=CARTESIAN_POINT('Ctrl Pts',(1.8906992305479,-6.50009261914438,39.8928897532106));
#19017=CARTESIAN_POINT('Ctrl Pts',(2.06619101226672,-6.44645022952148,39.9014855107581));
#19018=CARTESIAN_POINT('Ctrl Pts',(2.23910910938076,-6.38581861598716,39.9100812683057));
#19019=CARTESIAN_POINT('Ctrl Pts',(2.41218854495864,-6.32513043109592,39.9186850459873));
#19020=CARTESIAN_POINT('Ctrl Pts',(2.58268921467238,-6.25744010679457,39.9272888236689));
#19021=CARTESIAN_POINT('Ctrl Pts',(2.75005151816753,-6.18300134622535,39.9358926013506));
#19022=CARTESIAN_POINT('Ctrl Pts',(2.92399130653878,-6.10563707727332,39.9448345150186));
#19023=CARTESIAN_POINT('Ctrl Pts',(3.09454072032255,-6.02098337137873,39.9537764286866));
#19024=CARTESIAN_POINT('Ctrl Pts',(3.26110085699704,-5.92937688129985,39.9627183423546));
#19025=CARTESIAN_POINT('Ctrl Pts',(3.4217988968878,-5.84099448866459,39.9713455446853));
#19026=CARTESIAN_POINT('Ctrl Pts',(3.57878345104977,-5.74614057350822,39.979972747016));
#19027=CARTESIAN_POINT('Ctrl Pts',(3.73154691430984,-5.64516134634828,39.9885999493467));
#19028=CARTESIAN_POINT('Ctrl Pts',(3.88445586138645,-5.54408595193051,39.9972353677672));
#19029=CARTESIAN_POINT('Ctrl Pts',(4.03313544439508,-5.43687377724324,40.0058707861876));
#19030=CARTESIAN_POINT('Ctrl Pts',(4.17710997963996,-5.32391220983144,40.0145062046081));
#19031=CARTESIAN_POINT('Ctrl Pts',(4.3212972167531,-5.21078375779389,40.0231543806292));
#19032=CARTESIAN_POINT('Ctrl Pts',(4.46076528075879,-5.09188913384303,40.0318025566503));
#19033=CARTESIAN_POINT('Ctrl Pts',(4.59507316255803,-4.96765454019691,40.0404507326715));
#19034=CARTESIAN_POINT('Ctrl Pts',(4.60928242719726,-4.95451099124939,40.0413656769032));
#19035=CARTESIAN_POINT('Ctrl Pts',(4.62343397034782,-4.94130770519692,40.042280621135));
#19036=CARTESIAN_POINT('Ctrl Pts',(4.6375272953042,-4.92804520934098,40.0431955653667));
#19037=CARTESIAN_POINT('Ctrl Pts',(4.76423620493021,-4.80880603802919,40.0514215579081));
#19038=CARTESIAN_POINT('Ctrl Pts',(4.88650968612764,-4.6845203573194,40.0596475504494));
#19039=CARTESIAN_POINT('Ctrl Pts',(5.00392275384399,-4.55555112731296,40.0678735429908));
#19040=CARTESIAN_POINT('Ctrl Pts',(5.12121272913508,-4.42671710487426,40.0760909116422));
#19041=CARTESIAN_POINT('Ctrl Pts',(5.2336521987825,-4.29320957372223,40.0843082802936));
#19042=CARTESIAN_POINT('Ctrl Pts',(5.34085104333207,-4.15543007797493,40.092525648945));
#19043=CARTESIAN_POINT('Ctrl Pts',(5.44795895377338,-4.01776745714017,40.1007360470074));
#19044=CARTESIAN_POINT('Ctrl Pts',(5.5498348741313,-3.87584037018802,40.1089464450698));
#19045=CARTESIAN_POINT('Ctrl Pts',(5.64612714378422,-3.73008542478896,40.1171568431322));
#19046=CARTESIAN_POINT('Ctrl Pts',(5.74235699334489,-3.58442496295718,40.1253619189209));
#19047=CARTESIAN_POINT('Ctrl Pts',(5.83301020523841,-3.43494188323044,40.1335669947097));
#19048=CARTESIAN_POINT('Ctrl Pts',(5.91777680708612,-3.28210399919224,40.1417720704985));
#19049=CARTESIAN_POINT('Ctrl Pts',(6.00250541339887,-3.12933462276243,40.149973468468));
#19050=CARTESIAN_POINT('Ctrl Pts',(6.0813524931119,-2.97321375059752,40.1581748664374));
#19051=CARTESIAN_POINT('Ctrl Pts',(6.15405259617078,-2.81423624515847,40.1663762644069));
#19052=CARTESIAN_POINT('Ctrl Pts',(6.22674700475229,-2.65527119216133,40.1745770199746));
#19053=CARTESIAN_POINT('Ctrl Pts',(6.29329523892015,-2.49345027353249,40.1827777755423));
#19054=CARTESIAN_POINT('Ctrl Pts',(6.3534786747419,-2.32929125048801,40.19097853111));
#19055=CARTESIAN_POINT('Ctrl Pts',(6.41366180486043,-2.16513306129323,40.1991792450218));
#19056=CARTESIAN_POINT('Ctrl Pts',(6.46748007667239,-1.99863712744613,40.2073799589336));
#19057=CARTESIAN_POINT('Ctrl Pts',(6.51476377714247,-1.8303392931455,40.2155806728454));
#19058=CARTESIAN_POINT('Ctrl Pts',(6.56205580641776,-1.66201181395955,40.223782831275));
#19059=CARTESIAN_POINT('Ctrl Pts',(6.60281087417786,-1.49188214698168,40.2319849897046));
#19060=CARTESIAN_POINT('Ctrl Pts',(6.63690970038484,-1.32049938619359,40.2401871481342));
#19061=CARTESIAN_POINT('Ctrl Pts',(6.67102071256402,-1.14905537797291,40.2483922377871));
#19062=CARTESIAN_POINT('Ctrl Pts',(6.69847067468287,-0.976357735117145,
40.25659732744));
#19063=CARTESIAN_POINT('Ctrl Pts',(6.71919177212339,-0.802963840673674,
40.264802417093));
#19064=CARTESIAN_POINT('Ctrl Pts',(6.73993654096788,-0.629371864206111,
40.2730168800907));
#19065=CARTESIAN_POINT('Ctrl Pts',(6.75393704542791,-0.455082403312534,
40.2812313430885));
#19066=CARTESIAN_POINT('Ctrl Pts',(6.76117745574585,-0.280657107364366,
40.2894458060863));
#19067=CARTESIAN_POINT('Ctrl Pts',(6.76842215577805,-0.10612846994128,40.2976651358938));
#19068=CARTESIAN_POINT('Ctrl Pts',(6.76889877690449,0.0685358051907464,
40.3058844657012));
#19069=CARTESIAN_POINT('Ctrl Pts',(6.76264362239255,0.242776103670322,40.3141037955087));
#19070=CARTESIAN_POINT('Ctrl Pts',(6.75637877589794,0.41728637692849,40.3223358606694));
#19071=CARTESIAN_POINT('Ctrl Pts',(6.74336133630555,0.591371003614929,40.3305679258301));
#19072=CARTESIAN_POINT('Ctrl Pts',(6.7236794379904,0.764476170423357,40.3387999909908));
#19073=CARTESIAN_POINT('Ctrl Pts',(6.7059879345467,0.920075523985483,40.346199562252));
#19074=CARTESIAN_POINT('Ctrl Pts',(6.68291247249063,1.07488344052355,40.3535991335132));
#19075=CARTESIAN_POINT('Ctrl Pts',(6.65455179220865,1.22850699827582,40.3609987047744));
#19076=CARTESIAN_POINT('Ctrl Pts',(6.62329196254614,1.39783460959325,40.3691546916866));
#19077=CARTESIAN_POINT('Ctrl Pts',(6.58551401471038,1.56624452008607,40.3773106785988));
#19078=CARTESIAN_POINT('Ctrl Pts',(6.5412795957629,1.73319077139706,40.385466665511));
#19079=CARTESIAN_POINT('Ctrl Pts',(6.49709959192488,1.89993165325244,40.3936126193103));
#19080=CARTESIAN_POINT('Ctrl Pts',(6.44647902008466,2.06521211056929,40.4017585731096));
#19081=CARTESIAN_POINT('Ctrl Pts',(6.38953102028647,2.22849328937669,40.4099045269089));
#19082=CARTESIAN_POINT('Ctrl Pts',(6.33264109914247,2.39160794519551,40.4180421730234));
#19083=CARTESIAN_POINT('Ctrl Pts',(6.26943671711267,2.55272703933819,40.4261798191378));
#19084=CARTESIAN_POINT('Ctrl Pts',(6.20008160138574,2.71132387149857,40.4343174652523));
#19085=CARTESIAN_POINT('Ctrl Pts',(6.13078264161349,2.86979228982207,40.4424485224182));
#19086=CARTESIAN_POINT('Ctrl Pts',(6.05534301075599,3.02574217942287,40.4505795795842));
#19087=CARTESIAN_POINT('Ctrl Pts',(5.97397561401119,3.17866392737573,40.4587106367501));
#19088=CARTESIAN_POINT('Ctrl Pts',(5.89265719347881,3.33149362951771,40.4668367997152));
#19089=CARTESIAN_POINT('Ctrl Pts',(5.80541828473356,3.4812984983562,40.4749629626803));
#19090=CARTESIAN_POINT('Ctrl Pts',(5.71251907108747,3.62759077935508,40.4830891256454));
#19091=CARTESIAN_POINT('Ctrl Pts',(5.61964970089293,3.77383606462138,40.4912126781175));
#19092=CARTESIAN_POINT('Ctrl Pts',(5.52112384099072,3.91657069984591,40.4993362305895));
#19093=CARTESIAN_POINT('Ctrl Pts',(5.4172466508149,4.0553332445355,40.5074597830616));
#19094=CARTESIAN_POINT('Ctrl Pts',(5.31338306991627,4.19407760950795,40.5155822712415));
#19095=CARTESIAN_POINT('Ctrl Pts',(5.20416977378661,4.32885062745309,40.5237047594214));
#19096=CARTESIAN_POINT('Ctrl Pts',(5.08995408415236,4.45922150394222,40.5318272476013));
#19097=CARTESIAN_POINT('Ctrl Pts',(4.97573163057727,4.58960010109476,40.5399502168012));
#19098=CARTESIAN_POINT('Ctrl Pts',(4.85650643522585,4.7155757632107,40.5480731860011));
#19099=CARTESIAN_POINT('Ctrl Pts',(4.73266474162749,4.83675236531249,40.556196155201));
#19100=CARTESIAN_POINT('Ctrl Pts',(4.60873588189369,4.95801425772165,40.5643248417632));
#19101=CARTESIAN_POINT('Ctrl Pts',(4.48018429332503,5.0744700849674,40.5724535283254));
#19102=CARTESIAN_POINT('Ctrl Pts',(4.34743209048359,5.1857615852094,40.5805822148876));
#19103=CARTESIAN_POINT('Ctrl Pts',(4.214633173298,5.29709224796119,40.5887137618639));
#19104=CARTESIAN_POINT('Ctrl Pts',(4.07763098363975,5.40325473622688,40.5968453088401));
#19105=CARTESIAN_POINT('Ctrl Pts',(3.93687887216083,5.50393257098356,40.6049768558163));
#19106=CARTESIAN_POINT('Ctrl Pts',(3.79596064724308,5.60472922414495,40.613117999517));
#19107=CARTESIAN_POINT('Ctrl Pts',(3.65128396189943,5.70002808697505,40.6212591432177));
#19108=CARTESIAN_POINT('Ctrl Pts',(3.50333000523339,5.78955679430053,40.6294002869184));
#19109=CARTESIAN_POINT('Ctrl Pts',(3.37110942337792,5.86956504850397,40.636675704091));
#19110=CARTESIAN_POINT('Ctrl Pts',(3.23627203569165,5.94496563415476,40.6439511212635));
#19111=CARTESIAN_POINT('Ctrl Pts',(3.09917575053255,6.01559628526641,40.6512265384361));
#19112=CARTESIAN_POINT('Origin',(0.,0.,-3.69717978381041));
#19113=CARTESIAN_POINT('',(3.09917575053267,6.01559628526634,43.0458827467338));
#19114=CARTESIAN_POINT('',(3.09917575053259,6.01559628526639,42.6516693621546));
#19115=CARTESIAN_POINT('',(3.09917575053259,6.01559628526639,-3.69717978381041));
#19116=CARTESIAN_POINT('',(-6.76699999999432,8.76508570167211E-6,41.6973687769752));
#19117=CARTESIAN_POINT('Ctrl Pts',(-6.76699999999432,8.76508570167208E-6,
41.6973687769752));
#19118=CARTESIAN_POINT('Ctrl Pts',(-6.76700022316934,-0.172291357653503,
41.7055020235368));
#19119=CARTESIAN_POINT('Ctrl Pts',(-6.76041552196173,-0.344817324618494,
41.7136352700984));
#19120=CARTESIAN_POINT('Ctrl Pts',(-6.74722008764693,-0.517020395007585,
41.72176851666));
#19121=CARTESIAN_POINT('Ctrl Pts',(-6.73403694439764,-0.68906306452083,
41.7298941873992));
#19122=CARTESIAN_POINT('Ctrl Pts',(-6.71425535454535,-0.860783072876566,
41.7380198581384));
#19123=CARTESIAN_POINT('Ctrl Pts',(-6.68790153363355,-1.03163078493329,
41.7461455288777));
#19124=CARTESIAN_POINT('Ctrl Pts',(-6.66156668084154,-1.2023555296268,41.7542653511786));
#19125=CARTESIAN_POINT('Ctrl Pts',(-6.62866907138239,-1.37220886699804,
41.7623851734795));
#19126=CARTESIAN_POINT('Ctrl Pts',(-6.58928681335984,-1.54064541387114,
41.7705049957804));
#19127=CARTESIAN_POINT('Ctrl Pts',(-6.54992456624683,-1.70899637478059,
41.7786206922379));
#19128=CARTESIAN_POINT('Ctrl Pts',(-6.50408431591424,-1.87593162239383,
41.7867363886954));
#19129=CARTESIAN_POINT('Ctrl Pts',(-6.45189541292007,-2.04091513315496,
41.7948520851529));
#19130=CARTESIAN_POINT('Ctrl Pts',(-6.39971417545145,-2.20587441107646,
41.8029665895739));
#19131=CARTESIAN_POINT('Ctrl Pts',(-6.34118624531644,-2.36888217105438,
41.8110810939949));
#19132=CARTESIAN_POINT('Ctrl Pts',(-6.27649113796564,-2.52941653253053,
41.8191955984159));
#19133=CARTESIAN_POINT('Ctrl Pts',(-6.21179847389791,-2.68994483124702,
41.8273097963835));
#19134=CARTESIAN_POINT('Ctrl Pts',(-6.14093923265554,-2.84799957658851,
41.8354239943512));
#19135=CARTESIAN_POINT('Ctrl Pts',(-6.06414141080024,-3.00307807920768,
41.8435381923188));
#19136=CARTESIAN_POINT('Ctrl Pts',(-5.98733176980108,-3.15818044832578,
41.8516536390572));
#19137=CARTESIAN_POINT('Ctrl Pts',(-5.90458189114834,-3.31030533361942,
41.8597690857956));
#19138=CARTESIAN_POINT('Ctrl Pts',(-5.81616610487774,-3.45897395776137,
41.867884532534));
#19139=CARTESIAN_POINT('Ctrl Pts',(-5.72771976377007,-3.60769395899081,
41.8760027838185));
#19140=CARTESIAN_POINT('Ctrl Pts',(-5.63360380397292,-3.75295500559633,
41.884121035103));
#19141=CARTESIAN_POINT('Ctrl Pts',(-5.53413627041377,-3.89430670857995,
41.8922392863876));
#19142=CARTESIAN_POINT('Ctrl Pts',(-5.43455819379238,-4.03581550252121,
41.9003665598759));
#19143=CARTESIAN_POINT('Ctrl Pts',(-5.32961687635012,-4.17340597521397,
41.9084938333642));
#19144=CARTESIAN_POINT('Ctrl Pts',(-5.21967164507103,-4.30665960085557,
41.9166211068525));
#19145=CARTESIAN_POINT('Ctrl Pts',(-5.10966031301768,-4.4399933406388,41.9247532665834));
#19146=CARTESIAN_POINT('Ctrl Pts',(-4.99463931697718,-4.56898476535065,
41.9328854263143));
#19147=CARTESIAN_POINT('Ctrl Pts',(-4.87500509432254,-4.69325199944871,
41.9410175860452));
#19148=CARTESIAN_POINT('Ctrl Pts',(-4.7551935351311,-4.8177034377021,41.9491618002619));
#19149=CARTESIAN_POINT('Ctrl Pts',(-4.63075535388932,-4.93741644373681,
41.9573060144786));
#19150=CARTESIAN_POINT('Ctrl Pts',(-4.5021211123992,-5.05204854383738,41.9654502286954));
#19151=CARTESIAN_POINT('Ctrl Pts',(-4.41221603767525,-5.13216723856375,
41.971142384837));
#19152=CARTESIAN_POINT('Ctrl Pts',(-4.32026191353386,-5.2098048226097,41.9768345409787));
#19153=CARTESIAN_POINT('Ctrl Pts',(-4.22641390799836,-5.28485709156625,
41.9825266971203));
#19154=CARTESIAN_POINT('Ctrl Pts',(-4.09197864337153,-5.39236786476217,
41.990680589287));
#19155=CARTESIAN_POINT('Ctrl Pts',(-3.95321822543893,-5.49492178816961,
41.9988344814538));
#19156=CARTESIAN_POINT('Ctrl Pts',(-3.81053623764059,-5.59214650931357,
42.0069883736205));
#19157=CARTESIAN_POINT('Ctrl Pts',(-3.66802836173056,-5.68925258913461,
42.0151323157607));
#19158=CARTESIAN_POINT('Ctrl Pts',(-3.52160874027091,-5.78104220769026,
42.0232762579009));
#19159=CARTESIAN_POINT('Ctrl Pts',(-3.37171526295274,-5.8671820481021,42.0314202000411));
#19160=CARTESIAN_POINT('Ctrl Pts',(-3.2219731479675,-5.95323490456083,42.039555918434));
#19161=CARTESIAN_POINT('Ctrl Pts',(-3.06876447530341,-6.03364915987303,
42.0476916368269));
#19162=CARTESIAN_POINT('Ctrl Pts',(-2.9125574550802,-6.10813376334022,42.0558273552198));
#19163=CARTESIAN_POINT('Ctrl Pts',(-2.75647531441785,-6.18255882015863,
42.06395656952));
#19164=CARTESIAN_POINT('Ctrl Pts',(-2.59739992743273,-6.25106350723082,
42.0720857838202));
#19165=CARTESIAN_POINT('Ctrl Pts',(-2.43582553294712,-6.31340185423381,
42.0802149981204));
#19166=CARTESIAN_POINT('Ctrl Pts',(-2.27434633594233,-6.37570347231318,
42.0883394227958));
#19167=CARTESIAN_POINT('Ctrl Pts',(-2.11037140391,-6.43184585425817,42.0964638474712));
#19168=CARTESIAN_POINT('Ctrl Pts',(-1.94441645063388,-6.48163047901563,
42.1045882721466));
#19169=CARTESIAN_POINT('Ctrl Pts',(-1.77745404455236,-6.53171732831587,
42.1127620172808));
#19170=CARTESIAN_POINT('Ctrl Pts',(-1.60848783736744,-6.57536881497801,
42.120935762415));
#19171=CARTESIAN_POINT('Ctrl Pts',(-1.43806066745962,-6.61243302549868,
42.1291095075492));
#19172=CARTESIAN_POINT('Ctrl Pts',(-1.26872486327763,-6.64925988766087,
42.1372309104114));
#19173=CARTESIAN_POINT('Ctrl Pts',(-1.09794711950863,-6.67958353688564,
42.1453523132735));
#19174=CARTESIAN_POINT('Ctrl Pts',(-0.926271973831232,-6.70330584342493,
42.1534737161357));
#19175=CARTESIAN_POINT('Ctrl Pts',(-0.754583555135203,-6.7270299840481,
42.161595746902));
#19176=CARTESIAN_POINT('Ctrl Pts',(-0.581997958867696,-6.74415171520996,
42.1697177776682));
#19177=CARTESIAN_POINT('Ctrl Pts',(-0.40906646848288,-6.75462461017361,
42.1778398084345));
#19178=CARTESIAN_POINT('Ctrl Pts',(-0.236088677797123,-6.76510030912736,
42.1859640137756));
#19179=CARTESIAN_POINT('Ctrl Pts',(-0.0627651737578177,-6.76892360518161,
42.1940882191167));
#19180=CARTESIAN_POINT('Ctrl Pts',(0.110351168858707,-6.76610017805911,
42.2022124244578));
#19181=CARTESIAN_POINT('Ctrl Pts',(0.285341376097719,-6.76324618929166,
42.2104245687003));
#19182=CARTESIAN_POINT('Ctrl Pts',(0.460119527330116,-6.7536007497577,42.2186367129428));
#19183=CARTESIAN_POINT('Ctrl Pts',(0.634119112966488,-6.73722360847334,
42.2268488571852));
#19184=CARTESIAN_POINT('Ctrl Pts',(0.806530274157802,-6.72099597243902,
42.2349860336017));
#19185=CARTESIAN_POINT('Ctrl Pts',(0.978176671386174,-6.69815913995813,
42.2431232100181));
#19186=CARTESIAN_POINT('Ctrl Pts',(1.14851704837981,-6.66882280388233,42.2512603864346));
#19187=CARTESIAN_POINT('Ctrl Pts',(1.32121144483127,-6.6390810542037,42.25951001459));
#19188=CARTESIAN_POINT('Ctrl Pts',(1.49256307573794,-6.60265892719256,42.2677596427455));
#19189=CARTESIAN_POINT('Ctrl Pts',(1.66202383692403,-6.55972299457045,42.276009270901));
#19190=CARTESIAN_POINT('Ctrl Pts',(1.83148459811012,-6.51678706194835,42.2842588990564));
#19191=CARTESIAN_POINT('Ctrl Pts',(1.99905413843699,-6.46733749329357,42.2925085272119));
#19192=CARTESIAN_POINT('Ctrl Pts',(2.16420575846851,-6.41159125607768,42.3007581553673));
#19193=CARTESIAN_POINT('Ctrl Pts',(2.32886169154851,-6.35601233591493,42.308983023045));
#19194=CARTESIAN_POINT('Ctrl Pts',(2.49160642798038,-6.2940085238898,42.3172078907226));
#19195=CARTESIAN_POINT('Ctrl Pts',(2.65190242788229,-6.22572907481461,42.3254327584002));
#19196=CARTESIAN_POINT('Ctrl Pts',(2.81201783639852,-6.15752655018127,42.3336483598437));
#19197=CARTESIAN_POINT('Ctrl Pts',(2.96968967474599,-6.08306260639842,42.3418639612873));
#19198=CARTESIAN_POINT('Ctrl Pts',(3.12439564138987,-6.00253620364459,42.3500795627308));
#19199=CARTESIAN_POINT('Ctrl Pts',(3.2789583979792,-5.92208434352658,42.358287559059));
#19200=CARTESIAN_POINT('Ctrl Pts',(3.4305604343155,-5.83558136539181,42.3664955553871));
#19201=CARTESIAN_POINT('Ctrl Pts',(3.57869944091381,-5.74327426748916,42.3747035517153));
#19202=CARTESIAN_POINT('Ctrl Pts',(3.72673107092835,-5.65103407715568,42.3829055985867));
#19203=CARTESIAN_POINT('Ctrl Pts',(3.87130436765057,-5.55299833564588,42.3911076454582));
#19204=CARTESIAN_POINT('Ctrl Pts',(4.0119415802419,-5.44945995092414,42.3993096923296));
#19205=CARTESIAN_POINT('Ctrl Pts',(4.15250509503649,-5.34597582318526,42.4075074411012));
#19206=CARTESIAN_POINT('Ctrl Pts',(4.28913634652938,-5.23699500890228,42.4157051898728));
#19207=CARTESIAN_POINT('Ctrl Pts',(4.42138647724192,-5.12285375731753,42.4239029386444));
#19208=CARTESIAN_POINT('Ctrl Pts',(4.5536113838977,-5.00873427588448,42.43209912386));
#19209=CARTESIAN_POINT('Ctrl Pts',(4.68145655881384,-4.88945654711756,42.4402953090756));
#19210=CARTESIAN_POINT('Ctrl Pts',(4.80450593516675,-4.76539733064804,42.4484914942913));
#19211=CARTESIAN_POINT('Ctrl Pts',(4.92754620860461,-4.64134729179927,42.4566870731716));
#19212=CARTESIAN_POINT('Ctrl Pts',(5.04579113671474,-4.51251672382981,42.464882652052));
#19213=CARTESIAN_POINT('Ctrl Pts',(5.15886131848055,-4.37931945588411,42.4730782309323));
#19214=CARTESIAN_POINT('Ctrl Pts',(5.27194370735004,-4.24610780790617,42.4812746946108));
#19215=CARTESIAN_POINT('Ctrl Pts',(5.37985000457132,-4.10852879433005,42.4894711582892));
#19216=CARTESIAN_POINT('Ctrl Pts',(5.48224090557458,-3.96702957554451,42.4976676219677));
#19217=CARTESIAN_POINT('Ctrl Pts',(5.58466148963133,-3.82548933623039,42.5058664617954));
#19218=CARTESIAN_POINT('Ctrl Pts',(5.6815632823423,-3.68002691864602,42.5140653016232));
#19219=CARTESIAN_POINT('Ctrl Pts',(5.77265011563406,-3.53111875224695,42.5222641414509));
#19220=CARTESIAN_POINT('Ctrl Pts',(5.86383209171485,-3.38205504703128,42.5304715452002));
#19221=CARTESIAN_POINT('Ctrl Pts',(5.94918678604182,-3.2295387088168,42.5386789489494));
#19222=CARTESIAN_POINT('Ctrl Pts',(6.02846336904168,-3.07407195883939,42.5468863526987));
#19223=CARTESIAN_POINT('Ctrl Pts',(6.10778241677463,-2.91852193264355,42.5550981527677));
#19224=CARTESIAN_POINT('Ctrl Pts',(6.18101671238073,-2.76001866955657,42.5633099528367));
#19225=CARTESIAN_POINT('Ctrl Pts',(6.24796353223583,-2.59908458882184,42.5715217529057));
#19226=CARTESIAN_POINT('Ctrl Pts',(6.31500890716424,-2.43791359063295,42.5797456418919));
#19227=CARTESIAN_POINT('Ctrl Pts',(6.37574818351,-2.27430495965851,42.587969530878));
#19228=CARTESIAN_POINT('Ctrl Pts',(6.43002808066008,-2.10879773376274,42.5961934198642));
#19229=CARTESIAN_POINT('Ctrl Pts',(6.48018176724473,-1.95587191829703,42.6037921511141));
#19230=CARTESIAN_POINT('Ctrl Pts',(6.52482129653724,-1.80132555495087,42.6113908823641));
#19231=CARTESIAN_POINT('Ctrl Pts',(6.56386471263037,-1.6455907857927,42.618989613614));
#19232=CARTESIAN_POINT('Ctrl Pts',(6.60612521175542,-1.47702384841073,42.6272144619361));
#19233=CARTESIAN_POINT('Ctrl Pts',(6.64194738592476,-1.30659134167416,42.6354393102581));
#19234=CARTESIAN_POINT('Ctrl Pts',(6.67116620613291,-1.13482617618305,42.6436641585801));
#19235=CARTESIAN_POINT('Ctrl Pts',(6.70035211947112,-0.963254456352035,
42.6518797438994));
#19236=CARTESIAN_POINT('Ctrl Pts',(6.72294942787765,-0.790353416846953,
42.6600953292186));
#19237=CARTESIAN_POINT('Ctrl Pts',(6.73884315648882,-0.616670018927359,
42.6683109145378));
#19238=CARTESIAN_POINT('Ctrl Pts',(6.75472217860409,-0.443147330570621,
42.676518897961));
#19239=CARTESIAN_POINT('Ctrl Pts',(6.76390994150824,-0.268844080524225,
42.6847268813842));
#19240=CARTESIAN_POINT('Ctrl Pts',(6.76634269161954,-0.0943163801617513,
42.6929348648074));
#19241=CARTESIAN_POINT('Ctrl Pts',(6.768773679333,0.0800848841803265,42.701136901984));
#19242=CARTESIAN_POINT('Ctrl Pts',(6.76445939649494,0.254709917682513,42.7093389391605));
#19243=CARTESIAN_POINT('Ctrl Pts',(6.75338798891608,0.428998451237325,42.7175409763371));
#19244=CARTESIAN_POINT('Ctrl Pts',(6.74232237874528,0.603195720719244,42.7257387186165));
#19245=CARTESIAN_POINT('Ctrl Pts',(6.72450671535754,0.777056484078363,42.733936460896));
#19246=CARTESIAN_POINT('Ctrl Pts',(6.69998122647779,0.950021349678609,42.7421342031754));
#19247=CARTESIAN_POINT('Ctrl Pts',(6.67546040071404,1.12295332887091,42.7503303867897));
#19248=CARTESIAN_POINT('Ctrl Pts',(6.64423233476188,1.29498939386639,42.7585265704041));
#19249=CARTESIAN_POINT('Ctrl Pts',(6.60638906358163,1.46557583924855,42.7667227540185));
#19250=CARTESIAN_POINT('Ctrl Pts',(6.56854857819412,1.6361497270883,42.7749183342793));
#19251=CARTESIAN_POINT('Ctrl Pts',(6.52409393423409,1.8052738573329,42.7831139145402));
#19252=CARTESIAN_POINT('Ctrl Pts',(6.47316817398407,1.9724053313961,42.7913094948011));
#19253=CARTESIAN_POINT('Ctrl Pts',(6.42223689724095,2.13955490984538,42.7995059628418));
#19254=CARTESIAN_POINT('Ctrl Pts',(6.36483321225574,2.30471105874899,42.8077024308825));
#19255=CARTESIAN_POINT('Ctrl Pts',(6.30114987824893,2.46734659337587,42.8158988989232));
#19256=CARTESIAN_POINT('Ctrl Pts',(6.23744805931675,2.63002933510593,42.8240977460966));
#19257=CARTESIAN_POINT('Ctrl Pts',(6.16746309147786,2.79018967117871,42.8322965932699));
#19258=CARTESIAN_POINT('Ctrl Pts',(6.091435676857,2.94732088424619,42.8404954404433));
#19259=CARTESIAN_POINT('Ctrl Pts',(6.01532880619455,3.1046163147116,42.8487028562093));
#19260=CARTESIAN_POINT('Ctrl Pts',(5.93316702881184,3.2588759740207,42.8569102719752));
#19261=CARTESIAN_POINT('Ctrl Pts',(5.8452372548959,3.40961734421579,42.8651176877412));
#19262=CARTESIAN_POINT('Ctrl Pts',(5.75726035371393,3.56043950648321,42.8733295023933));
#19263=CARTESIAN_POINT('Ctrl Pts',(5.66350948561644,3.70773931805832,42.8815413170454));
#19264=CARTESIAN_POINT('Ctrl Pts',(5.564314558757,3.85106381292298,42.8897531316975));
#19265=CARTESIAN_POINT('Ctrl Pts',(5.4649735522876,3.99459937489533,42.8979770394952));
#19266=CARTESIAN_POINT('Ctrl Pts',(5.36017268038438,4.13414763365764,42.9062009472928));
#19267=CARTESIAN_POINT('Ctrl Pts',(5.25028256087597,4.26928823470163,42.9144248550904));
#19268=CARTESIAN_POINT('Ctrl Pts',(5.14874611993157,4.39415565425196,42.9220235940139));
#19269=CARTESIAN_POINT('Ctrl Pts',(5.04286535323869,4.51526029391803,42.9296223329375));
#19270=CARTESIAN_POINT('Ctrl Pts',(4.93295950574095,4.63229959250479,42.9372210718611));
#19271=CARTESIAN_POINT('Ctrl Pts',(4.81503765735996,4.75787517139151,42.9453740260453));
#19272=CARTESIAN_POINT('Ctrl Pts',(4.69213232769796,4.87914231663287,42.9535269802296));
#19273=CARTESIAN_POINT('Ctrl Pts',(4.56459273787198,4.99567634433681,42.9616799344139));
#19274=CARTESIAN_POINT('Ctrl Pts',(4.43724053715183,5.11203915299198,42.9698209097702));
#19275=CARTESIAN_POINT('Ctrl Pts',(4.30526790901352,5.2236824543534,42.9779618851266));
#19276=CARTESIAN_POINT('Ctrl Pts',(4.16906305282286,5.3302159676309,42.986102860483));
#19277=CARTESIAN_POINT('Ctrl Pts',(4.03297357626649,5.43665923597774,42.9942369395892));
#19278=CARTESIAN_POINT('Ctrl Pts',(3.89265929133585,5.5380011053793,43.0023710186954));
#19279=CARTESIAN_POINT('Ctrl Pts',(3.74854431605663,5.6338889331047,43.0105050978017));
#19280=CARTESIAN_POINT('Ctrl Pts',(3.60454489032177,5.72969987919595,43.0186326551073));
#19281=CARTESIAN_POINT('Ctrl Pts',(3.45675114718345,5.82006529201822,43.0267602124129));
#19282=CARTESIAN_POINT('Ctrl Pts',(3.30561904837234,5.90467371723772,43.0348877697185));
#19283=CARTESIAN_POINT('Ctrl Pts',(3.23746843885906,5.94282653714844,43.038552762057));
#19284=CARTESIAN_POINT('Ctrl Pts',(3.16863942116908,5.97980928870432,43.0422177543954));
#19285=CARTESIAN_POINT('Ctrl Pts',(3.09917575053267,6.01559628526635,43.0458827467338));
#19286=CARTESIAN_POINT('Ctrl Pts',(3.09917575053253,6.01559628526642,41.0457515827422));
#19287=CARTESIAN_POINT('Ctrl Pts',(2.93382384459258,6.10078395293763,41.0545010306546));
#19288=CARTESIAN_POINT('Ctrl Pts',(2.76495772122977,6.17915010267052,41.063250478567));
#19289=CARTESIAN_POINT('Ctrl Pts',(2.59315093316703,6.25042856433181,41.0719999264794));
#19290=CARTESIAN_POINT('Ctrl Pts',(2.42134553245601,6.32170645041457,41.0807493037394));
#19291=CARTESIAN_POINT('Ctrl Pts',(2.24659977927567,6.38589665313466,41.0894986809994));
#19292=CARTESIAN_POINT('Ctrl Pts',(2.06950718689887,6.44278115439085,41.0982480582594));
#19293=CARTESIAN_POINT('Ctrl Pts',(1.89241596572834,6.49966521519732,41.1069973677741));
#19294=CARTESIAN_POINT('Ctrl Pts',(1.71297821457174,6.54924360009552,41.1157466772887));
#19295=CARTESIAN_POINT('Ctrl Pts',(1.53180337335825,6.59134792173561,41.1244959868034));
#19296=CARTESIAN_POINT('Ctrl Pts',(1.35062987477768,6.63345193135307,41.1332452314795));
#19297=CARTESIAN_POINT('Ctrl Pts',(1.16771959102943,6.66808192368239,41.1419944761556));
#19298=CARTESIAN_POINT('Ctrl Pts',(0.983693746906803,6.69512028363169,41.1507437208318));
#19299=CARTESIAN_POINT('Ctrl Pts',(0.799669205419937,6.72215845218866,41.1594929035759));
#19300=CARTESIAN_POINT('Ctrl Pts',(0.61452940287365,6.74160505424577,41.1682420863201));
#19301=CARTESIAN_POINT('Ctrl Pts',(0.428903127363531,6.7533940435412,41.1769912690643));
#19302=CARTESIAN_POINT('Ctrl Pts',(0.243278104164166,6.76518295330329,41.1857403927829));
#19303=CARTESIAN_POINT('Ctrl Pts',(0.0571669005394085,6.76931433552275,
41.1944895165015));
#19304=CARTESIAN_POINT('Ctrl Pts',(-0.128798404777218,6.76577415902474,
41.2032386402201));
#19305=CARTESIAN_POINT('Ctrl Pts',(-0.31476251725885,6.76223400523443,41.2119877078193));
#19306=CARTESIAN_POINT('Ctrl Pts',(-0.500580446819306,6.7510223966509,41.2207367754185));
#19307=CARTESIAN_POINT('Ctrl Pts',(-0.685621118842454,6.73217741012499,
41.2294858430177));
#19308=CARTESIAN_POINT('Ctrl Pts',(-0.870660665414367,6.71333253821773,
41.2382348574035));
#19309=CARTESIAN_POINT('Ctrl Pts',(-1.05492267885478,6.68685441030614,41.2469838717893));
#19310=CARTESIAN_POINT('Ctrl Pts',(-1.23778137635247,6.65283295028178,41.2557328861751));
#19311=CARTESIAN_POINT('Ctrl Pts',(-1.42999922978841,6.61707018861867,41.2649296965425));
#19312=CARTESIAN_POINT('Ctrl Pts',(-1.62066601233689,6.57297172934414,41.2741265069099));
#19313=CARTESIAN_POINT('Ctrl Pts',(-1.80906628500378,6.52070304311296,41.2833233172772));
#19314=CARTESIAN_POINT('Ctrl Pts',(-1.98831342545516,6.47097374915034,41.292073315015));
#19315=CARTESIAN_POINT('Ctrl Pts',(-2.16550875896686,6.41384933989534,41.3008233127528));
#19316=CARTESIAN_POINT('Ctrl Pts',(-2.34005036713991,6.34952386240483,41.3095733104905));
#19317=CARTESIAN_POINT('Ctrl Pts',(-2.51458843547069,6.28519968948604,41.3183231307714));
#19318=CARTESIAN_POINT('Ctrl Pts',(-2.68647261718036,6.21367483971107,41.3270729510523));
#19319=CARTESIAN_POINT('Ctrl Pts',(-2.85511905908713,6.13519226743852,41.3358227713331));
#19320=CARTESIAN_POINT('Ctrl Pts',(-3.02376230488867,6.05671118252946,41.3445724257917));
#19321=CARTESIAN_POINT('Ctrl Pts',(-3.18916767379888,5.97127275992642,41.3533220802502));
#19322=CARTESIAN_POINT('Ctrl Pts',(-3.35077334102772,5.87916720438005,41.3620717347087));
#19323=CARTESIAN_POINT('Ctrl Pts',(-3.51237616037362,5.78706327195647,41.3708212349772));
#19324=CARTESIAN_POINT('Ctrl Pts',(-3.67017916302304,5.68829258362296,41.3795707352456));
#19325=CARTESIAN_POINT('Ctrl Pts',(-3.82364636566475,5.58319061741033,41.3883202355141));
#19326=CARTESIAN_POINT('Ctrl Pts',(-3.97711106778817,5.47809036367688,41.3970695932225));
#19327=CARTESIAN_POINT('Ctrl Pts',(-4.12623987481952,5.36665920043206,41.4058189509309));
#19328=CARTESIAN_POINT('Ctrl Pts',(-4.27052628213961,5.24927559512309,41.4145683086394));
#19329=CARTESIAN_POINT('Ctrl Pts',(-4.41481053025001,5.13189374643016,41.4233175354159));
#19330=CARTESIAN_POINT('Ctrl Pts',(-4.55425230136545,5.00855981477339,41.4320667621924));
#19331=CARTESIAN_POINT('Ctrl Pts',(-4.68837800630555,4.87969268192069,41.4408159889689));
#19332=CARTESIAN_POINT('Ctrl Pts',(-4.8225018822889,4.75082730631813,41.4495650964398));
#19333=CARTESIAN_POINT('Ctrl Pts',(-4.95130963052951,4.61642907903541,41.4583142039106));
#19334=CARTESIAN_POINT('Ctrl Pts',(-5.07436379033342,4.47695444731718,41.4670633113814));
#19335=CARTESIAN_POINT('Ctrl Pts',(-5.19741643562785,4.33748153220611,41.4758123111712));
#19336=CARTESIAN_POINT('Ctrl Pts',(-5.31471544462757,4.1929325525461,41.4845613109609));
#19337=CARTESIAN_POINT('Ctrl Pts',(-5.42586245275615,4.0437984177962,41.4933103107507));
#19338=CARTESIAN_POINT('Ctrl Pts',(-5.53702160019143,3.89464799484357,41.5020602660928));
#19339=CARTESIAN_POINT('Ctrl Pts',(-5.64202723081243,3.74091164443862,41.510810221435));
#19340=CARTESIAN_POINT('Ctrl Pts',(-5.74052265232961,3.58311159163242,41.5195601767772));
#19341=CARTESIAN_POINT('Ctrl Pts',(-5.83901427066912,3.42531763191793,41.5283097942596));
#19342=CARTESIAN_POINT('Ctrl Pts',(-5.93099603115734,3.26346052695622,41.537059411742));
#19343=CARTESIAN_POINT('Ctrl Pts',(-6.01615550622749,3.09809004467086,41.5458090292245));
#19344=CARTESIAN_POINT('Ctrl Pts',(-6.101312145788,2.93272506863827,41.5545583553756));
#19345=CARTESIAN_POINT('Ctrl Pts',(-6.17964682328753,2.76384720416884,41.5633076815267));
#19346=CARTESIAN_POINT('Ctrl Pts',(-6.25089348288573,2.59203002791572,41.5720570076778));
#19347=CARTESIAN_POINT('Ctrl Pts',(-6.32213814889341,2.42021765937,41.5808060890094));
#19348=CARTESIAN_POINT('Ctrl Pts',(-6.38629508412598,2.24546640831882,41.5895551703409));
#19349=CARTESIAN_POINT('Ctrl Pts',(-6.44314639819826,2.06836976659998,41.5983042516725));
#19350=CARTESIAN_POINT('Ctrl Pts',(-6.50000285283712,1.89125711158234,41.6070541241069));
#19351=CARTESIAN_POINT('Ctrl Pts',(-6.5495522767326,1.71179891440215,41.6158039965413));
#19352=CARTESIAN_POINT('Ctrl Pts',(-6.59162635926394,1.53060476278394,41.6245538689757));
#19353=CARTESIAN_POINT('Ctrl Pts',(-6.63369752055211,1.3494231916463,41.6333031338982));
#19354=CARTESIAN_POINT('Ctrl Pts',(-6.66829431424271,1.1665061864261,41.6420523988207));
#19355=CARTESIAN_POINT('Ctrl Pts',(-6.69529923745435,0.982474997617332,
41.6508016637432));
#19356=CARTESIAN_POINT('Ctrl Pts',(-6.72230554731459,0.79843435917646,41.6595513779229));
#19357=CARTESIAN_POINT('Ctrl Pts',(-6.74171916496715,0.613279706239005,
41.6683010921026));
#19358=CARTESIAN_POINT('Ctrl Pts',(-6.75347414817284,0.427639953653992,
41.6770508062823));
#19359=CARTESIAN_POINT('Ctrl Pts',(-6.76248837758748,0.285283364197565,
41.6837604654582));
#19360=CARTESIAN_POINT('Ctrl Pts',(-6.76699999999997,0.142641701104487,
41.6904701246341));
#19361=CARTESIAN_POINT('Ctrl Pts',(-6.767,1.31890318194932E-12,41.69717978381));
#19362=CARTESIAN_POINT('',(-6.76699997529837,-0.000578197107039292,41.3028202161655));
#19363=CARTESIAN_POINT('Ctrl Pts',(3.09917575053255,6.01559628526641,40.6512265384361));
#19364=CARTESIAN_POINT('Ctrl Pts',(2.94551530212736,6.09476062956918,40.6593809815982));
#19365=CARTESIAN_POINT('Ctrl Pts',(2.78901715297729,6.16793186163224,40.6675354247604));
#19366=CARTESIAN_POINT('Ctrl Pts',(2.63020092619897,6.23492839476302,40.6756898679225));
#19367=CARTESIAN_POINT('Ctrl Pts',(2.60999793920778,6.24345101310468,40.6767271933423));
#19368=CARTESIAN_POINT('Ctrl Pts',(2.58975745831133,6.25187377711503,40.6777645187622));
#19369=CARTESIAN_POINT('Ctrl Pts',(2.56948056803328,6.26019637156051,40.6788018441821));
#19370=CARTESIAN_POINT('Ctrl Pts',(2.40868055201595,6.3261963006319,40.6870280535191));
#19371=CARTESIAN_POINT('Ctrl Pts',(2.24511120123291,6.38608902214036,40.695254262856));
#19372=CARTESIAN_POINT('Ctrl Pts',(2.0792765258894,6.43963493754773,40.703480472193));
#19373=CARTESIAN_POINT('Ctrl Pts',(1.91362815869939,6.49312069641301,40.7116974397362));
#19374=CARTESIAN_POINT('Ctrl Pts',(1.74571987291272,6.54027373847451,40.7199144072794));
#19375=CARTESIAN_POINT('Ctrl Pts',(1.57607673768459,6.58090199873312,40.7281313748226));
#19376=CARTESIAN_POINT('Ctrl Pts',(1.40659014051535,6.62149276929909,40.736340760166));
#19377=CARTESIAN_POINT('Ctrl Pts',(1.23537222860056,6.65557066558009,40.7445501455093));
#19378=CARTESIAN_POINT('Ctrl Pts',(1.06296444828513,6.68299301074615,40.7527595308527));
#19379=CARTESIAN_POINT('Ctrl Pts',(0.890681164586124,6.71039555408435,40.7609629881533));
#19380=CARTESIAN_POINT('Ctrl Pts',(0.717210076635454,6.73115206294866,40.7691664454539));
#19381=CARTESIAN_POINT('Ctrl Pts',(0.543104165577543,6.74517063278108,40.7773699027545));
#19382=CARTESIAN_POINT('Ctrl Pts',(0.369089052147779,6.75918189181697,40.7855690818863));
#19383=CARTESIAN_POINT('Ctrl Pts',(0.194440131780878,6.76646218339899,40.7937682610182));
#19384=CARTESIAN_POINT('Ctrl Pts',(0.019716964911336,6.76697127534133,40.80196744015));
#19385=CARTESIAN_POINT('Ctrl Pts',(-0.154973280348247,6.76748027135979,
40.8101650743798));
#19386=CARTESIAN_POINT('Ctrl Pts',(-0.329737385997837,6.76122060181682,
40.8183627086096));
#19387=CARTESIAN_POINT('Ctrl Pts',(-0.504014009278662,6.7482041224648,40.8265603428394));
#19388=CARTESIAN_POINT('Ctrl Pts',(-0.678278053081919,6.73518858265651,
40.834757385355));
#19389=CARTESIAN_POINT('Ctrl Pts',(-0.852054326845273,6.71541723018181,
40.8429544278706));
#19390=CARTESIAN_POINT('Ctrl Pts',(-1.0247848860671,6.68895394940707,40.8511514703862));
#19391=CARTESIAN_POINT('Ctrl Pts',(-1.19753437089774,6.66248776912398,40.859349411029));
#19392=CARTESIAN_POINT('Ctrl Pts',(-1.36923755830116,6.62932825409143,40.8675473516718));
#19393=CARTESIAN_POINT('Ctrl Pts',(-1.53934494120944,6.58959074237338,40.8757452923147));
#19394=CARTESIAN_POINT('Ctrl Pts',(-1.70950187915898,6.54984165447327,40.8839456211506));
#19395=CARTESIAN_POINT('Ctrl Pts',(-1.87806173743238,6.50351083446698,40.8921459499866));
#19396=CARTESIAN_POINT('Ctrl Pts',(-2.04448840290889,6.45076399896718,40.9003462788226));
#19397=CARTESIAN_POINT('Ctrl Pts',(-2.2110884892894,6.39796219989608,40.908555152614));
#19398=CARTESIAN_POINT('Ctrl Pts',(-2.37555059960082,6.33873113691363,40.9167640264054));
#19399=CARTESIAN_POINT('Ctrl Pts',(-2.53735596045524,6.27328572041337,40.9249729001968));
#19400=CARTESIAN_POINT('Ctrl Pts',(-2.69924816046197,6.20780518008,40.9331861796003));
#19401=CARTESIAN_POINT('Ctrl Pts',(-2.85848044179878,6.13610378456785,40.9413994590037));
#19402=CARTESIAN_POINT('Ctrl Pts',(-3.01455711976554,6.05844323004441,40.9496127384071));
#19403=CARTESIAN_POINT('Ctrl Pts',(-3.17086208440454,5.98066908475399,40.9578380310226));
#19404=CARTESIAN_POINT('Ctrl Pts',(-3.32400190709226,5.89691853377205,40.966063323638));
#19405=CARTESIAN_POINT('Ctrl Pts',(-3.47350736005325,5.80749822381858,40.9742886162535));
#19406=CARTESIAN_POINT('Ctrl Pts',(-3.60871708299939,5.72662829502928,40.9817274053655));
#19407=CARTESIAN_POINT('Ctrl Pts',(-3.74095446105745,5.64112172591948,40.9891661944776));
#19408=CARTESIAN_POINT('Ctrl Pts',(-3.86989548350949,5.55123391208773,40.9966049835897));
#19409=CARTESIAN_POINT('Ctrl Pts',(-4.01161479509416,5.45243805291246,41.0047809701915));
#19410=CARTESIAN_POINT('Ctrl Pts',(-4.14975890089944,5.3480648934046,41.0129569567933));
#19411=CARTESIAN_POINT('Ctrl Pts',(-4.28385665501696,5.2384025388726,41.0211329433951));
#19412=CARTESIAN_POINT('Ctrl Pts',(-4.41780315719193,5.12886387503369,41.0292997081135));
#19413=CARTESIAN_POINT('Ctrl Pts',(-4.54771211508459,5.014048121242,41.0374664728319));
#19414=CARTESIAN_POINT('Ctrl Pts',(-4.67314066217522,4.89428701155997,41.0456332375503));
#19415=CARTESIAN_POINT('Ctrl Pts',(-4.79845377853718,4.77463611691651,41.0537924864708));
#19416=CARTESIAN_POINT('Ctrl Pts',(-4.9192944328203,4.65004917789119,41.0619517353913));
#19417=CARTESIAN_POINT('Ctrl Pts',(-5.03525220343385,4.52089861065415,41.0701109843119));
#19418=CARTESIAN_POINT('Ctrl Pts',(-5.15112732565981,4.39184009491207,41.0782644177639));
#19419=CARTESIAN_POINT('Ctrl Pts',(-5.26212625302865,4.25822469807299,41.0864178512159));
#19420=CARTESIAN_POINT('Ctrl Pts',(-5.3678748597193,4.1204621695137,41.0945712846679));
#19421=CARTESIAN_POINT('Ctrl Pts',(-5.47357003594037,3.98276924675653,41.1027205985216));
#19422=CARTESIAN_POINT('Ctrl Pts',(-5.57401995448648,3.84093365376934,41.1108699123753));
#19423=CARTESIAN_POINT('Ctrl Pts',(-5.66889028254878,3.69539875580755,41.119019226229));
#19424=CARTESIAN_POINT('Ctrl Pts',(-5.76374507207625,3.549887694583,41.1271672053304));
#19425=CARTESIAN_POINT('Ctrl Pts',(-5.85302188730736,3.4006788359124,41.1353151844317));
#19426=CARTESIAN_POINT('Ctrl Pts',(-5.93642918259666,3.24824530477838,41.143463163533));
#19427=CARTESIAN_POINT('Ctrl Pts',(-6.01983274651937,3.0958185930165,41.1516107781207));
#19428=CARTESIAN_POINT('Ctrl Pts',(-6.09736713816796,2.94016781481091,41.1597583927084));
#19429=CARTESIAN_POINT('Ctrl Pts',(-6.16878639378154,2.7817914062517,41.1679060072961));
#19430=CARTESIAN_POINT('Ctrl Pts',(-6.24021587719233,2.62339231694936,41.1760547886861));
#19431=CARTESIAN_POINT('Ctrl Pts',(-6.30552833107212,2.46226715157735,41.184203570076));
#19432=CARTESIAN_POINT('Ctrl Pts',(-6.36452564273323,2.29893504540496,41.192352351466));
#19433=CARTESIAN_POINT('Ctrl Pts',(-6.42354249184777,2.13554885043892,41.2005038313931));
#19434=CARTESIAN_POINT('Ctrl Pts',(-6.47623991082771,1.96995460122454,41.2086553113202));
#19435=CARTESIAN_POINT('Ctrl Pts',(-6.52246942850797,1.80268731458867,41.2168067912473));
#19436=CARTESIAN_POINT('Ctrl Pts',(-6.56874694125375,1.63524637257448,41.2249667339668));
#19437=CARTESIAN_POINT('Ctrl Pts',(-6.60854304531649,1.46612927504205,41.2331266766864));
#19438=CARTESIAN_POINT('Ctrl Pts',(-6.64176006570574,1.2958827993289,41.2412866194059));
#19439=CARTESIAN_POINT('Ctrl Pts',(-6.67499648835186,1.12553688164852,41.249451328396));
#19440=CARTESIAN_POINT('Ctrl Pts',(-6.70164611365765,0.954060629730198,
41.2576160373861));
#19441=CARTESIAN_POINT('Ctrl Pts',(-6.72166310516942,0.782006458160169,
41.2657807463761));
#19442=CARTESIAN_POINT('Ctrl Pts',(-6.74170705281312,0.609720587688462,
41.2739564504737));
#19443=CARTESIAN_POINT('Ctrl Pts',(-6.75510049993274,0.436855604788317,
41.2821321545712));
#19444=CARTESIAN_POINT('Ctrl Pts',(-6.76184969379621,0.263965373691635,
41.2903078586687));
#19445=CARTESIAN_POINT('Ctrl Pts',(-6.76529275408913,0.175766471457374,
41.294478644501));
#19446=CARTESIAN_POINT('Ctrl Pts',(-6.76700750622803,0.0875609516987905,
41.2986494303332));
#19447=CARTESIAN_POINT('Ctrl Pts',(-6.76699997529837,-0.000578197106943801,
41.3028202161655));
#19448=CARTESIAN_POINT('Ctrl Pts',(-6.76699997529832,-0.000578197623143367,
41.3028202161899));
#19449=CARTESIAN_POINT('Ctrl Pts',(-6.76699300077022,-0.0822053604272126,
41.3066828517924));
#19450=CARTESIAN_POINT('Ctrl Pts',(-6.76550913867493,-0.163818062147753,
41.3105454873949));
#19451=CARTESIAN_POINT('Ctrl Pts',(-6.7625496072816,-0.245380946806069,
41.3144081229974));
#19452=CARTESIAN_POINT('Ctrl Pts',(-6.75630316093462,-0.417529207869196,
41.3225606792107));
#19453=CARTESIAN_POINT('Ctrl Pts',(-6.74346931326276,-0.589708059610257,
41.3307132354239));
#19454=CARTESIAN_POINT('Ctrl Pts',(-6.72403209526724,-0.761368098764339,
41.3388657916372));
#19455=CARTESIAN_POINT('Ctrl Pts',(-6.70461739575737,-0.932829265624681,
41.3470089029176));
#19456=CARTESIAN_POINT('Ctrl Pts',(-6.67861459501554,-1.1037724568311,41.3551520141979));
#19457=CARTESIAN_POINT('Ctrl Pts',(-6.64605970415537,-1.27364807101581,
41.3632951254782));
#19458=CARTESIAN_POINT('Ctrl Pts',(-6.61353568466071,-1.44336259443845,
41.3714305147556));
#19459=CARTESIAN_POINT('Ctrl Pts',(-6.5744720131826,-1.61201119977722,41.3795659040329));
#19460=CARTESIAN_POINT('Ctrl Pts',(-6.52895649381364,-1.77904921289118,
41.3877012933103));
#19461=CARTESIAN_POINT('Ctrl Pts',(-6.48347457229122,-1.94596392481888,
41.3958306773489));
#19462=CARTESIAN_POINT('Ctrl Pts',(-6.43155038157621,-2.11127006057263,
41.4039600613875));
#19463=CARTESIAN_POINT('Ctrl Pts',(-6.37332281721652,-2.27443295516646,
41.4120894454261));
#19464=CARTESIAN_POINT('Ctrl Pts',(-6.31512600368384,-2.43750968105306,
41.4202145362182));
#19465=CARTESIAN_POINT('Ctrl Pts',(-6.25063256875132,-2.59844507643375,
41.4283396270104));
#19466=CARTESIAN_POINT('Ctrl Pts',(-6.18003129058261,-2.75671947202101,
41.4364647178026));
#19467=CARTESIAN_POINT('Ctrl Pts',(-6.10916051203007,-2.91559803528723,
41.4446208238277));
#19468=CARTESIAN_POINT('Ctrl Pts',(-6.03213527368781,-3.07179488638972,
41.4527769298528));
#19469=CARTESIAN_POINT('Ctrl Pts',(-5.94919558390946,-3.2248040102295,41.4609330358779));
#19470=CARTESIAN_POINT('Ctrl Pts',(-5.86658971138256,-3.37719730001799,
41.4690563150513));
#19471=CARTESIAN_POINT('Ctrl Pts',(-5.7781171026914,-3.52642816140395,41.4771795942247));
#19472=CARTESIAN_POINT('Ctrl Pts',(-5.68406107456446,-3.67202106483896,
41.4853028733981));
#19473=CARTESIAN_POINT('Ctrl Pts',(-5.5899925220826,-3.81763335519935,41.4934272342548));
#19474=CARTESIAN_POINT('Ctrl Pts',(-5.49033926782225,-3.95960641541173,
41.5015515951115));
#19475=CARTESIAN_POINT('Ctrl Pts',(-5.38542804251937,-4.09749359961013,
41.5096759559682));
#19476=CARTESIAN_POINT('Ctrl Pts',(-5.28048288749987,-4.23542537839859,
41.5178029443536));
#19477=CARTESIAN_POINT('Ctrl Pts',(-5.17027659660184,-4.36926835880579,
41.525929932739));
#19478=CARTESIAN_POINT('Ctrl Pts',(-5.05517623096443,-4.4986089265341,41.5340569211244));
#19479=CARTESIAN_POINT('Ctrl Pts',(-4.93933175456783,-4.62878566630681,
41.5422364495645));
#19480=CARTESIAN_POINT('Ctrl Pts',(-4.81852995461568,-4.75440129564737,
41.5504159780046));
#19481=CARTESIAN_POINT('Ctrl Pts',(-4.69318208614446,-4.87507240010779,
41.5585955064446));
#19482=CARTESIAN_POINT('Ctrl Pts',(-4.56842452119599,-4.9951752254349,41.5667365148483));
#19483=CARTESIAN_POINT('Ctrl Pts',(-4.43916392892557,-5.11037980130094,
41.574877523252));
#19484=CARTESIAN_POINT('Ctrl Pts',(-4.30583804466706,-5.22034938802929,
41.5830185316556));
#19485=CARTESIAN_POINT('Ctrl Pts',(-4.17156589227026,-5.33109947373337,
41.5912173201139));
#19486=CARTESIAN_POINT('Ctrl Pts',(-4.03317083000002,-5.43653975866168,
41.5994161085721));
#19487=CARTESIAN_POINT('Ctrl Pts',(-3.891128225651,-5.53637156733018,41.6076148970304));
#19488=CARTESIAN_POINT('Ctrl Pts',(-3.74908562130194,-5.63620337599872,
41.6158136854886));
#19489=CARTESIAN_POINT('Ctrl Pts',(-3.60339582188938,-5.73042656113058,
41.6240124739468));
#19490=CARTESIAN_POINT('Ctrl Pts',(-3.45455747197761,-5.81879039601907,
41.6322112624051));
#19491=CARTESIAN_POINT('Ctrl Pts',(-3.30509714590246,-5.90752349191479,
41.6404443125371));
#19492=CARTESIAN_POINT('Ctrl Pts',(-3.15199735783756,-5.99062409752655,
41.6486773626691));
#19493=CARTESIAN_POINT('Ctrl Pts',(-2.99572046393637,-6.06777948692542,
41.6569104128011));
#19494=CARTESIAN_POINT('Ctrl Pts',(-2.83962967179355,-6.14484299611554,
41.665133658636));
#19495=CARTESIAN_POINT('Ctrl Pts',(-2.68036962560976,-6.21597522979205,
41.6733569044708));
#19496=CARTESIAN_POINT('Ctrl Pts',(-2.5184306862568,-6.28090724963521,41.6815801503057));
#19497=CARTESIAN_POINT('Ctrl Pts',(-2.35665217885975,-6.34577494170775,
41.6897952494192));
#19498=CARTESIAN_POINT('Ctrl Pts',(-2.19220039386249,-6.40445452045606,
41.6980103485327));
#19499=CARTESIAN_POINT('Ctrl Pts',(-2.02558935548251,-6.45672337667922,
41.7062254476462));
#19500=CARTESIAN_POINT('Ctrl Pts',(-1.85911004216774,-6.50895090839855,
41.7144340517851));
#19501=CARTESIAN_POINT('Ctrl Pts',(-1.69047521596552,-6.55477770611507,
41.722642655924));
#19502=CARTESIAN_POINT('Ctrl Pts',(-1.52021799328566,-6.5940295914479,41.7308512600629));
#19503=CARTESIAN_POINT('Ctrl Pts',(-1.35006132220516,-6.63325829515127,
41.7390550163119));
#19504=CARTESIAN_POINT('Ctrl Pts',(-1.17828451153328,-6.66591974179152,
41.7472587725609));
#19505=CARTESIAN_POINT('Ctrl Pts',(-1.00543501373014,-6.69188982524111,
41.7554625288098));
#19506=CARTESIAN_POINT('Ctrl Pts',(-0.832636657736434,-6.71785222479762,
41.7636638577741));
#19507=CARTESIAN_POINT('Ctrl Pts',(-0.658766600006017,-6.73712714789639,
41.7718651867384));
#19508=CARTESIAN_POINT('Ctrl Pts',(-0.484381893107001,-6.74964170764864,
41.7800665157027));
#19509=CARTESIAN_POINT('Ctrl Pts',(-0.310021235523848,-6.76215454152363,
41.7882667136254));
#19510=CARTESIAN_POINT('Ctrl Pts',(-0.135146427312531,-6.7679088424695,
41.7964669115481));
#19511=CARTESIAN_POINT('Ctrl Pts',(0.039680932635225,-6.76688365672007,
41.8046671094709));
#19512=CARTESIAN_POINT('Ctrl Pts',(0.214515864495584,-6.76585842656903,
41.8128676625507));
#19513=CARTESIAN_POINT('Ctrl Pts',(0.389302985699496,-6.75805312679117,
41.8210682156306));
#19514=CARTESIAN_POINT('Ctrl Pts',(0.563481212773167,-6.74349893770672,
41.8292687687104));
#19515=CARTESIAN_POINT('Ctrl Pts',(0.737698548151672,-6.72894148076456,
41.8374711630636));
#19516=CARTESIAN_POINT('Ctrl Pts',(0.911306360135065,-6.70763214623251,
41.8456735574168));
#19517=CARTESIAN_POINT('Ctrl Pts',(1.08374913724422,-6.67965394369517,41.85387595177));
#19518=CARTESIAN_POINT('Ctrl Pts',(1.25635317866392,-6.65164957662013,41.8620860168039));
#19519=CARTESIAN_POINT('Ctrl Pts',(1.42778965433692,-6.61696393885949,41.8702960818377));
#19520=CARTESIAN_POINT('Ctrl Pts',(1.59751276324409,-6.57573128794602,41.8785061468715));
#19521=CARTESIAN_POINT('Ctrl Pts',(1.76731709862022,-6.53447890381731,41.8867201410968));
#19522=CARTESIAN_POINT('Ctrl Pts',(1.93540608788346,-6.48667335723624,41.8949341353222));
#19523=CARTESIAN_POINT('Ctrl Pts',(2.10124960291294,-6.43249866741208,41.9031481295475));
#19524=CARTESIAN_POINT('Ctrl Pts',(2.26731921788926,-6.37825011944226,41.9113733221827));
#19525=CARTESIAN_POINT('Ctrl Pts',(2.43113690442495,-6.31761519901466,41.9195985148178));
#19526=CARTESIAN_POINT('Ctrl Pts',(2.59219187337344,-6.25082636869852,41.927823707453));
#19527=CARTESIAN_POINT('Ctrl Pts',(2.73702826199803,-6.19076331664487,41.935220605573));
#19528=CARTESIAN_POINT('Ctrl Pts',(2.87963046621809,-6.12572408816284,41.9426175036929));
#19529=CARTESIAN_POINT('Ctrl Pts',(3.01964500430957,-6.05590893656338,41.9500144018129));
#19530=CARTESIAN_POINT('Ctrl Pts',(3.18330293023272,-5.97430453273133,41.9586603683038));
#19531=CARTESIAN_POINT('Ctrl Pts',(3.34379671844566,-5.88598941906037,41.9673063347946));
#19532=CARTESIAN_POINT('Ctrl Pts',(3.50057226502568,-5.79122463882493,41.9759523012855));
#19533=CARTESIAN_POINT('Ctrl Pts',(3.6571472743686,-5.69658107562633,41.9845872084099));
#19534=CARTESIAN_POINT('Ctrl Pts',(3.81001326636679,-5.59550445384675,41.9932221155342));
#19535=CARTESIAN_POINT('Ctrl Pts',(3.95863978141795,-5.4883021127645,42.0018570226586));
#19536=CARTESIAN_POINT('Ctrl Pts',(4.1122005768098,-5.37754074048316,42.0107786017301));
#19537=CARTESIAN_POINT('Ctrl Pts',(4.26123526340441,-5.26024003820608,42.0197001808016));
#19538=CARTESIAN_POINT('Ctrl Pts',(4.40518767082388,-5.13678991052012,42.028621759873));
#19539=CARTESIAN_POINT('Ctrl Pts',(4.54412974150958,-5.01763652729729,42.0372328188487));
#19540=CARTESIAN_POINT('Ctrl Pts',(4.67833706471288,-4.89275476582606,42.0458438778244));
#19541=CARTESIAN_POINT('Ctrl Pts',(4.8073396277206,-4.76253868265101,42.0544549368001));
#19542=CARTESIAN_POINT('Ctrl Pts',(4.93622053535602,-4.63244539925378,42.0630578751496));
#19543=CARTESIAN_POINT('Ctrl Pts',(5.05990625479924,-4.49702803960598,42.0716608134992));
#19544=CARTESIAN_POINT('Ctrl Pts',(5.17796138381624,-4.35671951216828,42.0802637518487));
#19545=CARTESIAN_POINT('Ctrl Pts',(5.29588431839897,-4.2165680978231,42.0888570568975));
#19546=CARTESIAN_POINT('Ctrl Pts',(5.40818904485295,-4.07153667495343,42.0974503619462));
#19547=CARTESIAN_POINT('Ctrl Pts',(5.51447829534973,-3.92209359017818,42.106043666995));
#19548=CARTESIAN_POINT('Ctrl Pts',(5.52632065763324,-3.90544318439959,42.1070011018355));
#19549=CARTESIAN_POINT('Ctrl Pts',(5.53808838564072,-3.88873804974682,42.107958536676));
#19550=CARTESIAN_POINT('Ctrl Pts',(5.54978095996358,-3.87197886053446,42.1089159715166));
#19551=CARTESIAN_POINT('Ctrl Pts',(5.65475576318882,-3.7215164780681,42.1175117290641));
#19552=CARTESIAN_POINT('Ctrl Pts',(5.75354654205222,-3.56687090449153,42.1261074866117));
#19553=CARTESIAN_POINT('Ctrl Pts',(5.84584546916468,-3.40857444551924,42.1347032441592));
#19554=CARTESIAN_POINT('Ctrl Pts',(5.93823051431431,-3.25013029056863,42.1433070218408));
#19555=CARTESIAN_POINT('Ctrl Pts',(6.02411146370063,-3.08802871466845,42.1519107995225));
#19556=CARTESIAN_POINT('Ctrl Pts',(6.10322690035181,-2.92282575649355,42.1605145772041));
#19557=CARTESIAN_POINT('Ctrl Pts',(6.18545164284543,-2.75113017760155,42.1694564908721));
#19558=CARTESIAN_POINT('Ctrl Pts',(6.26036818667169,-2.57608485797007,42.1783984045401));
#19559=CARTESIAN_POINT('Ctrl Pts',(6.32773899548431,-2.39833446479578,42.1873403182082));
#19560=CARTESIAN_POINT('Ctrl Pts',(6.39273868351397,-2.22684001034127,42.1959675205389));
#19561=CARTESIAN_POINT('Ctrl Pts',(6.45071468212739,-2.05282794452216,42.2045947228696));
#19562=CARTESIAN_POINT('Ctrl Pts',(6.50150514702655,-1.87689099928241,42.2132219252003));
#19563=CARTESIAN_POINT('Ctrl Pts',(6.55234398206938,-1.70078650103176,42.2218573436207));
#19564=CARTESIAN_POINT('Ctrl Pts',(6.59598354837541,-1.52275375950016,42.2304927620411));
#19565=CARTESIAN_POINT('Ctrl Pts',(6.63231300466784,-1.34339614712631,42.2391281804615));
#19566=CARTESIAN_POINT('Ctrl Pts',(6.66869613255724,-1.1637735594276,42.2477763564827));
#19567=CARTESIAN_POINT('Ctrl Pts',(6.69774751649917,-0.982822489873342,
42.2564245325038));
#19568=CARTESIAN_POINT('Ctrl Pts',(6.7194078817565,-0.801153367707252,42.2650727085249));
#19569=CARTESIAN_POINT('Ctrl Pts',(6.7216994662713,-0.781933463415356,42.2659876527567));
#19570=CARTESIAN_POINT('Ctrl Pts',(6.72390837236021,-0.762705523586282,
42.2669025969886));
#19571=CARTESIAN_POINT('Ctrl Pts',(6.72603456392106,-0.743470271725283,
42.2678175412204));
#19572=CARTESIAN_POINT('Ctrl Pts',(6.74515052237273,-0.570531820575015,
42.2760435337617));
#19573=CARTESIAN_POINT('Ctrl Pts',(6.75761744990937,-0.396628656856025,
42.2842695263031));
#19574=CARTESIAN_POINT('Ctrl Pts',(6.76334725359576,-0.222312679077808,
42.2924955188444));
#19575=CARTESIAN_POINT('Ctrl Pts',(6.76907105032358,-0.0481794490710688,
42.3007128874958));
#19576=CARTESIAN_POINT('Ctrl Pts',(6.76807177658168,0.126365378010484,42.3089302561473));
#19577=CARTESIAN_POINT('Ctrl Pts',(6.76031290176944,0.300763146295607,42.3171476247987));
#19578=CARTESIAN_POINT('Ctrl Pts',(6.75256060861734,0.475012977300236,42.3253580228611));
#19579=CARTESIAN_POINT('Ctrl Pts',(6.73806015026366,0.649115642033112,42.3335684209235));
#19580=CARTESIAN_POINT('Ctrl Pts',(6.71682701035082,0.822510737329076,42.3417788189858));
#19581=CARTESIAN_POINT('Ctrl Pts',(6.6956076345185,0.995793431724204,42.3499838947746));
#19582=CARTESIAN_POINT('Ctrl Pts',(6.66766431401944,1.16836911596368,42.3581889705634));
#19583=CARTESIAN_POINT('Ctrl Pts',(6.63306450304007,1.33968067035015,42.3663940463522));
#19584=CARTESIAN_POINT('Ctrl Pts',(6.5984802009793,1.51091543654391,42.3745954443217));
#19585=CARTESIAN_POINT('Ctrl Pts',(6.5572454235981,1.68088685131457,42.3827968422912));
#19586=CARTESIAN_POINT('Ctrl Pts',(6.50947905684096,1.84904608069918,42.3909982402606));
#19587=CARTESIAN_POINT('Ctrl Pts',(6.46171643154333,2.01719213845294,42.3991989958284));
#19588=CARTESIAN_POINT('Ctrl Pts',(6.40742332536684,2.1835259467978,42.4073997513961));
#19589=CARTESIAN_POINT('Ctrl Pts',(6.34676911807194,2.34751161059713,42.4156005069638));
#19590=CARTESIAN_POINT('Ctrl Pts',(6.28611521887159,2.51149644142721,42.4238012208756));
#19591=CARTESIAN_POINT('Ctrl Pts',(6.21910040623486,2.6731328149813,42.4320019347873));
#19592=CARTESIAN_POINT('Ctrl Pts',(6.14594301737774,2.83190279267241,42.4402026486991));
#19593=CARTESIAN_POINT('Ctrl Pts',(6.07277274218481,2.99070073696103,42.4484048071287));
#19594=CARTESIAN_POINT('Ctrl Pts',(5.99345788507549,3.14663095396814,42.4566069655583));
#19595=CARTESIAN_POINT('Ctrl Pts',(5.90826376476316,3.29919812772539,42.464809123988));
#19596=CARTESIAN_POINT('Ctrl Pts',(5.82303919844145,3.45181982474768,42.4730142136409));
#19597=CARTESIAN_POINT('Ctrl Pts',(5.731931358044,3.60107577165232,42.4812193032938));
#19598=CARTESIAN_POINT('Ctrl Pts',(5.63525011239159,3.74649772064399,42.4894243929467));
#19599=CARTESIAN_POINT('Ctrl Pts',(5.53845841984662,3.89208579701919,42.4976388559445));
#19600=CARTESIAN_POINT('Ctrl Pts',(5.43608080059845,4.03383082649398,42.5058533189423));
#19601=CARTESIAN_POINT('Ctrl Pts',(5.32846946003411,4.17129502834358,42.5140677819401));
#19602=CARTESIAN_POINT('Ctrl Pts',(5.22079436315163,4.30884067338809,42.5222871117476));
#19603=CARTESIAN_POINT('Ctrl Pts',(5.10787959512425,4.44210016211765,42.530506441555));
#19604=CARTESIAN_POINT('Ctrl Pts',(4.99011572398894,4.57067107339812,42.5387257713625));
#19605=CARTESIAN_POINT('Ctrl Pts',(4.87216938487518,4.69944119751054,42.5469578365232));
#19606=CARTESIAN_POINT('Ctrl Pts',(4.74935917990521,4.8235079720207,42.5551899016839));
#19607=CARTESIAN_POINT('Ctrl Pts',(4.62211136750552,4.94250700620407,42.5634219668446));
#19608=CARTESIAN_POINT('Ctrl Pts',(4.50773189682578,5.04947188272816,42.5708215381057));
#19609=CARTESIAN_POINT('Ctrl Pts',(4.3897675643863,5.15234259889075,42.5782211093669));
#19610=CARTESIAN_POINT('Ctrl Pts',(4.26854835633068,5.25088410933499,42.5856206806281));
#19611=CARTESIAN_POINT('Ctrl Pts',(4.13492892115702,5.35950601157244,42.5937771976381));
#19612=CARTESIAN_POINT('Ctrl Pts',(3.99694264807765,5.46320145068243,42.6019337146481));
#19613=CARTESIAN_POINT('Ctrl Pts',(3.85499061912882,5.56159476467217,42.6100902316581));
#19614=CARTESIAN_POINT('Ctrl Pts',(3.71323923686838,5.65984900144858,42.6182352195753));
#19615=CARTESIAN_POINT('Ctrl Pts',(3.56753356038438,5.75281583359409,42.6263802074924));
#19616=CARTESIAN_POINT('Ctrl Pts',(3.41830902533422,5.84015859436357,42.6345251954095));
#19617=CARTESIAN_POINT('Ctrl Pts',(3.31360945068443,5.90144040635399,42.6402399176579));
#19618=CARTESIAN_POINT('Ctrl Pts',(3.20717838310867,5.95995439641602,42.6459546399062));
#19619=CARTESIAN_POINT('Ctrl Pts',(3.09917575053259,6.01559628526639,42.6516693621546));
#19620=CARTESIAN_POINT('Origin',(0.,0.,-3.69717978381041));
#19621=CARTESIAN_POINT('',(3.09917575053261,6.01559628526638,45.0457515827422));
#19622=CARTESIAN_POINT('',(3.09917575053253,6.01559628526642,44.6513725725535));
#19623=CARTESIAN_POINT('',(3.09917575053259,6.01559628526639,-3.69717978381041));
#19624=CARTESIAN_POINT('',(-6.7672120803281,0.000214420623927318,43.6968126146988));
#19625=CARTESIAN_POINT('Ctrl Pts',(-6.767,1.46149302575801E-12,43.69717978381));
#19626=CARTESIAN_POINT('Ctrl Pts',(-6.76700000000004,-0.186007249414336,
43.705929295616));
#19627=CARTESIAN_POINT('Ctrl Pts',(-6.75932637295445,-0.372014355526311,
43.7146788074219));
#19628=CARTESIAN_POINT('Ctrl Pts',(-6.74400518266937,-0.557389537153946,
43.7234283192279));
#19629=CARTESIAN_POINT('Ctrl Pts',(-6.72868405709656,-0.742763935810554,
43.7321777940784));
#19630=CARTESIAN_POINT('Ctrl Pts',(-6.70571545653,-0.92750612969445,43.740927268929));
#19631=CARTESIAN_POINT('Ctrl Pts',(-6.67517739415656,-1.11098863924943,
43.7496767437795));
#19632=CARTESIAN_POINT('Ctrl Pts',(-6.64463945823074,-1.29447038906637,
43.7584261824015));
#19633=CARTESIAN_POINT('Ctrl Pts',(-6.60653217027127,-1.47669218228355,
43.7671756210235));
#19634=CARTESIAN_POINT('Ctrl Pts',(-6.56098496116676,-1.65703510504262,
43.7759250596455));
#19635=CARTESIAN_POINT('Ctrl Pts',(-6.51543793687472,-1.83737729604181,
43.7846744627657));
#19636=CARTESIAN_POINT('Ctrl Pts',(-6.46245112202584,-2.01584035397232,
43.793423865886));
#19637=CARTESIAN_POINT('Ctrl Pts',(-6.40220448416175,-2.19181813638339,
43.8021732690062));
#19638=CARTESIAN_POINT('Ctrl Pts',(-6.34195808575108,-2.36779521936157,
43.8109226373515));
#19639=CARTESIAN_POINT('Ctrl Pts',(-6.27445201489142,-2.54128677545057,
43.8196720056968));
#19640=CARTESIAN_POINT('Ctrl Pts',(-6.19991555136076,-2.71170355238086,
43.8284213740421));
#19641=CARTESIAN_POINT('Ctrl Pts',(-6.1253793778893,-2.88211966613302,43.8371707083391));
#19642=CARTESIAN_POINT('Ctrl Pts',(-6.04381298133508,-3.0494607621066,43.8459200426362));
#19643=CARTESIAN_POINT('Ctrl Pts',(-5.95549339426198,-3.21315848207055,
43.8546693769332));
#19644=CARTESIAN_POINT('Ctrl Pts',(-5.86717414355047,-3.37685557859834,
43.8634186779088));
#19645=CARTESIAN_POINT('Ctrl Pts',(-5.77210188986118,-3.53690907467507,
43.8721679788843));
#19646=CARTESIAN_POINT('Ctrl Pts',(-5.67059953466942,-3.69277536785098,
43.8809172798599));
#19647=CARTESIAN_POINT('Ctrl Pts',(-5.56909755761632,-3.84864108035987,
43.8896665482406));
#19648=CARTESIAN_POINT('Ctrl Pts',(-5.46116568337928,-4.00031938104473,
43.8984158166214));
#19649=CARTESIAN_POINT('Ctrl Pts',(-5.34717048685965,-4.14729511663412,
43.9071650850022));
#19650=CARTESIAN_POINT('Ctrl Pts',(-5.23317570555368,-4.29427031688222,
43.9159143215148));
#19651=CARTESIAN_POINT('Ctrl Pts',(-5.11311782178657,-4.436542759873,43.9246635580274));
#19652=CARTESIAN_POINT('Ctrl Pts',(-4.98740459171868,-4.57362924147809,
43.93341279454));
#19653=CARTESIAN_POINT('Ctrl Pts',(-4.86169180910655,-4.71071523514618,
43.9421619999112));
#19654=CARTESIAN_POINT('Ctrl Pts',(-4.73032391415227,-4.84261509316725,
43.9509112052823));
#19655=CARTESIAN_POINT('Ctrl Pts',(-4.59374707237057,-4.96888084331742,
43.9596604106534));
#19656=CARTESIAN_POINT('Ctrl Pts',(-4.45717070537163,-5.09514615452933,
43.9684095856097));
#19657=CARTESIAN_POINT('Ctrl Pts',(-4.31538563819269,-5.21577720253831,
43.9771587605659));
#19658=CARTESIAN_POINT('Ctrl Pts',(-4.16887341290407,-5.33036429028838,
43.9859079355221));
#19659=CARTESIAN_POINT('Ctrl Pts',(-4.02236168477094,-5.44495098921357,
43.99465708079));
#19660=CARTESIAN_POINT('Ctrl Pts',(-3.87112305634193,-5.55349359238931,
44.0034062260579));
#19661=CARTESIAN_POINT('Ctrl Pts',(-3.71567117316484,-5.65562346102636,
44.0121553713259));
#19662=CARTESIAN_POINT('Ctrl Pts',(-3.56021980457064,-5.75775299158915,
44.020904487632));
#19663=CARTESIAN_POINT('Ctrl Pts',(-3.40055544862164,-5.85346967275483,
44.0296536039382));
#19664=CARTESIAN_POINT('Ctrl Pts',(-3.23722036323193,-5.94244842803676,
44.0384027202443));
#19665=CARTESIAN_POINT('Ctrl Pts',(-3.07388580495827,-6.03142689616588,
44.0471518083153));
#19666=CARTESIAN_POINT('Ctrl Pts',(-2.90688079257477,-6.11366734484932,
44.0559008963862));
#19667=CARTESIAN_POINT('Ctrl Pts',(-2.73677251094374,-6.18889046787408,
44.0646499844572));
#19668=CARTESIAN_POINT('Ctrl Pts',(-2.56666476416412,-6.26411335438365,
44.0733990450194));
#19669=CARTESIAN_POINT('Ctrl Pts',(-2.39345402971868,-6.33231884350375,
44.0821481055816));
#19670=CARTESIAN_POINT('Ctrl Pts',(-2.21772856473822,-6.39327529621118,
44.0908971661438));
#19671=CARTESIAN_POINT('Ctrl Pts',(-2.04200363768048,-6.45423156232152,
44.0996461999238));
#19672=CARTESIAN_POINT('Ctrl Pts',(-1.86376426619866,-6.50793874252121,
44.1083952337038));
#19673=CARTESIAN_POINT('Ctrl Pts',(-1.68361578194456,-6.55421443796182,
44.1171442674838));
#19674=CARTESIAN_POINT('Ctrl Pts',(-1.50346783419641,-6.60048999558731,
44.1258932752081));
#19675=CARTESIAN_POINT('Ctrl Pts',(-1.32141106257024,-6.63933404145539,
44.1346422829323));
#19676=CARTESIAN_POINT('Ctrl Pts',(-1.13806375958828,-6.67061465527067,
44.1433912906565));
#19677=CARTESIAN_POINT('Ctrl Pts',(-0.954716987416852,-6.70189517852514,
44.1521402730514));
#19678=CARTESIAN_POINT('Ctrl Pts',(-0.77007997380744,-6.72561226535856,
44.1608892554463));
#19679=CARTESIAN_POINT('Ctrl Pts',(-0.58477977054989,-6.74168536939804,
44.1696382378412));
#19680=CARTESIAN_POINT('Ctrl Pts',(-0.391490647551392,-6.75845143942408,
44.1787644185172));
#19681=CARTESIAN_POINT('Ctrl Pts',(-0.197480213101866,-6.76689975924034,
44.1878905991933));
#19682=CARTESIAN_POINT('Ctrl Pts',(-0.00346532629538061,-6.76699911271708,
44.1970167798693));
#19683=CARTESIAN_POINT('Ctrl Pts',(0.184486595298432,-6.76709536139767,
44.2058577673993));
#19684=CARTESIAN_POINT('Ctrl Pts',(0.372442378187562,-6.75935659726757,
44.2146987549292));
#19685=CARTESIAN_POINT('Ctrl Pts',(0.559750217724375,-6.74380965728998,
44.2235397424591));
#19686=CARTESIAN_POINT('Ctrl Pts',(0.745129914460036,-6.72842275717228,
44.2322897210569));
#19687=CARTESIAN_POINT('Ctrl Pts',(0.929874656316456,-6.70538772273441,
44.2410396996547));
#19688=CARTESIAN_POINT('Ctrl Pts',(1.11335688290003,-6.67478280180705,44.2497896782524));
#19689=CARTESIAN_POINT('Ctrl Pts',(1.29683723119081,-6.6441781941798,44.2585395672774));
#19690=CARTESIAN_POINT('Ctrl Pts',(1.47905480730458,-6.60600390230025,44.2672894563023));
#19691=CARTESIAN_POINT('Ctrl Pts',(1.65939064805029,-6.56038959797078,44.2760393453272));
#19692=CARTESIAN_POINT('Ctrl Pts',(1.8397247026449,-6.51477574543193,44.2847891476882));
#19693=CARTESIAN_POINT('Ctrl Pts',(2.01817678126076,-6.46172209820029,44.2935389500492));
#19694=CARTESIAN_POINT('Ctrl Pts',(2.1941407234791,-6.40140886723935,44.3022887524101));
#19695=CARTESIAN_POINT('Ctrl Pts',(2.37010298132326,-6.34109621361289,44.3110384710156));
#19696=CARTESIAN_POINT('Ctrl Pts',(2.54357687927141,-6.27352420825879,44.3197881896211));
#19697=CARTESIAN_POINT('Ctrl Pts',(2.71397317790197,-6.19892237325397,44.3285379082266));
#19698=CARTESIAN_POINT('Ctrl Pts',(2.88436790207423,-6.12432122756859,44.3372875459848));
#19699=CARTESIAN_POINT('Ctrl Pts',(3.05168482126474,-6.04269049717307,44.3460371837431));
#19700=CARTESIAN_POINT('Ctrl Pts',(3.21535561997602,-5.95430745234814,44.3547868215014));
#19701=CARTESIAN_POINT('Ctrl Pts',(3.3790249607549,-5.86592519481396,44.3635363813204));
#19702=CARTESIAN_POINT('Ctrl Pts',(3.5390479938508,-5.77079087940106,44.3722859411394));
#19703=CARTESIAN_POINT('Ctrl Pts',(3.69488118815184,-5.66922763746894,44.3810355009584));
#19704=CARTESIAN_POINT('Ctrl Pts',(3.85071304611026,-5.56766526648918,44.3897849857458));
#19705=CARTESIAN_POINT('Ctrl Pts',(4.00235489706154,-5.45967423580577,44.3985344705333));
#19706=CARTESIAN_POINT('Ctrl Pts',(4.14929168607833,-5.34562133936189,44.4072839553207));
#19707=CARTESIAN_POINT('Ctrl Pts',(4.29622726385928,-5.2315693830839,44.416033367984));
#19708=CARTESIAN_POINT('Ctrl Pts',(4.43845763092229,-5.11145583677061,44.4247827806473));
#19709=CARTESIAN_POINT('Ctrl Pts',(4.57549970661116,-4.9856886620407,44.4335321933106));
#19710=CARTESIAN_POINT('Ctrl Pts',(4.71254069815443,-4.85992248226018,44.4422815367569));
#19711=CARTESIAN_POINT('Ctrl Pts',(4.84439326931456,-4.72850295733857,44.4510308802033));
#19712=CARTESIAN_POINT('Ctrl Pts',(4.97060959434834,-4.59187644221535,44.4597802236496));
#19713=CARTESIAN_POINT('Ctrl Pts',(5.09682496280656,-4.45525096256503,44.4685295007859));
#19714=CARTESIAN_POINT('Ctrl Pts',(5.21740397615984,-4.31341878218151,44.4772787779222));
#19715=CARTESIAN_POINT('Ctrl Pts',(5.33193710452082,-4.16686161438488,44.4860280550585));
#19716=CARTESIAN_POINT('Ctrl Pts',(5.44646940289518,-4.0203055086433,44.4947772687914));
#19717=CARTESIAN_POINT('Ctrl Pts',(5.55495572749788,-3.86902470979956,44.5035264825244));
#19718=CARTESIAN_POINT('Ctrl Pts',(5.65702762491568,-3.71353301465611,44.5122756962573));
#19719=CARTESIAN_POINT('Ctrl Pts',(5.75909881655263,-3.55804239466717,44.5210248494935));
#19720=CARTESIAN_POINT('Ctrl Pts',(5.85475551250888,-3.39834117619372,44.5297740027296));
#19721=CARTESIAN_POINT('Ctrl Pts',(5.94367283728196,-3.23497174691783,44.5385231559657));
#19722=CARTESIAN_POINT('Ctrl Pts',(6.03258957676404,-3.07160339300784,44.5472722516112));
#19723=CARTESIAN_POINT('Ctrl Pts',(6.11476689685368,-2.90456712829328,44.5560213472568));
#19724=CARTESIAN_POINT('Ctrl Pts',(6.18992570525336,-2.73443024475734,44.5647704429023));
#19725=CARTESIAN_POINT('Ctrl Pts',(6.26508404388763,-2.56429442462869,44.5735194838633));
#19726=CARTESIAN_POINT('Ctrl Pts',(6.33322384283372,-2.39105828655842,44.5822685248243));
#19727=CARTESIAN_POINT('Ctrl Pts',(6.39411368720081,-2.21531017131941,44.5910175657854));
#19728=CARTESIAN_POINT('Ctrl Pts',(6.45500317120933,-2.03956309619377,44.5997665549678));
#19729=CARTESIAN_POINT('Ctrl Pts',(6.50864269270112,-1.86130434438497,44.6085155441502));
#19730=CARTESIAN_POINT('Ctrl Pts',(6.55485008446368,-1.68113930719811,44.6172645333326));
#19731=CARTESIAN_POINT('Ctrl Pts',(6.60199664749434,-1.49731239211706,44.6261913468619));
#19732=CARTESIAN_POINT('Ctrl Pts',(6.64140563640933,-1.31150116499538,44.6351181603913));
#19733=CARTESIAN_POINT('Ctrl Pts',(6.67293772282195,-1.12436255155527,44.6440449739207));
#19734=CARTESIAN_POINT('Ctrl Pts',(6.7038449494989,-0.940932395050006,44.6527948880762));
#19735=CARTESIAN_POINT('Ctrl Pts',(6.72718449348945,-0.756227260505368,
44.6615448022317));
#19736=CARTESIAN_POINT('Ctrl Pts',(6.74287707373944,-0.570874564540339,
44.6702947163872));
#19737=CARTESIAN_POINT('Ctrl Pts',(6.75856934538678,-0.385525513631136,
44.6790444584712));
#19738=CARTESIAN_POINT('Ctrl Pts',(6.76661493004107,-0.199529212416906,
44.6877942005552));
#19739=CARTESIAN_POINT('Ctrl Pts',(6.76698649908907,-0.0135174385991209,
44.6965439426392));
#19740=CARTESIAN_POINT('Ctrl Pts',(6.76735806132386,0.172490924447099,44.7052935242851));
#19741=CARTESIAN_POINT('Ctrl Pts',(6.76005588896282,0.35851447290274,44.714043105931));
#19742=CARTESIAN_POINT('Ctrl Pts',(6.74510478454574,0.543921359663555,44.7227926875769));
#19743=CARTESIAN_POINT('Ctrl Pts',(6.73015393440673,0.729325093151777,44.7315421204159));
#19744=CARTESIAN_POINT('Ctrl Pts',(6.70755443556879,0.914111900257673,44.740291553255));
#19745=CARTESIAN_POINT('Ctrl Pts',(6.67738304682297,1.09765415591669,44.749040986094));
#19746=CARTESIAN_POINT('Ctrl Pts',(6.64721213111835,1.28119353391405,44.7577902817553));
#19747=CARTESIAN_POINT('Ctrl Pts',(6.60946960955465,1.46348811672786,44.7665395774167));
#19748=CARTESIAN_POINT('Ctrl Pts',(6.5642836699115,1.64391876348355,44.775288873078));
#19749=CARTESIAN_POINT('Ctrl Pts',(6.51909837867681,1.82434682109845,44.7840380431888));
#19750=CARTESIAN_POINT('Ctrl Pts',(6.46646995271882,2.00291071820571,44.7927872132996));
#19751=CARTESIAN_POINT('Ctrl Pts',(6.40657713281508,2.17900400212826,44.8015363834105));
#19752=CARTESIAN_POINT('Ctrl Pts',(6.34668509279017,2.35509499309773,44.8102854395962));
#19753=CARTESIAN_POINT('Ctrl Pts',(6.27952894037483,2.52871516398229,44.819034495782));
#19754=CARTESIAN_POINT('Ctrl Pts',(6.20533675061404,2.69927486771518,44.8277835519678));
#19755=CARTESIAN_POINT('Ctrl Pts',(6.12832117907873,2.87632521636016,44.83686555325));
#19756=CARTESIAN_POINT('Ctrl Pts',(6.04372366626035,3.05007728920084,44.8459475545323));
#19757=CARTESIAN_POINT('Ctrl Pts',(5.95185378007824,3.21989527478277,44.8550295558146));
#19758=CARTESIAN_POINT('Ctrl Pts',(5.86334450817324,3.38350129286833,44.8637793361217));
#19759=CARTESIAN_POINT('Ctrl Pts',(5.76808562057205,3.54345567125044,44.8725291164288));
#19760=CARTESIAN_POINT('Ctrl Pts',(5.66640068804431,3.69921508465391,44.8812788967359));
#19761=CARTESIAN_POINT('Ctrl Pts',(5.56471941107868,3.85496889852363,44.8900283624894));
#19762=CARTESIAN_POINT('Ctrl Pts',(5.45661270815056,4.00652780919715,44.8987778282429));
#19763=CARTESIAN_POINT('Ctrl Pts',(5.34244776449055,4.15337704569305,44.9075272939964));
#19764=CARTESIAN_POINT('Ctrl Pts',(5.22828631819535,4.30022178356323,44.916276491716));
#19765=CARTESIAN_POINT('Ctrl Pts',(5.10806717844008,4.4423569097275,44.9250256894356));
#19766=CARTESIAN_POINT('Ctrl Pts',(4.98219864544657,4.57929969070713,44.9337748871552));
#19767=CARTESIAN_POINT('Ctrl Pts',(4.85633329943962,4.71623900430066,44.9425238633454));
#19768=CARTESIAN_POINT('Ctrl Pts',(4.72481904033584,4.84798602483679,44.9512728395357));
#19769=CARTESIAN_POINT('Ctrl Pts',(4.58810250737134,4.97409332259185,44.9600218157259));
#19770=CARTESIAN_POINT('Ctrl Pts',(4.45137708685576,5.10020881822193,44.9687713606621));
#19771=CARTESIAN_POINT('Ctrl Pts',(4.30944892635983,5.2206836630799,44.9775209055983));
#19772=CARTESIAN_POINT('Ctrl Pts',(4.1628000946659,5.33510865604906,44.9862704505344));
#19773=CARTESIAN_POINT('Ctrl Pts',(4.01615988348713,5.44952692272947,44.9950194811427));
#19774=CARTESIAN_POINT('Ctrl Pts',(3.8647997823215,5.55789587288682,45.003768511751));
#19775=CARTESIAN_POINT('Ctrl Pts',(3.70923383580982,5.65984746713934,45.0125175423593));
#19776=CARTESIAN_POINT('Ctrl Pts',(3.55366577799451,5.76180044505438,45.0212666917073));
#19777=CARTESIAN_POINT('Ctrl Pts',(3.39389200026746,5.85733573571114,45.0300158410553));
#19778=CARTESIAN_POINT('Ctrl Pts',(3.23045513625943,5.94612887621981,45.0387649904033));
#19779=CARTESIAN_POINT('Ctrl Pts',(3.18695122151514,5.96976399206722,45.0410938545163));
#19780=CARTESIAN_POINT('Ctrl Pts',(3.14318791262633,5.99292165435349,45.0434227186292));
#19781=CARTESIAN_POINT('Ctrl Pts',(3.09917575053261,6.01559628526638,45.0457515827422));
#19782=CARTESIAN_POINT('Ctrl Pts',(3.09917575053267,6.01559628526635,43.0458827467338));
#19783=CARTESIAN_POINT('Ctrl Pts',(2.94523624461966,6.09490439723907,43.0540047924677));
#19784=CARTESIAN_POINT('Ctrl Pts',(2.78817827432546,6.16833687487766,43.0621268382015));
#19785=CARTESIAN_POINT('Ctrl Pts',(2.62849662845226,6.2356470774263,43.0702488839354));
#19786=CARTESIAN_POINT('Ctrl Pts',(2.46882253523766,6.30295409632176,43.0783705455109));
#19787=CARTESIAN_POINT('Ctrl Pts',(2.30652534672956,6.36413926578448,43.0864922070864));
#19788=CARTESIAN_POINT('Ctrl Pts',(2.14212130073705,6.41900345325726,43.0946138686619));
#19789=CARTESIAN_POINT('Ctrl Pts',(1.97771293322712,6.47386908288762,43.1027357437231));
#19790=CARTESIAN_POINT('Ctrl Pts',(1.81119794486564,6.52241328294052,43.1108576187842));
#19791=CARTESIAN_POINT('Ctrl Pts',(1.64310903459608,6.56448640035371,43.1189794938454));
#19792=CARTESIAN_POINT('Ctrl Pts',(1.4749836981359,6.60656863534277,43.1271031289808));
#19793=CARTESIAN_POINT('Ctrl Pts',(1.30528411553005,6.64217690616454,43.1352267641163));
#19794=CARTESIAN_POINT('Ctrl Pts',(1.13455446400562,6.67121242115741,43.1433503992517));
#19795=CARTESIAN_POINT('Ctrl Pts',(0.963755300768497,6.70025975781312,43.151477341884));
#19796=CARTESIAN_POINT('Ctrl Pts',(0.791925593920185,6.72272894853215,43.1596042845164));
#19797=CARTESIAN_POINT('Ctrl Pts',(0.619615901835754,6.73857293009375,43.1677312271487));
#19798=CARTESIAN_POINT('Ctrl Pts',(0.447103370332945,6.75443556286392,43.1758677366504));
#19799=CARTESIAN_POINT('Ctrl Pts',(0.274110089669046,6.76365737737787,43.1840042461521));
#19800=CARTESIAN_POINT('Ctrl Pts',(0.101188800426362,6.76624340581007,43.1921407556538));
#19801=CARTESIAN_POINT('Ctrl Pts',(-0.0718453686045659,6.76883112235334,
43.2002825765169));
#19802=CARTESIAN_POINT('Ctrl Pts',(-0.244807087985825,6.76477443114987,
43.2084243973801));
#19803=CARTESIAN_POINT('Ctrl Pts',(-0.417147791540064,6.75413034520457,
43.2165662182432));
#19804=CARTESIAN_POINT('Ctrl Pts',(-0.589746847604112,6.74347030292243,
43.2247202443476));
#19805=CARTESIAN_POINT('Ctrl Pts',(-0.761722665787755,6.72620317980963,
43.232874270452));
#19806=CARTESIAN_POINT('Ctrl Pts',(-0.932534917209093,6.70243743933398,
43.2410282965563));
#19807=CARTESIAN_POINT('Ctrl Pts',(-1.03325554186012,6.68842380620121,43.2458363744068));
#19808=CARTESIAN_POINT('Ctrl Pts',(-1.13357182950383,6.67215159794002,43.2506444522573));
#19809=CARTESIAN_POINT('Ctrl Pts',(-1.23337550007314,6.65365116878089,43.2554525301078));
#19810=CARTESIAN_POINT('Ctrl Pts',(-1.40424649873686,6.62197711523061,43.2636843021386));
#19811=CARTESIAN_POINT('Ctrl Pts',(-1.57414743562728,6.58367018517124,43.2719160741694));
#19812=CARTESIAN_POINT('Ctrl Pts',(-1.74252458728602,6.53879935941635,43.2801478462002));
#19813=CARTESIAN_POINT('Ctrl Pts',(-1.91070067979916,6.49398211391152,43.2883697886726));
#19814=CARTESIAN_POINT('Ctrl Pts',(-2.07735626741041,6.44261667123134,43.296591731145));
#19815=CARTESIAN_POINT('Ctrl Pts',(-2.24194537073223,6.38482340825902,43.3048136736174));
#19816=CARTESIAN_POINT('Ctrl Pts',(-2.40637091509038,6.32708757682991,43.3130274456073));
#19817=CARTESIAN_POINT('Ctrl Pts',(-2.56873372905258,6.26293676385857,43.3212412175972));
#19818=CARTESIAN_POINT('Ctrl Pts',(-2.72850052018119,6.19254179730513,43.329454989587));
#19819=CARTESIAN_POINT('Ctrl Pts',(-2.88814054352925,6.12220268599925,43.3376622443174));
#19820=CARTESIAN_POINT('Ctrl Pts',(-3.04518832035738,6.04562943313532,43.3458694990477));
#19821=CARTESIAN_POINT('Ctrl Pts',(-3.19912807143316,5.96304189005648,43.354076753778));
#19822=CARTESIAN_POINT('Ctrl Pts',(-3.35297650216819,5.88050333966812,43.3622791397899));
#19823=CARTESIAN_POINT('Ctrl Pts',(-3.50372026521591,5.79195777549586,43.3704815258019));
#19824=CARTESIAN_POINT('Ctrl Pts',(-3.65086575693661,5.69767217597043,43.3786839118138));
#19825=CARTESIAN_POINT('Ctrl Pts',(-3.79796732929761,5.60341471840921,43.3868838496125));
#19826=CARTESIAN_POINT('Ctrl Pts',(-3.94147246628386,5.50342082804556,43.3950837874112));
#19827=CARTESIAN_POINT('Ctrl Pts',(-4.08091406165074,5.39800235470691,43.4032837252099));
#19828=CARTESIAN_POINT('Ctrl Pts',(-4.22033615948397,5.29259862159139,43.4114825164456));
#19829=CARTESIAN_POINT('Ctrl Pts',(-4.3556955610149,5.18177203157267,43.4196813076814));
#19830=CARTESIAN_POINT('Ctrl Pts',(-4.48655593213868,5.06587651525294,43.4278800989172));
#19831=CARTESIAN_POINT('Ctrl Pts',(-4.61742174435583,4.94997618006924,43.4360792310536));
#19832=CARTESIAN_POINT('Ctrl Pts',(-4.74378788509258,4.82900673628776,43.44427836319));
#19833=CARTESIAN_POINT('Ctrl Pts',(-4.86525273595378,4.70336101264769,43.4524774953264));
#19834=CARTESIAN_POINT('Ctrl Pts',(-4.98674467152199,4.57768727203325,43.4606784557374));
#19835=CARTESIAN_POINT('Ctrl Pts',(-5.10333289138271,4.44733543237846,43.4688794161483));
#19836=CARTESIAN_POINT('Ctrl Pts',(-5.21465409925935,4.31273366034557,43.4770803765593));
#19837=CARTESIAN_POINT('Ctrl Pts',(-5.32607964190557,4.17800573405026,43.4852890232443));
#19838=CARTESIAN_POINT('Ctrl Pts',(-5.43222808109294,4.03902019373569,43.4934976699294));
#19839=CARTESIAN_POINT('Ctrl Pts',(-5.53277717272509,3.89623738457658,43.5017063166144));
#19840=CARTESIAN_POINT('Ctrl Pts',(-5.6333742693174,3.75338640689447,43.5099188823379));
#19841=CARTESIAN_POINT('Ctrl Pts',(-5.72836649351828,3.60673484638128,43.5181314480614));
#19842=CARTESIAN_POINT('Ctrl Pts',(-5.81747616663442,3.45677017613849,43.5263440137849));
#19843=CARTESIAN_POINT('Ctrl Pts',(-5.90670811108098,3.30659973272758,43.5345678483337));
#19844=CARTESIAN_POINT('Ctrl Pts',(-5.99004120164727,3.15310740915804,43.5427916828824));
#19845=CARTESIAN_POINT('Ctrl Pts',(-6.06724421044289,2.99680441317869,43.5510155174312));
#19846=CARTESIAN_POINT('Ctrl Pts',(-6.13817925295864,2.85319136184688,43.5585716744057));
#19847=CARTESIAN_POINT('Ctrl Pts',(-6.20393965309091,2.70720593898942,43.5661278313801));
#19848=CARTESIAN_POINT('Ctrl Pts',(-6.26438279490053,2.55925715764443,43.5736839883546));
#19849=CARTESIAN_POINT('Ctrl Pts',(-6.33711745157415,2.38122200767981,43.582776740102));
#19850=CARTESIAN_POINT('Ctrl Pts',(-6.40230502939274,2.19997039809362,43.5918694918494));
#19851=CARTESIAN_POINT('Ctrl Pts',(-6.45968401808883,2.01612781996773,43.6009622435968));
#19852=CARTESIAN_POINT('Ctrl Pts',(-6.51689443909958,1.83282533358212,43.6100282827069));
#19853=CARTESIAN_POINT('Ctrl Pts',(-6.56634198463486,1.64694728694844,43.619094321817));
#19854=CARTESIAN_POINT('Ctrl Pts',(-6.60781461466737,1.45913502397426,43.6281603609271));
#19855=CARTESIAN_POINT('Ctrl Pts',(-6.64920538668722,1.27169346183549,43.6372085056344));
#19856=CARTESIAN_POINT('Ctrl Pts',(-6.68265259622375,1.08232552107935,43.6462566503418));
#19857=CARTESIAN_POINT('Ctrl Pts',(-6.70799399247436,0.891686938856826,
43.6553047950491));
#19858=CARTESIAN_POINT('Ctrl Pts',(-6.73325265009385,0.701670783874526,
43.6643233979309));
#19859=CARTESIAN_POINT('Ctrl Pts',(-6.75045826143766,0.510392489687212,
43.6733420008127));
#19860=CARTESIAN_POINT('Ctrl Pts',(-6.75949971433177,0.318516266380099,
43.6823606036945));
#19861=CARTESIAN_POINT('Ctrl Pts',(-6.76445195659145,0.213420597264003,
43.6873003303997));
#19862=CARTESIAN_POINT('Ctrl Pts',(-6.76695579227593,0.108145788607282,
43.6922400571048));
#19863=CARTESIAN_POINT('Ctrl Pts',(-6.76699941967512,0.00280251968678848,
43.69717978381));
#19864=CARTESIAN_POINT('',(-6.76699727772403,0.00606986618896983,43.3028202161432));
#19865=CARTESIAN_POINT('Ctrl Pts',(3.09917575053259,6.01559628526639,42.6516693621546));
#19866=CARTESIAN_POINT('Ctrl Pts',(2.94547762866111,6.09478003856665,42.6598019609222));
#19867=CARTESIAN_POINT('Ctrl Pts',(2.78859575421918,6.16814523834569,42.6679345596898));
#19868=CARTESIAN_POINT('Ctrl Pts',(2.62901526227188,6.23542843361557,42.6760671584574));
#19869=CARTESIAN_POINT('Ctrl Pts',(2.46953836527548,6.30266795061861,42.6841944777817));
#19870=CARTESIAN_POINT('Ctrl Pts',(2.30736667512768,6.36383318397364,42.692321797106));
#19871=CARTESIAN_POINT('Ctrl Pts',(2.14300853510284,6.41870730119986,42.7004491164302));
#19872=CARTESIAN_POINT('Ctrl Pts',(1.97197764007607,6.47580924565839,42.7089063957471));
#19873=CARTESIAN_POINT('Ctrl Pts',(1.79857940220122,6.52609835618054,42.717363675064));
#19874=CARTESIAN_POINT('Ctrl Pts',(1.62340864502557,6.56938607262933,42.7258209543809));
#19875=CARTESIAN_POINT('Ctrl Pts',(1.45515793721862,6.61096372548239,42.7339441323253));
#19876=CARTESIAN_POINT('Ctrl Pts',(1.28527245991803,6.64608247726379,42.7420673102697));
#19877=CARTESIAN_POINT('Ctrl Pts',(1.11429343029639,6.67462651773103,42.750190488214));
#19878=CARTESIAN_POINT('Ctrl Pts',(0.943309450257023,6.70317138464421,42.7583139013517));
#19879=CARTESIAN_POINT('Ctrl Pts',(0.771232215586851,6.72514110037779,42.7664373144894));
#19880=CARTESIAN_POINT('Ctrl Pts',(0.598611430890102,6.74047130064417,42.7745607276271));
#19881=CARTESIAN_POINT('Ctrl Pts',(0.425952807857227,6.75580486127803,42.7826859214104));
#19882=CARTESIAN_POINT('Ctrl Pts',(0.252750761859558,6.76449597610237,42.7908111151937));
#19883=CARTESIAN_POINT('Ctrl Pts',(0.0795583495546547,6.76653230754248,
42.7989363089769));
#19884=CARTESIAN_POINT('Ctrl Pts',(-0.0937049778566374,6.76856947277582,
42.8070648296899));
#19885=CARTESIAN_POINT('Ctrl Pts',(-0.266958298377293,6.76394642463658,
42.8151933504029));
#19886=CARTESIAN_POINT('Ctrl Pts',(-0.439650370402464,6.75270290711838,
42.8233218711159));
#19887=CARTESIAN_POINT('Ctrl Pts',(-0.612534460621611,6.7414468878107,42.8314594300195));
#19888=CARTESIAN_POINT('Ctrl Pts',(-0.784855691413282,6.72355572461415,
42.8395969889231));
#19889=CARTESIAN_POINT('Ctrl Pts',(-0.956068947050589,6.6991209250532,42.8477345478267));
#19890=CARTESIAN_POINT('Ctrl Pts',(-1.12739465151351,6.67467007729256,42.8558774512869));
#19891=CARTESIAN_POINT('Ctrl Pts',(-1.29761057262233,6.64366709610046,42.8640203547472));
#19892=CARTESIAN_POINT('Ctrl Pts',(-1.46618386057521,6.60625414943967,42.8721632582074));
#19893=CARTESIAN_POINT('Ctrl Pts',(-1.63498327105339,6.56879101742578,42.880317084477));
#19894=CARTESIAN_POINT('Ctrl Pts',(-1.80213529769376,6.52490084712561,42.8884709107467));
#19895=CARTESIAN_POINT('Ctrl Pts',(-1.96712352916672,6.47477521007476,42.8966247370163));
#19896=CARTESIAN_POINT('Ctrl Pts',(-2.01298210917268,6.46084275855065,42.8988910980228));
#19897=CARTESIAN_POINT('Ctrl Pts',(-2.05867364890705,6.44642885910712,42.9011574590293));
#19898=CARTESIAN_POINT('Ctrl Pts',(-2.10418736768364,6.43153827024924,42.9034238200358));
#19899=CARTESIAN_POINT('Ctrl Pts',(-2.26938848846164,6.37748990781063,42.9116500293728));
#19900=CARTESIAN_POINT('Ctrl Pts',(-2.4327367662887,6.31699684427263,42.9198762387097));
#19901=CARTESIAN_POINT('Ctrl Pts',(-2.59369317001151,6.2502035758714,42.9281024480467));
#19902=CARTESIAN_POINT('Ctrl Pts',(-2.75446874610995,6.18348534684587,42.9363194155899));
#19903=CARTESIAN_POINT('Ctrl Pts',(-2.91285747074717,6.1104811434104,42.9445363831331));
#19904=CARTESIAN_POINT('Ctrl Pts',(-3.06833511080451,6.03138530089102,42.9527533506763));
#19905=CARTESIAN_POINT('Ctrl Pts',(-3.22366928400182,5.95236244399301,42.9609627360197));
#19906=CARTESIAN_POINT('Ctrl Pts',(-3.37609740464669,5.86725930414412,42.969172121363));
#19907=CARTESIAN_POINT('Ctrl Pts',(-3.5251148041122,5.77631843113146,42.9773815067064));
#19908=CARTESIAN_POINT('Ctrl Pts',(-3.6740245972852,5.68544322702873,42.985584964007));
#19909=CARTESIAN_POINT('Ctrl Pts',(-3.81952827006225,5.58873887230033,42.9937884213076));
#19910=CARTESIAN_POINT('Ctrl Pts',(-3.96114530187512,5.4864940442356,43.0019918786082));
#19911=CARTESIAN_POINT('Ctrl Pts',(-4.10268847927094,5.38430253766812,43.0101910577401));
#19912=CARTESIAN_POINT('Ctrl Pts',(-4.24034876359638,5.2765765233987,43.0183902368719));
#19913=CARTESIAN_POINT('Ctrl Pts',(-4.37367413811537,5.16364827748568,43.0265894160038));
#19914=CARTESIAN_POINT('Ctrl Pts',(-4.50697439126041,5.05074130968799,43.0347870502336));
#19915=CARTESIAN_POINT('Ctrl Pts',(-4.63594108416167,4.9326342895393,43.0429846844634));
#19916=CARTESIAN_POINT('Ctrl Pts',(-4.76015462476693,4.80970029714014,43.0511823186932));
#19917=CARTESIAN_POINT('Ctrl Pts',(-4.88435919950286,4.68677517825113,43.0593793612088));
#19918=CARTESIAN_POINT('Ctrl Pts',(-5.00381104966564,4.55902403268096,43.0675764037244));
#19919=CARTESIAN_POINT('Ctrl Pts',(-5.11812691275048,4.42685733957841,43.07577344624));
#19920=CARTESIAN_POINT('Ctrl Pts',(-5.23245530110767,4.29467616533753,43.0839713868828));
#19921=CARTESIAN_POINT('Ctrl Pts',(-5.34164634656284,4.15807875103507,43.0921693275256));
#19922=CARTESIAN_POINT('Ctrl Pts',(-5.44535657900357,4.01750926912466,43.1003672681685));
#19923=CARTESIAN_POINT('Ctrl Pts',(-5.54909702391801,3.87689883704302,43.1085675970044));
#19924=CARTESIAN_POINT('Ctrl Pts',(-5.64735326259328,3.73231432104986,43.1167679258404));
#19925=CARTESIAN_POINT('Ctrl Pts',(-5.73982469281005,3.58422955400572,43.1249682546764));
#19926=CARTESIAN_POINT('Ctrl Pts',(-5.83239248065666,3.43599047879164,43.1331771284678));
#19927=CARTESIAN_POINT('Ctrl Pts',(-5.91916322694038,3.28424417030447,43.1413860022592));
#19928=CARTESIAN_POINT('Ctrl Pts',(-5.99988143240041,3.12949066097613,43.1495948760507));
#19929=CARTESIAN_POINT('Ctrl Pts',(-6.08064295843088,2.97465409714647,43.1578081554541));
#19930=CARTESIAN_POINT('Ctrl Pts',(-6.15534531468992,2.81680743893843,43.1660214348575));
#19931=CARTESIAN_POINT('Ctrl Pts',(-6.22378091914611,2.65647135698331,43.1742347142609));
#19932=CARTESIAN_POINT('Ctrl Pts',(-6.29231662142997,2.49590075830803,43.1824600068764));
#19933=CARTESIAN_POINT('Ctrl Pts',(-6.35456712612489,2.33283379430901,43.1906852994918));
#19934=CARTESIAN_POINT('Ctrl Pts',(-6.41037414202956,2.16780819243741,43.1989105921073));
#19935=CARTESIAN_POINT('Ctrl Pts',(-6.46084488412926,2.01856235915123,43.2063493812193));
#19936=CARTESIAN_POINT('Ctrl Pts',(-6.50604607878305,1.8677149212602,43.2137881703314));
#19937=CARTESIAN_POINT('Ctrl Pts',(-6.54589673199735,1.71567041532643,43.2212269594435));
#19938=CARTESIAN_POINT('Ctrl Pts',(-6.60234368379457,1.50030508991207,43.2317637245043));
#19939=CARTESIAN_POINT('Ctrl Pts',(-6.64818382531231,1.28205434231952,43.2423004895651));
#19940=CARTESIAN_POINT('Ctrl Pts',(-6.68317317027446,1.06183114294304,43.2528372546259));
#19941=CARTESIAN_POINT('Ctrl Pts',(-6.71756478004758,0.845370093325244,
43.2631940164525));
#19942=CARTESIAN_POINT('Ctrl Pts',(-6.7414732007806,0.627003238492665,43.2735507782791));
#19943=CARTESIAN_POINT('Ctrl Pts',(-6.75471215089131,0.40761839826148,43.2839075401057));
#19944=CARTESIAN_POINT('Ctrl Pts',(-6.76277078217368,0.27407748137766,43.2902117654515));
#19945=CARTESIAN_POINT('Ctrl Pts',(-6.76687700164212,0.140159793959005,
43.2965159907974));
#19946=CARTESIAN_POINT('Ctrl Pts',(-6.76699727772403,0.0060698661890735,
43.3028202161432));
#19947=CARTESIAN_POINT('Ctrl Pts',(-6.76699727772492,0.00606986519518309,
43.3028202161899));
#19948=CARTESIAN_POINT('Ctrl Pts',(-6.76715235655782,-0.166819977707758,
43.3109486158973));
#19949=CARTESIAN_POINT('Ctrl Pts',(-6.76067749336114,-0.339861581287961,
43.3190770156048));
#19950=CARTESIAN_POINT('Ctrl Pts',(-6.7475647088073,-0.512503171169026,
43.3272054153122));
#19951=CARTESIAN_POINT('Ctrl Pts',(-6.7344591306595,-0.685049882239841,
43.3353293478869));
#19952=CARTESIAN_POINT('Ctrl Pts',(-6.71472292397814,-0.85719665330725,
43.3434532804617));
#19953=CARTESIAN_POINT('Ctrl Pts',(-6.68840018265249,-1.02839291941074,
43.3515772130364));
#19954=CARTESIAN_POINT('Ctrl Pts',(-6.66208305724268,-1.19955266105763,
43.3596994123828));
#19955=CARTESIAN_POINT('Ctrl Pts',(-6.62918224502249,-1.36976193915329,
43.3678216117292));
#19956=CARTESIAN_POINT('Ctrl Pts',(-6.58979359439325,-1.53847631873022,
43.3759438110755));
#19957=CARTESIAN_POINT('Ctrl Pts',(-6.55040804042411,-1.70717743430651,
43.3840653718702));
#19958=CARTESIAN_POINT('Ctrl Pts',(-6.50453574599593,-1.87438352856006,
43.3921869326648));
#19959=CARTESIAN_POINT('Ctrl Pts',(-6.45232345152619,-2.03956149132238,
43.4003084934595));
#19960=CARTESIAN_POINT('Ctrl Pts',(-6.40010530233302,-2.2047579759922,43.4084309649495));
#19961=CARTESIAN_POINT('Ctrl Pts',(-6.34154584781495,-2.36792552707013,
43.4165534364394));
#19962=CARTESIAN_POINT('Ctrl Pts',(-6.27684134802887,-2.5285473481181,43.4246759079294));
#19963=CARTESIAN_POINT('Ctrl Pts',(-6.21211724954308,-2.68921782078769,
43.4328008396792));
#19964=CARTESIAN_POINT('Ctrl Pts',(-6.14124453662508,-2.84734068862425,
43.440925771429));
#19965=CARTESIAN_POINT('Ctrl Pts',(-6.06446711525331,-3.00242029169988,
43.4490507031788));
#19966=CARTESIAN_POINT('Ctrl Pts',(-5.98760984615137,-3.15766117597095,
43.4571840847742));
#19967=CARTESIAN_POINT('Ctrl Pts',(-5.90483576632286,-3.3098521457591,43.4653174663696));
#19968=CARTESIAN_POINT('Ctrl Pts',(-5.81643455838062,-3.45852252097274,
43.473450847965));
#19969=CARTESIAN_POINT('Ctrl Pts',(-5.72798356075828,-3.6072766309067,43.4815888104759));
#19970=CARTESIAN_POINT('Ctrl Pts',(-5.63389931864332,-3.75250588857054,
43.4897267729869));
#19971=CARTESIAN_POINT('Ctrl Pts',(-5.53451396175305,-3.89376992221684,
43.4978647354978));
#19972=CARTESIAN_POINT('Ctrl Pts',(-5.43498826531216,-4.03523343123478,
43.50601418942));
#19973=CARTESIAN_POINT('Ctrl Pts',(-5.33014672314952,-4.1727202412223,43.5141636433421));
#19974=CARTESIAN_POINT('Ctrl Pts',(-5.22036137774323,-4.30582350843213,
43.5223130972642));
#19975=CARTESIAN_POINT('Ctrl Pts',(-5.14529369791631,-4.39683523144351,
43.5278854311265));
#19976=CARTESIAN_POINT('Ctrl Pts',(-5.06791540253621,-4.48579821978216,
43.5334577649888));
#19977=CARTESIAN_POINT('Ctrl Pts',(-4.98835480509962,-4.57259284634436,
43.5390300988511));
#19978=CARTESIAN_POINT('Ctrl Pts',(-4.87195434184831,-4.69957699509482,
43.5471826550644));
#19979=CARTESIAN_POINT('Ctrl Pts',(-4.75051986269689,-4.82231220563415,
43.5553352112776));
#19980=CARTESIAN_POINT('Ctrl Pts',(-4.62439552489982,-4.94036992838457,
43.5634877674909));
#19981=CARTESIAN_POINT('Ctrl Pts',(-4.4984173051886,-5.05829087841713,43.5716308787712));
#19982=CARTESIAN_POINT('Ctrl Pts',(-4.3677603065204,-5.17154488040067,43.5797739900516));
#19983=CARTESIAN_POINT('Ctrl Pts',(-4.23280838067924,-5.27973694538389,
43.5879171013319));
#19984=CARTESIAN_POINT('Ctrl Pts',(-4.09798442793581,-5.38782641328581,
43.5960524906093));
#19985=CARTESIAN_POINT('Ctrl Pts',(-3.958873939743,-5.49086327361666,43.6041878798866));
#19986=CARTESIAN_POINT('Ctrl Pts',(-3.81589699596826,-5.58848987796886,
43.612323269164));
#19987=CARTESIAN_POINT('Ctrl Pts',(-3.67302559240245,-5.6860444180291,43.6204526532026));
#19988=CARTESIAN_POINT('Ctrl Pts',(-3.52629371683801,-5.77819644889409,
43.6285820372412));
#19989=CARTESIAN_POINT('Ctrl Pts',(-3.37615384738565,-5.864629075976,43.6367114212798));
#19990=CARTESIAN_POINT('Ctrl Pts',(-3.22609326899139,-5.95101605672506,
43.6448365120719));
#19991=CARTESIAN_POINT('Ctrl Pts',(-3.07262859721654,-6.03168946716792,
43.652961602864));
#19992=CARTESIAN_POINT('Ctrl Pts',(-2.91624055427901,-6.106376178191,43.6610866936562));
#19993=CARTESIAN_POINT('Ctrl Pts',(-2.75925554427864,-6.18134798458118,
43.6692427996813));
#19994=CARTESIAN_POINT('Ctrl Pts',(-2.59932511257514,-6.25028709286662,
43.6773989057064));
#19995=CARTESIAN_POINT('Ctrl Pts',(-2.43696012126463,-6.31296399224373,
43.6855550117315));
#19996=CARTESIAN_POINT('Ctrl Pts',(-2.27524861968018,-6.37538862843606,
43.6936782909049));
#19997=CARTESIAN_POINT('Ctrl Pts',(-2.11112247080499,-6.43160125810205,
43.7018015700783));
#19998=CARTESIAN_POINT('Ctrl Pts',(-1.94510573082439,-6.48142366273909,
43.7099248492517));
#19999=CARTESIAN_POINT('Ctrl Pts',(-1.77906688431242,-6.53125270165018,
43.7180492101083));
#20000=CARTESIAN_POINT('Ctrl Pts',(-1.61113729568207,-6.57468971550923,
43.726173570965));
#20001=CARTESIAN_POINT('Ctrl Pts',(-1.4418553344958,-6.6116066273173,43.7342979318217));
#20002=CARTESIAN_POINT('Ctrl Pts',(-1.27251862522095,-6.64853547855674,
43.7424249202071));
#20003=CARTESIAN_POINT('Ctrl Pts',(-1.101829029676,-6.67893995077014,43.7505519085925));
#20004=CARTESIAN_POINT('Ctrl Pts',(-0.930334193544025,-6.70274326588172,
43.758678896978));
#20005=CARTESIAN_POINT('Ctrl Pts',(-0.757730662821797,-6.7267004667154,
43.7668584254181));
#20006=CARTESIAN_POINT('Ctrl Pts',(-0.584311816093609,-6.7439708114104,
43.7750379538581));
#20007=CARTESIAN_POINT('Ctrl Pts',(-0.410639352460591,-6.75452917102375,
43.7832174822982));
#20008=CARTESIAN_POINT('Ctrl Pts',(-0.237784768448134,-6.76503780791782,
43.7913584907019));
#20009=CARTESIAN_POINT('Ctrl Pts',(-0.0646793178176682,-6.76889759763473,
43.7994994991056));
#20010=CARTESIAN_POINT('Ctrl Pts',(0.108125414811876,-6.76613611263266,
43.8076405075093));
#20011=CARTESIAN_POINT('Ctrl Pts',(0.28215661305668,-6.76335502824606,43.8158392959675));
#20012=CARTESIAN_POINT('Ctrl Pts',(0.455882432014132,-6.75385835649914,
43.8240380844258));
#20013=CARTESIAN_POINT('Ctrl Pts',(0.628747328436504,-6.73772704975379,
43.832236872884));
#20014=CARTESIAN_POINT('Ctrl Pts',(0.801612224858811,-6.72159574300845,
43.8404356613423));
#20015=CARTESIAN_POINT('Ctrl Pts',(0.973615839090478,-6.69882991421583,
43.8486344498006));
#20016=CARTESIAN_POINT('Ctrl Pts',(1.14421600706632,-6.66956210925224,43.8568332382588));
#20017=CARTESIAN_POINT('Ctrl Pts',(1.31552909102076,-6.64017199792715,43.8650662883908));
#20018=CARTESIAN_POINT('Ctrl Pts',(1.48595952790044,-6.60413421298527,43.8732993385228));
#20019=CARTESIAN_POINT('Ctrl Pts',(1.65495256627668,-6.56151057328831,43.8815323886548));
#20020=CARTESIAN_POINT('Ctrl Pts',(1.82374435992116,-6.51893769179429,43.8897556344897));
#20021=CARTESIAN_POINT('Ctrl Pts',(1.99110181962276,-6.46979465911976,43.8979788803245));
#20022=CARTESIAN_POINT('Ctrl Pts',(2.15647727562801,-6.4141947865418,43.9062021261594));
#20023=CARTESIAN_POINT('Ctrl Pts',(2.32168889514025,-6.35864999643107,43.9144172252729));
#20024=CARTESIAN_POINT('Ctrl Pts',(2.48492208423485,-6.29666121898922,43.9226323243864));
#20025=CARTESIAN_POINT('Ctrl Pts',(2.64564120766742,-6.22839237687319,43.9308474234999));
#20026=CARTESIAN_POINT('Ctrl Pts',(2.8062332642672,-6.16017750907809,43.9390560276388));
#20027=CARTESIAN_POINT('Ctrl Pts',(2.96431488602863,-6.08569260551714,43.9472646317776));
#20028=CARTESIAN_POINT('Ctrl Pts',(3.1193673147187,-6.00515083539661,43.9554732359165));
#20029=CARTESIAN_POINT('Ctrl Pts',(3.27432817155355,-5.92465663214993,43.9636769921655));
#20030=CARTESIAN_POINT('Ctrl Pts',(3.42626308224412,-5.83811285308669,43.9718807484144));
#20031=CARTESIAN_POINT('Ctrl Pts',(3.57467485037603,-5.74578007881342,43.9800845046634));
#20032=CARTESIAN_POINT('Ctrl Pts',(3.723042707207,-5.65347462348047,43.9882858336277));
#20033=CARTESIAN_POINT('Ctrl Pts',(3.86788919213928,-5.55538377050031,43.9964871625919));
#20034=CARTESIAN_POINT('Ctrl Pts',(4.00874301933719,-5.45181331346877,44.0046884915562));
#20035=CARTESIAN_POINT('Ctrl Pts',(4.14957742144741,-5.34825713979219,44.0128886894789));
#20036=CARTESIAN_POINT('Ctrl Pts',(4.28641997345309,-5.23922307866104,44.0210888874016));
#20037=CARTESIAN_POINT('Ctrl Pts',(4.41882960990569,-5.12505940244801,44.0292890853243));
#20038=CARTESIAN_POINT('Ctrl Pts',(4.55124498112526,-5.01089078171511,44.0374896384041));
#20039=CARTESIAN_POINT('Ctrl Pts',(4.67922678288968,-4.89159233721435,44.045690191484));
#20040=CARTESIAN_POINT('Ctrl Pts',(4.80236815335128,-4.76755169029948,44.0538907445638));
#20041=CARTESIAN_POINT('Ctrl Pts',(4.92553717279321,-4.64348319248939,44.062093138917));
#20042=CARTESIAN_POINT('Ctrl Pts',(5.04386334391571,-4.51467062575975,44.0702955332702));
#20043=CARTESIAN_POINT('Ctrl Pts',(5.15697765972981,-4.38153744900664,44.0784979276235));
#20044=CARTESIAN_POINT('Ctrl Pts',(5.27019775731346,-4.24827976932992,44.0867079926573));
#20045=CARTESIAN_POINT('Ctrl Pts',(5.37819602945704,-4.11069368038182,44.0949180576911));
#20046=CARTESIAN_POINT('Ctrl Pts',(5.48064409712424,-3.96923535213739,44.103128122725));
#20047=CARTESIAN_POINT('Ctrl Pts',(5.58314119461901,-3.8277093244468,44.1113421169503));
#20048=CARTESIAN_POINT('Ctrl Pts',(5.68008259290995,-3.682307660451,44.1195561111755));
#20049=CARTESIAN_POINT('Ctrl Pts',(5.77118411546925,-3.53351424298183,44.1277701054008));
#20050=CARTESIAN_POINT('Ctrl Pts',(5.8624098397462,-3.38451797052729,44.135995298036));
#20051=CARTESIAN_POINT('Ctrl Pts',(5.9477796015865,-3.23212101596296,44.1442204906712));
#20052=CARTESIAN_POINT('Ctrl Pts',(6.02705536251554,-3.07683159389211,44.1524456833064));
#20053=CARTESIAN_POINT('Ctrl Pts',(6.09834788452548,-2.93718014922409,44.1598425814265));
#20054=CARTESIAN_POINT('Ctrl Pts',(6.16471252537249,-2.79518992302598,44.1672394795465));
#20055=CARTESIAN_POINT('Ctrl Pts',(6.22601009619027,-2.65124259209468,44.1746363776665));
#20056=CARTESIAN_POINT('Ctrl Pts',(6.29765860812913,-2.48298776696532,44.1832823441574));
#20057=CARTESIAN_POINT('Ctrl Pts',(6.36254645794287,-2.3116769900004,44.1919283106483));
#20058=CARTESIAN_POINT('Ctrl Pts',(6.42042117281807,-2.13786832233172,44.2005742771392));
#20059=CARTESIAN_POINT('Ctrl Pts',(6.47822185806526,-1.96428197957712,44.2092091842636));
#20060=CARTESIAN_POINT('Ctrl Pts',(6.52902720070417,-1.78820440536733,44.217844091388));
#20061=CARTESIAN_POINT('Ctrl Pts',(6.57263275044773,-1.61021356587936,44.2264789985124));
#20062=CARTESIAN_POINT('Ctrl Pts',(6.61768596924769,-1.42631357418107,44.2354005775839));
#20063=CARTESIAN_POINT('Ctrl Pts',(6.6550529727088,-1.24037137989682,44.2443221566554));
#20064=CARTESIAN_POINT('Ctrl Pts',(6.68456328737994,-1.05304447057679,44.2532437357268));
#20065=CARTESIAN_POINT('Ctrl Pts',(6.71304648054431,-0.872237569582721,
44.2618547947025));
#20066=CARTESIAN_POINT('Ctrl Pts',(6.73421058578448,-0.690141055066458,
44.2704658536782));
#20067=CARTESIAN_POINT('Ctrl Pts',(6.74795340358676,-0.507359697869109,
44.2790769126539));
#20068=CARTESIAN_POINT('Ctrl Pts',(6.76168326127738,-0.324750711930169,
44.2876798510034));
#20069=CARTESIAN_POINT('Ctrl Pts',(6.76800576214893,-0.141458474040101,
44.296282789353));
#20070=CARTESIAN_POINT('Ctrl Pts',(6.76687024857627,0.0419051182232875,
44.3048857277025));
#20071=CARTESIAN_POINT('Ctrl Pts',(6.76573600651614,0.225063385681669,44.3134790327512));
#20072=CARTESIAN_POINT('Ctrl Pts',(6.75716041240889,0.408292543811773,44.3220723378));
#20073=CARTESIAN_POINT('Ctrl Pts',(6.74114481887468,0.590978452195285,44.3306656428487));
#20074=CARTESIAN_POINT('Ctrl Pts',(6.7393604196064,0.611332652652995,44.3316230776892));
#20075=CARTESIAN_POINT('Ctrl Pts',(6.73748371635307,0.631680107803456,44.3325805125297));
#20076=CARTESIAN_POINT('Ctrl Pts',(6.735514751076,0.652019967514503,44.3335379473702));
#20077=CARTESIAN_POINT('Ctrl Pts',(6.71783757094296,0.834629263971174,44.3421337049178));
#20078=CARTESIAN_POINT('Ctrl Pts',(6.69274026974788,1.01641209288584,44.3507294624654));
#20079=CARTESIAN_POINT('Ctrl Pts',(6.66033376041236,1.19676363577414,44.359325220013));
#20080=CARTESIAN_POINT('Ctrl Pts',(6.62789701470164,1.37728345278487,44.3679289976947));
#20081=CARTESIAN_POINT('Ctrl Pts',(6.58813750239558,1.55636901769334,44.3765327753764));
#20082=CARTESIAN_POINT('Ctrl Pts',(6.54121685482633,1.73342754626088,44.385136553058));
#20083=CARTESIAN_POINT('Ctrl Pts',(6.49245218477855,1.91744462982725,44.3940784667261));
#20084=CARTESIAN_POINT('Ctrl Pts',(6.43595222804921,2.09927176573737,44.4030203803941));
#20085=CARTESIAN_POINT('Ctrl Pts',(6.37195427288985,2.27826419543494,44.4119622940621));
#20086=CARTESIAN_POINT('Ctrl Pts',(6.31020873067017,2.45095697284283,44.4205894963928));
#20087=CARTESIAN_POINT('Ctrl Pts',(6.24148413654294,2.62101092201237,44.4292166987236));
#20088=CARTESIAN_POINT('Ctrl Pts',(6.16604171145989,2.78786990595631,44.4378439010543));
#20089=CARTESIAN_POINT('Ctrl Pts',(6.09052743901424,2.95488779754286,44.4464793194748));
#20090=CARTESIAN_POINT('Ctrl Pts',(6.00828269922023,3.11870437662215,44.4551147378952));
#20091=CARTESIAN_POINT('Ctrl Pts',(5.91961443617632,3.27878848464077,44.4637501563157));
#20092=CARTESIAN_POINT('Ctrl Pts',(5.83081517840424,3.43910909412556,44.4723983323368));
#20093=CARTESIAN_POINT('Ctrl Pts',(5.73557358823278,3.59568595059942,44.4810465083579));
#20094=CARTESIAN_POINT('Ctrl Pts',(5.63424043766182,3.74801596723072,44.489694684379));
#20095=CARTESIAN_POINT('Ctrl Pts',(5.62351977455632,3.76413190540057,44.4906096286107));
#20096=CARTESIAN_POINT('Ctrl Pts',(5.61273096715472,3.78020033939302,44.4915245728425));
#20097=CARTESIAN_POINT('Ctrl Pts',(5.60187445720227,3.79622069507883,44.4924395170742));
#20098=CARTESIAN_POINT('Ctrl Pts',(5.50426680375573,3.94025495035235,44.5006655086577));
#20099=CARTESIAN_POINT('Ctrl Pts',(5.40097240507913,4.08071133054436,44.5088915002412));
#20100=CARTESIAN_POINT('Ctrl Pts',(5.29228213753906,4.21711261133551,44.5171174918247));
#20101=CARTESIAN_POINT('Ctrl Pts',(5.18370187668307,4.35337583880372,44.5253351577864));
#20102=CARTESIAN_POINT('Ctrl Pts',(5.06973684219314,4.48559186080498,44.5335528237481));
#20103=CARTESIAN_POINT('Ctrl Pts',(4.95072157811933,4.61331170158094,44.5417704897098));
#20104=CARTESIAN_POINT('Ctrl Pts',(4.83180519152927,4.74092543313991,44.5499813284621));
#20105=CARTESIAN_POINT('Ctrl Pts',(4.70784717391219,4.86405016171377,44.5581921672144));
#20106=CARTESIAN_POINT('Ctrl Pts',(4.57922282039794,4.98226929833653,44.5664030059667));
#20107=CARTESIAN_POINT('Ctrl Pts',(4.45069209100074,5.10040238467422,44.5746078681484));
#20108=CARTESIAN_POINT('Ctrl Pts',(4.31750205727295,5.21363675318523,44.5828127303301));
#20109=CARTESIAN_POINT('Ctrl Pts',(4.18006535127247,5.32159211694127,44.5910175925118));
#20110=CARTESIAN_POINT('Ctrl Pts',(4.0426867279238,5.42950185726825,44.5992189872053));
#20111=CARTESIAN_POINT('Ctrl Pts',(3.90106528814467,5.5321368156678,44.6074203818988));
#20112=CARTESIAN_POINT('Ctrl Pts',(3.7556474699345,5.62915633834899,44.6156217765923));
#20113=CARTESIAN_POINT('Ctrl Pts',(3.61025764095278,5.72615718724166,44.6238215927261));
#20114=CARTESIAN_POINT('Ctrl Pts',(3.46107318584336,5.81754455327705,44.6320214088599));
#20115=CARTESIAN_POINT('Ctrl Pts',(3.30857042086482,5.90302047854981,44.6402212249937));
#20116=CARTESIAN_POINT('Ctrl Pts',(3.23943832861813,5.94176816651244,44.643938340847));
#20117=CARTESIAN_POINT('Ctrl Pts',(3.16962471935677,5.9793016728163,44.6476554567003));
#20118=CARTESIAN_POINT('Ctrl Pts',(3.09917575053253,6.01559628526642,44.6513725725535));
#20119=CARTESIAN_POINT('Origin',(0.,0.,-3.69717978381041));
#20120=CARTESIAN_POINT('',(3.09917575053261,6.01559628526638,47.0456199604263));
#20121=CARTESIAN_POINT('',(3.09917575053265,6.01559628526636,46.6512392818024));
#20122=CARTESIAN_POINT('',(3.09917575053259,6.01559628526639,-3.69717978381041));
#20123=CARTESIAN_POINT('',(-6.76766674060731,-0.00120259113188305,45.6960259323079));
#20124=CARTESIAN_POINT('Ctrl Pts',(-6.76699874733023,-0.0041174787364938,
45.69717978381));
#20125=CARTESIAN_POINT('Ctrl Pts',(-6.76687707323121,-0.204086568634054,
45.7065548943844));
#20126=CARTESIAN_POINT('Ctrl Pts',(-6.7578875822965,-0.403727183863877,
45.7159300049587));
#20127=CARTESIAN_POINT('Ctrl Pts',(-6.74014155289775,-0.602312914439911,
45.7253051155331));
#20128=CARTESIAN_POINT('Ctrl Pts',(-6.72232161735131,-0.801725686716585,
45.734719270239));
#20129=CARTESIAN_POINT('Ctrl Pts',(-6.69567215036646,-1.00007463449364,
45.744133424945));
#20130=CARTESIAN_POINT('Ctrl Pts',(-6.66035568938451,-1.19664158831433,
45.7535475796509));
#20131=CARTESIAN_POINT('Ctrl Pts',(-6.62485099266477,-1.39425623843718,
45.7630119115351));
#20132=CARTESIAN_POINT('Ctrl Pts',(-6.58058674220859,-1.59006971430474,
45.7724762434192));
#20133=CARTESIAN_POINT('Ctrl Pts',(-6.52777710226088,-1.78337183537215,
45.7819405753034));
#20134=CARTESIAN_POINT('Ctrl Pts',(-6.49176167599389,-1.91520114334412,
45.788395115563));
#20135=CARTESIAN_POINT('Ctrl Pts',(-6.45177276579902,-2.04586281575445,
45.7948496558226));
#20136=CARTESIAN_POINT('Ctrl Pts',(-6.40789099875665,-2.1751372251087,45.8013041960823));
#20137=CARTESIAN_POINT('Ctrl Pts',(-6.34911231426086,-2.3482975199864,45.8099499141346));
#20138=CARTESIAN_POINT('Ctrl Pts',(-6.28325801214895,-2.51922872732067,
45.818595632187));
#20139=CARTESIAN_POINT('Ctrl Pts',(-6.21051183233006,-2.6873466059458,45.8272413502393));
#20140=CARTESIAN_POINT('Ctrl Pts',(-6.13785904378099,-2.85524865547579,
45.8358759689516));
#20141=CARTESIAN_POINT('Ctrl Pts',(-6.05833214096519,-3.02034429973347,
45.8445105876639));
#20142=CARTESIAN_POINT('Ctrl Pts',(-5.97216393053393,-3.18206646486675,
45.8531452063762));
#20143=CARTESIAN_POINT('Ctrl Pts',(-5.88295259364632,-3.34950002863337,
45.8620847662787));
#20144=CARTESIAN_POINT('Ctrl Pts',(-5.78662237322204,-3.51331717483302,
45.8710243261811));
#20145=CARTESIAN_POINT('Ctrl Pts',(-5.6834863835324,-3.67291049825636,45.8799638860836));
#20146=CARTESIAN_POINT('Ctrl Pts',(-5.58414500021901,-3.82663202227688,
45.888574539354));
#20147=CARTESIAN_POINT('Ctrl Pts',(-5.47848986391709,-3.97643467025301,
45.8971851926245));
#20148=CARTESIAN_POINT('Ctrl Pts',(-5.36684796464517,-4.12179959779512,
45.905795845895));
#20149=CARTESIAN_POINT('Ctrl Pts',(-5.2553117419003,-4.2670269277077,45.914398348606));
#20150=CARTESIAN_POINT('Ctrl Pts',(-5.13780023956334,-4.40782467096363,
45.9230008513171));
#20151=CARTESIAN_POINT('Ctrl Pts',(-5.01468361606663,-4.54370303065165,
45.9316033540281));
#20152=CARTESIAN_POINT('Ctrl Pts',(-4.8917055578514,-4.67942846198098,45.9401961747955));
#20153=CARTESIAN_POINT('Ctrl Pts',(-4.76313516799962,-4.81024532969496,
45.9487889955629));
#20154=CARTESIAN_POINT('Ctrl Pts',(-4.62938286366172,-4.93569684053176,
45.9573818163304));
#20155=CARTESIAN_POINT('Ctrl Pts',(-4.61361954705468,-4.95048187092014,
45.9583945192888));
#20156=CARTESIAN_POINT('Ctrl Pts',(-4.59778430079689,-4.96519241644914,
45.9594072222473));
#20157=CARTESIAN_POINT('Ctrl Pts',(-4.581877832874,-4.9798277605373,45.9604199252057));
#20158=CARTESIAN_POINT('Ctrl Pts',(-4.44687260680354,-5.10404439661381,
45.9690151829658));
#20159=CARTESIAN_POINT('Ctrl Pts',(-4.30689265901136,-5.22269458332118,
45.9776104407259));
#20160=CARTESIAN_POINT('Ctrl Pts',(-4.1624241898148,-5.33540194025198,45.986205698486));
#20161=CARTESIAN_POINT('Ctrl Pts',(-4.01782043202398,-5.44821484284245,
45.9948090053404));
#20162=CARTESIAN_POINT('Ctrl Pts',(-3.86872000361035,-5.55507361946534,
46.0034123121948));
#20163=CARTESIAN_POINT('Ctrl Pts',(-3.7156388435457,-5.65564470103404,46.0120156190493));
#20164=CARTESIAN_POINT('Ctrl Pts',(-3.5562108855009,-5.76038549451955,46.0209756219892));
#20165=CARTESIAN_POINT('Ctrl Pts',(-3.392465403019,-5.85830590497551,46.0299356249292));
#20166=CARTESIAN_POINT('Ctrl Pts',(-3.22501316908197,-5.94908220310057,
46.0388956278692));
#20167=CARTESIAN_POINT('Ctrl Pts',(-3.06378731054833,-6.03648316668055,
46.0475224710739));
#20168=CARTESIAN_POINT('Ctrl Pts',(-2.89912567226049,-6.11726162817497,
46.0561493142787));
#20169=CARTESIAN_POINT('Ctrl Pts',(-2.73159394639005,-6.1911778775969,46.0647761574835));
#20170=CARTESIAN_POINT('Ctrl Pts',(-2.56390210253855,-6.26516477226864,
46.0734112457696));
#20171=CARTESIAN_POINT('Ctrl Pts',(-2.39333497820425,-6.33227624899114,
46.0820463340558));
#20172=CARTESIAN_POINT('Ctrl Pts',(-2.22047563376888,-6.39232171905003,
46.0906814223419));
#20173=CARTESIAN_POINT('Ctrl Pts',(-2.04735955851763,-6.45245636868187,
46.0993293354671));
#20174=CARTESIAN_POINT('Ctrl Pts',(-1.87194475060178,-6.505503947692,46.1079772485922));
#20175=CARTESIAN_POINT('Ctrl Pts',(-1.69482816952968,-6.55132402463568,
46.1166251617174));
#20176=CARTESIAN_POINT('Ctrl Pts',(-1.67495838541209,-6.5564643397412,46.1175953259213));
#20177=CARTESIAN_POINT('Ctrl Pts',(-1.65506719264996,-6.56151374690653,
46.1185654901251));
#20178=CARTESIAN_POINT('Ctrl Pts',(-1.63515544032632,-6.5664720882656,46.119535654329));
#20179=CARTESIAN_POINT('Ctrl Pts',(-1.46635125143795,-6.60850700200626,
46.1277603338477));
#20180=CARTESIAN_POINT('Ctrl Pts',(-1.29570268034101,-6.64408396036139,
46.1359850133665));
#20181=CARTESIAN_POINT('Ctrl Pts',(-1.12374468653719,-6.67304180111884,
46.1442096928853));
#20182=CARTESIAN_POINT('Ctrl Pts',(-0.951967440038932,-6.70196920390959,
46.1524257273355));
#20183=CARTESIAN_POINT('Ctrl Pts',(-0.778883862167657,-6.72429128480226,
46.1606417617856));
#20184=CARTESIAN_POINT('Ctrl Pts',(-0.605042517849,-6.73989707277455,46.1688577962357));
#20185=CARTESIAN_POINT('Ctrl Pts',(-0.431349079722954,-6.75548958316498,
46.1770668403903));
#20186=CARTESIAN_POINT('Ctrl Pts',(-0.256899514153053,-6.7643771494694,
46.1852758845449));
#20187=CARTESIAN_POINT('Ctrl Pts',(-0.0822510853937956,-6.76650011150163,
46.1934849286995));
#20188=CARTESIAN_POINT('Ctrl Pts',(0.0922837230030589,-6.76862169240654,
46.2016886323276));
#20189=CARTESIAN_POINT('Ctrl Pts',(0.267016779777068,-6.76398743074585,
46.2098923359556));
#20190=CARTESIAN_POINT('Ctrl Pts',(0.441387114435408,-6.75258960808447,
46.2180960395836));
#20191=CARTESIAN_POINT('Ctrl Pts',(0.61567891936995,-6.74119691856611,46.2262960485776));
#20192=CARTESIAN_POINT('Ctrl Pts',(0.789607970726171,-6.72304675994468,
46.2344960575716));
#20193=CARTESIAN_POINT('Ctrl Pts',(0.962614622985368,-6.69818349163523,
46.2426960665655));
#20194=CARTESIAN_POINT('Ctrl Pts',(1.1356074412675,-6.67332221144519,46.2508954198695));
#20195=CARTESIAN_POINT('Ctrl Pts',(1.30767765162365,-6.64174893307519,46.2590947731734));
#20196=CARTESIAN_POINT('Ctrl Pts',(1.4782716717604,-6.6035597873019,46.2672941264774));
#20197=CARTESIAN_POINT('Ctrl Pts',(1.64886457967465,-6.56537089051054,46.2754934263239));
#20198=CARTESIAN_POINT('Ctrl Pts',(1.81798096644585,-6.52056628949023,46.2836927261705));
#20199=CARTESIAN_POINT('Ctrl Pts',(1.98507849305553,-6.46929303528665,46.2918920260171));
#20200=CARTESIAN_POINT('Ctrl Pts',(2.15220524336969,-6.41801081389811,46.3000927598401));
#20201=CARTESIAN_POINT('Ctrl Pts',(2.31731208732258,-6.36025779056477,46.3082934936631));
#20202=CARTESIAN_POINT('Ctrl Pts',(2.47987281956919,-6.296230602413,46.3164942274862));
#20203=CARTESIAN_POINT('Ctrl Pts',(2.64249147251195,-6.23218060125307,46.3246978832461));
#20204=CARTESIAN_POINT('Ctrl Pts',(2.80256187322549,-6.16185211335252,46.3329015390061));
#20205=CARTESIAN_POINT('Ctrl Pts',(2.95957868273731,-6.08548954651036,46.3411051947661));
#20206=CARTESIAN_POINT('Ctrl Pts',(3.11677536509815,-6.00903950143897,46.3493182483411));
#20207=CARTESIAN_POINT('Ctrl Pts',(3.27091114488567,-5.92654172444302,46.3575313019161));
#20208=CARTESIAN_POINT('Ctrl Pts',(3.42150521013566,-5.83828665766033,46.3657443554912));
#20209=CARTESIAN_POINT('Ctrl Pts',(3.57218838527274,-5.74997936837454,46.3739622689142));
#20210=CARTESIAN_POINT('Ctrl Pts',(3.71932536677659,-5.6559081912402,46.3821801823373));
#20211=CARTESIAN_POINT('Ctrl Pts',(3.86246525736947,-5.5564063148418,46.3903980957604));
#20212=CARTESIAN_POINT('Ctrl Pts',(4.00582839790815,-5.4567492490799,46.3986288263564));
#20213=CARTESIAN_POINT('Ctrl Pts',(4.14518170305987,-5.35164477300992,46.4068595569524));
#20214=CARTESIAN_POINT('Ctrl Pts',(4.28010718289921,-5.24146654123582,46.4150902875484));
#20215=CARTESIAN_POINT('Ctrl Pts',(4.40402009935294,-5.14028101241576,46.4226492292242));
#20216=CARTESIAN_POINT('Ctrl Pts',(4.52419874326469,-5.03481675630696,46.4302081709001));
#20217=CARTESIAN_POINT('Ctrl Pts',(4.6403480297744,-4.92538923970166,46.437767112576));
#20218=CARTESIAN_POINT('Ctrl Pts',(4.76563921444728,-4.80734888316323,46.4459210047427));
#20219=CARTESIAN_POINT('Ctrl Pts',(4.88662865956076,-4.68433134391698,46.4540748969094));
#20220=CARTESIAN_POINT('Ctrl Pts',(5.00289112422744,-4.55668403547211,46.4622287890761));
#20221=CARTESIAN_POINT('Ctrl Pts',(5.11901171620532,-4.42919249240618,46.4703727312163));
#20222=CARTESIAN_POINT('Ctrl Pts',(5.23041656606654,-4.29708269318446,46.4785166733565));
#20223=CARTESIAN_POINT('Ctrl Pts',(5.33671427509191,-4.16074148993064,46.4866606154968));
#20224=CARTESIAN_POINT('Ctrl Pts',(5.44290464476189,-4.02453796393255,46.4947963338897));
#20225=CARTESIAN_POINT('Ctrl Pts',(5.54399791740909,-3.88411182654212,46.5029320522826));
#20226=CARTESIAN_POINT('Ctrl Pts',(5.63964029380605,-3.7398858747934,46.5110677706755));
#20227=CARTESIAN_POINT('Ctrl Pts',(5.7352062089921,-3.59577522435077,46.5191969849757));
#20228=CARTESIAN_POINT('Ctrl Pts',(5.82532970345467,-3.447871111354,46.5273261992759));
#20229=CARTESIAN_POINT('Ctrl Pts',(5.90969796537712,-3.29662842280072,46.5354554135761));
#20230=CARTESIAN_POINT('Ctrl Pts',(5.9940165186433,-3.14547484442522,46.5435798382515));
#20231=CARTESIAN_POINT('Ctrl Pts',(6.07258641453862,-2.99098692630713,46.551704262927));
#20232=CARTESIAN_POINT('Ctrl Pts',(6.14513881239261,-2.83364746862166,46.5598286876024));
#20233=CARTESIAN_POINT('Ctrl Pts',(6.21813164974716,-2.67535285970467,46.5680024327366));
#20234=CARTESIAN_POINT('Ctrl Pts',(6.28503348242055,-2.51417228940198,46.5761761778708));
#20235=CARTESIAN_POINT('Ctrl Pts',(6.34561781566061,-2.35062194696865,46.5843499230049));
#20236=CARTESIAN_POINT('Ctrl Pts',(6.40581418455886,-2.18811893306995,46.5924713258671));
#20237=CARTESIAN_POINT('Ctrl Pts',(6.45977362134892,-2.02327676416144,46.6005927287292));
#20238=CARTESIAN_POINT('Ctrl Pts',(6.5073226460148,-1.85662085000221,46.6087141315914));
#20239=CARTESIAN_POINT('Ctrl Pts',(6.55487534692094,-1.68995205088511,46.6168361623577));
#20240=CARTESIAN_POINT('Ctrl Pts',(6.59601654801478,-1.52146957912764,46.6249581931239));
#20241=CARTESIAN_POINT('Ctrl Pts',(6.63062301652858,-1.35171277003713,46.6330802238902));
#20242=CARTESIAN_POINT('Ctrl Pts',(6.66523875050299,-1.18191051062781,46.6412044292313));
#20243=CARTESIAN_POINT('Ctrl Pts',(6.69331619506547,-1.01083359297957,46.6493286345724));
#20244=CARTESIAN_POINT('Ctrl Pts',(6.7147834865773,-0.839030230914723,46.6574528399135));
#20245=CARTESIAN_POINT('Ctrl Pts',(6.73648314666556,-0.665367216333993,
46.665664984156));
#20246=CARTESIAN_POINT('Ctrl Pts',(6.75142866861152,-0.490962319540475,
46.6738771283984));
#20247=CARTESIAN_POINT('Ctrl Pts',(6.75959981342889,-0.316384832588614,
46.6820892726408));
#20248=CARTESIAN_POINT('Ctrl Pts',(6.76769636469985,-0.143401045683258,
46.6902264490573));
#20249=CARTESIAN_POINT('Ctrl Pts',(6.76914176934004,0.0297518272489233,
46.6983636254738));
#20250=CARTESIAN_POINT('Ctrl Pts',(6.76396877858226,0.20252249841538,46.7065008018902));
#20251=CARTESIAN_POINT('Ctrl Pts',(6.75872429965996,0.377680774497899,46.7147504300456));
#20252=CARTESIAN_POINT('Ctrl Pts',(6.7466771868812,0.552445816264765,46.7230000582011));
#20253=CARTESIAN_POINT('Ctrl Pts',(6.7279155491853,0.7262515838404,46.7312496863565));
#20254=CARTESIAN_POINT('Ctrl Pts',(6.7091539114894,0.900057351416098,46.7394993145119));
#20255=CARTESIAN_POINT('Ctrl Pts',(6.68367786756759,1.07290347336076,46.7477489426673));
#20256=CARTESIAN_POINT('Ctrl Pts',(6.6516284246408,1.24423804013162,46.7559985708227));
#20257=CARTESIAN_POINT('Ctrl Pts',(6.61967322770685,1.41506877298592,46.764223939761));
#20258=CARTESIAN_POINT('Ctrl Pts',(6.58108788452275,1.58490752284196,46.7724493086992));
#20259=CARTESIAN_POINT('Ctrl Pts',(6.535944853491,1.75320103585543,46.7806746776375));
#20260=CARTESIAN_POINT('Ctrl Pts',(6.4908532574364,1.92130279893985,46.7888906747712));
#20261=CARTESIAN_POINT('Ctrl Pts',(6.43921894433532,2.08786248769128,46.7971066719049));
#20262=CARTESIAN_POINT('Ctrl Pts',(6.38116573048613,2.25233499286172,46.8053226690386));
#20263=CARTESIAN_POINT('Ctrl Pts',(6.32316699653763,2.41665314920023,46.8135309558893));
#20264=CARTESIAN_POINT('Ctrl Pts',(6.25876147769551,2.5788876867241,46.82173924274));
#20265=CARTESIAN_POINT('Ctrl Pts',(6.18812335874269,2.73850658151175,46.8299475295907));
#20266=CARTESIAN_POINT('Ctrl Pts',(6.1175373414047,2.8980077438017,46.8381497621324));
#20267=CARTESIAN_POINT('Ctrl Pts',(6.04072802571354,3.05489677954035,46.8463519946741));
#20268=CARTESIAN_POINT('Ctrl Pts',(5.95791849285489,3.20865956943048,46.8545542272158));
#20269=CARTESIAN_POINT('Ctrl Pts',(5.875152242314,3.36234199164185,46.862752172671));
#20270=CARTESIAN_POINT('Ctrl Pts',(5.78639219198939,3.51290110800492,46.8709501181261));
#20271=CARTESIAN_POINT('Ctrl Pts',(5.69190839107925,3.6598453338306,46.8791480635812));
#20272=CARTESIAN_POINT('Ctrl Pts',(5.59745048915356,3.80674928072823,46.887343761895));
#20273=CARTESIAN_POINT('Ctrl Pts',(5.49727215463076,3.95004000869569,46.8955394602087));
#20274=CARTESIAN_POINT('Ctrl Pts',(5.39168806620751,4.08925284088861,46.9037351585224));
#20275=CARTESIAN_POINT('Ctrl Pts',(5.28611371010395,4.2284528409985,46.9119301013894));
#20276=CARTESIAN_POINT('Ctrl Pts',(5.17513480943015,4.36357540829451,46.9201250442564));
#20277=CARTESIAN_POINT('Ctrl Pts',(5.05910785515908,4.49418699097709,46.9283199871233));
#20278=CARTESIAN_POINT('Ctrl Pts',(4.94307048684747,4.62481029674872,46.9365156655303));
#20279=CARTESIAN_POINT('Ctrl Pts',(4.82198440133823,4.75092154380613,46.9447113439373));
#20280=CARTESIAN_POINT('Ctrl Pts',(4.69624467744004,4.87212222030771,46.9529070223443));
#20281=CARTESIAN_POINT('Ctrl Pts',(4.57041656617863,4.9934080934988,46.9611084618138));
#20282=CARTESIAN_POINT('Ctrl Pts',(4.43992853930252,5.10977625015996,46.9693099012832));
#20283=CARTESIAN_POINT('Ctrl Pts',(4.30521122796165,5.2208663344921,46.9775113407527));
#20284=CARTESIAN_POINT('Ctrl Pts',(4.17044471281827,5.33199699307943,46.9857157756947));
#20285=CARTESIAN_POINT('Ctrl Pts',(4.03144611770919,5.43784551698511,46.9939202106367));
#20286=CARTESIAN_POINT('Ctrl Pts',(3.88867705369091,5.53809351420665,47.0021246455787));
#20287=CARTESIAN_POINT('Ctrl Pts',(3.74574858479657,5.63845344057532,47.0103382409571));
#20288=CARTESIAN_POINT('Ctrl Pts',(3.59904153553808,5.73320014918724,47.0185518363356));
#20289=CARTESIAN_POINT('Ctrl Pts',(3.44904507755022,5.82205951988011,47.026765431714));
#20290=CARTESIAN_POINT('Ctrl Pts',(3.33427144539633,5.89005254359641,47.0330502746181));
#20291=CARTESIAN_POINT('Ctrl Pts',(3.2175724536714,5.95459947399275,47.0393351175222));
#20292=CARTESIAN_POINT('Ctrl Pts',(3.09917575053261,6.01559628526638,47.0456199604263));
#20293=CARTESIAN_POINT('Ctrl Pts',(3.09917575053261,6.01559628526638,45.0457515827422));
#20294=CARTESIAN_POINT('Ctrl Pts',(2.93382384459261,6.10078395293761,45.0545010306546));
#20295=CARTESIAN_POINT('Ctrl Pts',(2.76495772122974,6.17915010267054,45.063250478567));
#20296=CARTESIAN_POINT('Ctrl Pts',(2.59315093316695,6.25042856433184,45.0719999264794));
#20297=CARTESIAN_POINT('Ctrl Pts',(2.42134553245605,6.32170645041456,45.0807493037394));
#20298=CARTESIAN_POINT('Ctrl Pts',(2.24659977927582,6.3858966531346,45.0894986809994));
#20299=CARTESIAN_POINT('Ctrl Pts',(2.06950718689915,6.44278115439076,45.0982480582594));
#20300=CARTESIAN_POINT('Ctrl Pts',(1.89241596572862,6.49966521519724,45.1069973677741));
#20301=CARTESIAN_POINT('Ctrl Pts',(1.71297821457202,6.54924360009545,45.1157466772887));
#20302=CARTESIAN_POINT('Ctrl Pts',(1.53180337335854,6.59134792173554,45.1244959868034));
#20303=CARTESIAN_POINT('Ctrl Pts',(1.3506298747779,6.63345193135303,45.1332452314795));
#20304=CARTESIAN_POINT('Ctrl Pts',(1.16771959102959,6.66808192368237,45.1419944761556));
#20305=CARTESIAN_POINT('Ctrl Pts',(0.9836937469069,6.69512028363167,45.1507437208318));
#20306=CARTESIAN_POINT('Ctrl Pts',(0.799669205419907,6.72215845218867,45.1594929035759));
#20307=CARTESIAN_POINT('Ctrl Pts',(0.614529402873492,6.74160505424579,45.1682420863201));
#20308=CARTESIAN_POINT('Ctrl Pts',(0.428903127363245,6.75339404354122,45.1769912690643));
#20309=CARTESIAN_POINT('Ctrl Pts',(0.243278104163816,6.76518295330331,45.1857403927829));
#20310=CARTESIAN_POINT('Ctrl Pts',(0.0571669005389931,6.76931433552276,
45.1944895165015));
#20311=CARTESIAN_POINT('Ctrl Pts',(-0.128798404777697,6.76577415902473,
45.2032386402201));
#20312=CARTESIAN_POINT('Ctrl Pts',(-0.314762517259329,6.7622340052344,45.2119877078193));
#20313=CARTESIAN_POINT('Ctrl Pts',(-0.500580446819786,6.75102239665087,
45.2207367754185));
#20314=CARTESIAN_POINT('Ctrl Pts',(-0.685621118842932,6.73217741012494,
45.2294858430178));
#20315=CARTESIAN_POINT('Ctrl Pts',(-0.870660665414716,6.71333253821769,
45.2382348574035));
#20316=CARTESIAN_POINT('Ctrl Pts',(-1.054922678855,6.6868544103061,45.2469838717893));
#20317=CARTESIAN_POINT('Ctrl Pts',(-1.23778137635256,6.65283295028177,45.2557328861751));
#20318=CARTESIAN_POINT('Ctrl Pts',(-1.4299992297885,6.61707018861865,45.2649296965425));
#20319=CARTESIAN_POINT('Ctrl Pts',(-1.62066601233698,6.57297172934412,45.2741265069099));
#20320=CARTESIAN_POINT('Ctrl Pts',(-1.80906628500387,6.52070304311294,45.2833233172773));
#20321=CARTESIAN_POINT('Ctrl Pts',(-1.98831342545531,6.4709737491503,45.292073315015));
#20322=CARTESIAN_POINT('Ctrl Pts',(-2.16550875896707,6.41384933989527,45.3008233127528));
#20323=CARTESIAN_POINT('Ctrl Pts',(-2.34005036714018,6.34952386240473,45.3095733104906));
#20324=CARTESIAN_POINT('Ctrl Pts',(-2.51458843547096,6.28519968948593,45.3183231307714));
#20325=CARTESIAN_POINT('Ctrl Pts',(-2.68647261718063,6.21367483971096,45.3270729510523));
#20326=CARTESIAN_POINT('Ctrl Pts',(-2.85511905908739,6.1351922674384,45.3358227713331));
#20327=CARTESIAN_POINT('Ctrl Pts',(-3.02376230488893,6.05671118252933,45.3445724257917));
#20328=CARTESIAN_POINT('Ctrl Pts',(-3.18916767379913,5.97127275992628,45.3533220802502));
#20329=CARTESIAN_POINT('Ctrl Pts',(-3.35077334102797,5.87916720437991,45.3620717347087));
#20330=CARTESIAN_POINT('Ctrl Pts',(-3.51237616037376,5.78706327195638,45.3708212349772));
#20331=CARTESIAN_POINT('Ctrl Pts',(-3.67017916302306,5.68829258362294,45.3795707352456));
#20332=CARTESIAN_POINT('Ctrl Pts',(-3.82364636566466,5.58319061741039,45.3883202355141));
#20333=CARTESIAN_POINT('Ctrl Pts',(-3.97711106778793,5.47809036367705,45.3970695932225));
#20334=CARTESIAN_POINT('Ctrl Pts',(-4.12623987481914,5.36665920043235,45.4058189509309));
#20335=CARTESIAN_POINT('Ctrl Pts',(-4.27052628213908,5.24927559512352,45.4145683086394));
#20336=CARTESIAN_POINT('Ctrl Pts',(-4.41481053024965,5.13189374643048,45.4233175354159));
#20337=CARTESIAN_POINT('Ctrl Pts',(-4.55425230136524,5.00855981477359,45.4320667621924));
#20338=CARTESIAN_POINT('Ctrl Pts',(-4.68837800630548,4.87969268192076,45.4408159889689));
#20339=CARTESIAN_POINT('Ctrl Pts',(-4.82250188228864,4.75082730631839,45.4495650964398));
#20340=CARTESIAN_POINT('Ctrl Pts',(-4.95130963052908,4.61642907903586,45.4583142039106));
#20341=CARTESIAN_POINT('Ctrl Pts',(-5.07436379033284,4.47695444731783,45.4670633113814));
#20342=CARTESIAN_POINT('Ctrl Pts',(-5.19741643562712,4.33748153220697,45.4758123111711));
#20343=CARTESIAN_POINT('Ctrl Pts',(-5.31471544462671,4.19293255254718,45.4845613109609));
#20344=CARTESIAN_POINT('Ctrl Pts',(-5.42586245275517,4.04379841779751,45.4933103107506));
#20345=CARTESIAN_POINT('Ctrl Pts',(-5.53702160019041,3.89464799484502,45.5020602660928));
#20346=CARTESIAN_POINT('Ctrl Pts',(-5.64202723081139,3.7409116444402,45.5108102214349));
#20347=CARTESIAN_POINT('Ctrl Pts',(-5.74052265232854,3.58311159163414,45.5195601767771));
#20348=CARTESIAN_POINT('Ctrl Pts',(-5.83901427066817,3.42531763191956,45.5283097942595));
#20349=CARTESIAN_POINT('Ctrl Pts',(-5.93099603115649,3.26346052695777,45.537059411742));
#20350=CARTESIAN_POINT('Ctrl Pts',(-6.01615550622674,3.09809004467232,45.5458090292244));
#20351=CARTESIAN_POINT('Ctrl Pts',(-6.10131214578726,2.93272506863981,45.5545583553755));
#20352=CARTESIAN_POINT('Ctrl Pts',(-6.1796468232868,2.76384720417045,45.5633076815266));
#20353=CARTESIAN_POINT('Ctrl Pts',(-6.25089348288503,2.59203002791741,45.5720570076777));
#20354=CARTESIAN_POINT('Ctrl Pts',(-6.32213814889273,2.42021765937177,45.5808060890093));
#20355=CARTESIAN_POINT('Ctrl Pts',(-6.38629508412533,2.24546640832067,45.5895551703409));
#20356=CARTESIAN_POINT('Ctrl Pts',(-6.44314639819764,2.06836976660191,45.5983042516724));
#20357=CARTESIAN_POINT('Ctrl Pts',(-6.50000285283656,1.89125711158428,45.6070541241068));
#20358=CARTESIAN_POINT('Ctrl Pts',(-6.54955227673208,1.71179891440411,45.6158039965412));
#20359=CARTESIAN_POINT('Ctrl Pts',(-6.59162635926348,1.53060476278591,45.6245538689756));
#20360=CARTESIAN_POINT('Ctrl Pts',(-6.63369752055166,1.34942319164848,45.6333031338981));
#20361=CARTESIAN_POINT('Ctrl Pts',(-6.66829431424229,1.16650618642847,45.6420523988206));
#20362=CARTESIAN_POINT('Ctrl Pts',(-6.69529923745398,0.982474997619904,
45.6508016637431));
#20363=CARTESIAN_POINT('Ctrl Pts',(-6.72230554731428,0.798434359179042,
45.6595513779228));
#20364=CARTESIAN_POINT('Ctrl Pts',(-6.74171916496692,0.613279706241595,
45.6683010921025));
#20365=CARTESIAN_POINT('Ctrl Pts',(-6.75347414817267,0.427639953656586,
45.6770508062822));
#20366=CARTESIAN_POINT('Ctrl Pts',(-6.76248837758742,0.285283364199395,
45.6837604654581));
#20367=CARTESIAN_POINT('Ctrl Pts',(-6.76699999999997,0.142641701105548,
45.6904701246341));
#20368=CARTESIAN_POINT('Ctrl Pts',(-6.767,1.61040289520569E-12,45.69717978381));
#20369=CARTESIAN_POINT('',(-6.76699973265636,-0.0019021642129279,45.3028202162182));
#20370=CARTESIAN_POINT('Ctrl Pts',(3.09917575053253,6.01559628526642,44.6513725725535));
#20371=CARTESIAN_POINT('Ctrl Pts',(2.9437420728611,6.0956741797613,44.6595737570002));
#20372=CARTESIAN_POINT('Ctrl Pts',(2.7852141545089,6.16971810297613,44.6677749414468));
#20373=CARTESIAN_POINT('Ctrl Pts',(2.62410422784775,6.23749677365781,44.6759761258935));
#20374=CARTESIAN_POINT('Ctrl Pts',(2.46295268942282,6.30529295033736,44.6841794285569));
#20375=CARTESIAN_POINT('Ctrl Pts',(2.2992181444318,6.36682051187649,44.6923827312203));
#20376=CARTESIAN_POINT('Ctrl Pts',(2.13343179158499,6.42189674400441,44.7005860338837));
#20377=CARTESIAN_POINT('Ctrl Pts',(1.96757257393781,6.47699718270055,44.7087929419827));
#20378=CARTESIAN_POINT('Ctrl Pts',(1.79966009172503,6.5256405308075,44.7169998500816));
#20379=CARTESIAN_POINT('Ctrl Pts',(1.63023969950547,6.56769423178,44.7252067581806));
#20380=CARTESIAN_POINT('Ctrl Pts',(1.46062126562505,6.60979709085371,44.7334232596331));
#20381=CARTESIAN_POINT('Ctrl Pts',(1.28949174912264,6.64529483190286,44.7416397610855));
#20382=CARTESIAN_POINT('Ctrl Pts',(1.11740662978061,6.67410603929263,44.749856262538));
#20383=CARTESIAN_POINT('Ctrl Pts',(0.94520687225507,6.70293643988453,44.7580782375887));
#20384=CARTESIAN_POINT('Ctrl Pts',(0.772050597385722,6.72507138328482,44.7663002126393));
#20385=CARTESIAN_POINT('Ctrl Pts',(0.598497247238427,6.74048144015307,44.77452218769));
#20386=CARTESIAN_POINT('Ctrl Pts',(0.424697225229204,6.75591339937825,44.7827558486568));
#20387=CARTESIAN_POINT('Ctrl Pts',(0.250499357361747,6.76460136413436,44.7909895096236));
#20388=CARTESIAN_POINT('Ctrl Pts',(0.0764629357328109,6.76656799415029,
44.7992231705904));
#20389=CARTESIAN_POINT('Ctrl Pts',(-0.00117737115148329,6.7674453378496,
44.8028963325542));
#20390=CARTESIAN_POINT('Ctrl Pts',(-0.0787856135802052,6.7669857002162,
44.806569494518));
#20391=CARTESIAN_POINT('Ctrl Pts',(-0.156312583787009,6.76519440786071,
44.8102426564818));
#20392=CARTESIAN_POINT('Ctrl Pts',(-0.328444383897077,6.76121723221653,
44.8183981148886));
#20393=CARTESIAN_POINT('Ctrl Pts',(-0.500705055019613,6.75065976822586,
44.8265535732954));
#20394=CARTESIAN_POINT('Ctrl Pts',(-0.672545883368081,6.73349619698153,
44.8347090317022));
#20395=CARTESIAN_POINT('Ctrl Pts',(-0.844177558840259,6.71635351605952,
44.842854563844));
#20396=CARTESIAN_POINT('Ctrl Pts',(-1.01539004901787,6.69262076879519,44.8510000959859));
#20397=CARTESIAN_POINT('Ctrl Pts',(-1.18563345689058,6.66232409192931,44.8591456281278));
#20398=CARTESIAN_POINT('Ctrl Pts',(-1.35570545493074,6.63205791931833,44.8672829589283));
#20399=CARTESIAN_POINT('Ctrl Pts',(-1.52480995599806,6.59524103781933,44.8754202897289));
#20400=CARTESIAN_POINT('Ctrl Pts',(-1.69240100768474,6.55195145198647,44.8835576205294));
#20401=CARTESIAN_POINT('Ctrl Pts',(-1.8598585398467,6.5086963548979,44.8916884683314));
#20402=CARTESIAN_POINT('Ctrl Pts',(-2.0258046712114,6.45897891227745,44.8998193161334));
#20403=CARTESIAN_POINT('Ctrl Pts',(-2.18970248843383,6.40292839348893,44.9079501639354));
#20404=CARTESIAN_POINT('Ctrl Pts',(-2.35350415809935,6.34691075567793,44.9160762419292));
#20405=CARTESIAN_POINT('Ctrl Pts',(-2.51525956162403,6.28456755838002,44.924202319923));
#20406=CARTESIAN_POINT('Ctrl Pts',(-2.67444583368734,6.216078223661,44.9323283979168));
#20407=CARTESIAN_POINT('Ctrl Pts',(-2.83419655119693,6.14734603827024,44.940483289499));
#20408=CARTESIAN_POINT('Ctrl Pts',(-2.99135952598779,6.07242414824676,44.9486381810812));
#20409=CARTESIAN_POINT('Ctrl Pts',(-3.14542489990301,5.99154330695107,44.9567930726634));
#20410=CARTESIAN_POINT('Ctrl Pts',(-3.29888947272746,5.91097787265721,44.9649161630197));
#20411=CARTESIAN_POINT('Ctrl Pts',(-3.44928024226919,5.82450006568852,44.973039253376));
#20412=CARTESIAN_POINT('Ctrl Pts',(-3.59611672016378,5.73238462901422,44.9811623437323));
#20413=CARTESIAN_POINT('Ctrl Pts',(-3.74296472832917,5.64026195901517,44.9892860719508));
#20414=CARTESIAN_POINT('Ctrl Pts',(-3.88625757899098,5.5425009718914,44.9974098001692));
#20415=CARTESIAN_POINT('Ctrl Pts',(-4.02554283308931,5.43942036424501,45.0055335283877));
#20416=CARTESIAN_POINT('Ctrl Pts',(-4.16486552335506,5.3363120512761,45.013659440048));
#20417=CARTESIAN_POINT('Ctrl Pts',(-4.3001781783461,5.22788148837119,45.0217853517083));
#20418=CARTESIAN_POINT('Ctrl Pts',(-4.4310606155373,5.11448832449877,45.0299112633685));
#20419=CARTESIAN_POINT('Ctrl Pts',(-4.56278005952017,5.00036999955564,45.0380891410786));
#20420=CARTESIAN_POINT('Ctrl Pts',(-4.69001214174115,4.88122562657827,45.0462670187887));
#20421=CARTESIAN_POINT('Ctrl Pts',(-4.81236605622012,4.75745961001672,45.0544448964988));
#20422=CARTESIAN_POINT('Ctrl Pts',(-4.93413600200223,4.634284301809,45.0625837429722));
#20423=CARTESIAN_POINT('Ctrl Pts',(-5.0510740412375,4.50653168095525,45.0707225894456));
#20424=CARTESIAN_POINT('Ctrl Pts',(-5.16283553362158,4.37463349925161,45.0788614359191));
#20425=CARTESIAN_POINT('Ctrl Pts',(-5.27540098316419,4.24178650695932,45.0870588292475));
#20426=CARTESIAN_POINT('Ctrl Pts',(-5.38271489711704,4.10473438413423,45.0952562225759));
#20427=CARTESIAN_POINT('Ctrl Pts',(-5.48446984907871,3.96394746112339,45.1034536159043));
#20428=CARTESIAN_POINT('Ctrl Pts',(-5.58622480104038,3.82316053811254,45.1116510092327));
#20429=CARTESIAN_POINT('Ctrl Pts',(-5.68242063563078,3.67863915864375,45.1198484025611));
#20430=CARTESIAN_POINT('Ctrl Pts',(-5.77279741327199,3.53087793973684,45.1280457958895));
#20431=CARTESIAN_POINT('Ctrl Pts',(-5.86662260470627,3.37747874790526,45.1365559687278));
#20432=CARTESIAN_POINT('Ctrl Pts',(-5.95443936757663,3.22015832143925,45.1450661415661));
#20433=CARTESIAN_POINT('Ctrl Pts',(-6.03591757032215,3.05940976076699,45.1535763144045));
#20434=CARTESIAN_POINT('Ctrl Pts',(-6.11728481284174,2.89888011381656,45.1620748977542));
#20435=CARTESIAN_POINT('Ctrl Pts',(-6.19233055395715,2.73493192385575,45.170573481104));
#20436=CARTESIAN_POINT('Ctrl Pts',(-6.26076857721881,2.56808602319111,45.1790720644537));
#20437=CARTESIAN_POINT('Ctrl Pts',(-6.32912168482866,2.40144713944094,45.1875601030404));
#20438=CARTESIAN_POINT('Ctrl Pts',(-6.39088329399675,2.23191800921721,45.196048141627));
#20439=CARTESIAN_POINT('Ctrl Pts',(-6.44581345317645,2.06004318567584,45.2045361802136));
#20440=CARTESIAN_POINT('Ctrl Pts',(-6.50066071850216,1.8884277345219,45.2130114096942));
#20441=CARTESIAN_POINT('Ctrl Pts',(-6.5486969998166,1.71447395817075,45.2214866391749));
#20442=CARTESIAN_POINT('Ctrl Pts',(-6.58973080093811,1.53874525869867,45.2299618686555));
#20443=CARTESIAN_POINT('Ctrl Pts',(-6.6307281949429,1.36317247398701,45.2384295785142));
#20444=CARTESIAN_POINT('Ctrl Pts',(-6.66473541712651,1.18582821850764,45.246897288373));
#20445=CARTESIAN_POINT('Ctrl Pts',(-6.69161067495236,1.00729120658509,45.2553649982317));
#20446=CARTESIAN_POINT('Ctrl Pts',(-6.71845848019703,0.82893656693392,45.2638240584807));
#20447=CARTESIAN_POINT('Ctrl Pts',(-6.73818880400721,0.649391920275191,
45.2722831187297));
#20448=CARTESIAN_POINT('Ctrl Pts',(-6.7507108406708,0.469246359229067,45.2807421789787));
#20449=CARTESIAN_POINT('Ctrl Pts',(-6.76160495827098,0.312520502252987,
45.2881015247158));
#20450=CARTESIAN_POINT('Ctrl Pts',(-6.76704393253596,0.155340131828287,
45.2954608704528));
#20451=CARTESIAN_POINT('Ctrl Pts',(-6.76699973265654,-0.00190216360935057,
45.3028202161899));
#20452=CARTESIAN_POINT('Ctrl Pts',(-6.76699973265637,-0.00190216421283039,
45.3028202162181));
#20453=CARTESIAN_POINT('Ctrl Pts',(-6.7669471825227,-0.188850661127842,
45.3115698889445));
#20454=CARTESIAN_POINT('Ctrl Pts',(-6.75914331389005,-0.375595569033888,
45.3203195616709));
#20455=CARTESIAN_POINT('Ctrl Pts',(-6.7436639021329,-0.561503495153537,
45.3290692343973));
#20456=CARTESIAN_POINT('Ctrl Pts',(-6.72815474027868,-0.747768720306037,
45.3378357232415));
#20457=CARTESIAN_POINT('Ctrl Pts',(-6.7049405837135,-0.933193474538999,
45.3466022120858));
#20458=CARTESIAN_POINT('Ctrl Pts',(-6.67414848370708,-1.11715308594232,
45.3553687009301));
#20459=CARTESIAN_POINT('Ctrl Pts',(-6.64326641890751,-1.30165016924219,
45.3641608026866));
#20460=CARTESIAN_POINT('Ctrl Pts',(-6.60476215828831,-1.48467327101841,
45.3729529044431));
#20461=CARTESIAN_POINT('Ctrl Pts',(-6.55881366539612,-1.66560868832183,
45.3817450061997));
#20462=CARTESIAN_POINT('Ctrl Pts',(-6.51279361530138,-1.84682588270842,
45.3905508002052));
#20463=CARTESIAN_POINT('Ctrl Pts',(-6.45930625285953,-2.02594863342554,
45.3993565942107));
#20464=CARTESIAN_POINT('Ctrl Pts',(-6.3985786005201,-2.202380732972,45.4081623882163));
#20465=CARTESIAN_POINT('Ctrl Pts',(-6.33770714788192,-2.37923061564765,
45.4169890339386));
#20466=CARTESIAN_POINT('Ctrl Pts',(-6.26956121274525,-2.55337684513432,
45.4258156796609));
#20467=CARTESIAN_POINT('Ctrl Pts',(-6.19441589284408,-2.72424315113036,
45.4346423253833));
#20468=CARTESIAN_POINT('Ctrl Pts',(-6.16261354068299,-2.79655571088655,
45.4383778620213));
#20469=CARTESIAN_POINT('Ctrl Pts',(-6.12955809997296,-2.86828112775628,
45.4421133986592));
#20470=CARTESIAN_POINT('Ctrl Pts',(-6.09527282366468,-2.93937717979418,
45.4458489352972));
#20471=CARTESIAN_POINT('Ctrl Pts',(-6.01977160329613,-3.09594114165299,
45.454075136316));
#20472=CARTESIAN_POINT('Ctrl Pts',(-5.93812869545449,-3.24981306424306,
45.4623013373349));
#20473=CARTESIAN_POINT('Ctrl Pts',(-5.85055888297444,-3.40047787183639,
45.4705275383537));
#20474=CARTESIAN_POINT('Ctrl Pts',(-5.76308743672242,-3.55097343927262,
45.4787444989695));
#20475=CARTESIAN_POINT('Ctrl Pts',(-5.66970252156123,-3.69826875805281,
45.4869614595852));
#20476=CARTESIAN_POINT('Ctrl Pts',(-5.57066635348732,-3.84187003659993,
45.495178420201));
#20477=CARTESIAN_POINT('Ctrl Pts',(-5.47172155432969,-3.98533883129341,
45.5033878000026));
#20478=CARTESIAN_POINT('Ctrl Pts',(-5.36713608794945,-4.12512007963921,
45.5115971798042));
#20479=CARTESIAN_POINT('Ctrl Pts',(-5.25721736041371,-4.26074578276676,
45.5198065596057));
#20480=CARTESIAN_POINT('Ctrl Pts',(-5.14737798735698,-4.39627357257915,
45.5280100127461));
#20481=CARTESIAN_POINT('Ctrl Pts',(-5.03221324714273,-4.52765151525559,
45.5362134658865));
#20482=CARTESIAN_POINT('Ctrl Pts',(-4.91207305886323,-4.65444167053258,
45.5444169190269));
#20483=CARTESIAN_POINT('Ctrl Pts',(-4.79199550449857,-4.78116572499931,
45.5526160953771));
#20484=CARTESIAN_POINT('Ctrl Pts',(-4.66694791567108,-4.90330649724465,
45.5608152717272));
#20485=CARTESIAN_POINT('Ctrl Pts',(-4.53731963983386,-5.02046008708146,
45.5690144480774));
#20486=CARTESIAN_POINT('Ctrl Pts',(-4.40771575551302,-5.13759163270232,
45.5772120816287));
#20487=CARTESIAN_POINT('Ctrl Pts',(-4.27353316267407,-5.24973762029901,
45.5854097151801));
#20488=CARTESIAN_POINT('Ctrl Pts',(-4.13519734668707,-5.35653170474629,
45.5936073487315));
#20489=CARTESIAN_POINT('Ctrl Pts',(-3.99687149427392,-5.46331809739851,
45.601804391852));
#20490=CARTESIAN_POINT('Ctrl Pts',(-3.85439329783237,-5.56475313470061,
45.6100014349726));
#20491=CARTESIAN_POINT('Ctrl Pts',(-3.708220487231,-5.66051144492088,45.6181984780932));
#20492=CARTESIAN_POINT('Ctrl Pts',(-3.56203163799523,-5.75628026210563,
45.6263964206244));
#20493=CARTESIAN_POINT('Ctrl Pts',(-3.41214766704513,-5.84637091467463,
45.6345943631556));
#20494=CARTESIAN_POINT('Ctrl Pts',(-3.25905441604444,-5.93050194446147,
45.6427923056867));
#20495=CARTESIAN_POINT('Ctrl Pts',(-3.10591654252586,-6.01465749615478,
45.6509926376952));
#20496=CARTESIAN_POINT('Ctrl Pts',(-2.94956783998034,-6.09284979233589,
45.6591929697036));
#20497=CARTESIAN_POINT('Ctrl Pts',(-2.79051785633367,-6.16484380122343,
45.667393301712));
#20498=CARTESIAN_POINT('Ctrl Pts',(-2.63130209961605,-6.23691284732676,
45.6756021806828));
#20499=CARTESIAN_POINT('Ctrl Pts',(-2.46937976411834,-6.30277055134834,
45.6838110596535));
#20500=CARTESIAN_POINT('Ctrl Pts',(-2.3052803772165,-6.36223006361925,45.6920199386243));
#20501=CARTESIAN_POINT('Ctrl Pts',(-2.14109289795754,-6.42172149513548,
45.7002332243117));
#20502=CARTESIAN_POINT('Ctrl Pts',(-1.97472637884107,-6.47480777878317,
45.708446509999));
#20503=CARTESIAN_POINT('Ctrl Pts',(-1.80672444073288,-6.52135229804819,
45.7166597956864));
#20504=CARTESIAN_POINT('Ctrl Pts',(-1.63847673649504,-6.56796490620842,
45.7248850963985));
#20505=CARTESIAN_POINT('Ctrl Pts',(-1.46858918126387,-6.60801654307638,
45.7331103971106));
#20506=CARTESIAN_POINT('Ctrl Pts',(-1.29761575748285,-6.64142171119499,
45.7413356978227));
#20507=CARTESIAN_POINT('Ctrl Pts',(-1.14299091982237,-6.67163265616605,
45.7487744901168));
#20508=CARTESIAN_POINT('Ctrl Pts',(-0.987478236060209,-6.69640808578942,
45.7562132824109));
#20509=CARTESIAN_POINT('Ctrl Pts',(-0.831489413486529,-6.71572143222602,
45.7636520747049));
#20510=CARTESIAN_POINT('Ctrl Pts',(-0.660533215975414,-6.73688792488581,
45.7718046309182));
#20511=CARTESIAN_POINT('Ctrl Pts',(-0.488500868444045,-6.75155544123094,
45.7799571871314));
#20512=CARTESIAN_POINT('Ctrl Pts',(-0.315932268866136,-6.75962098060898,
45.7881097433447));
#20513=CARTESIAN_POINT('Ctrl Pts',(-0.14356359417106,-6.76767717586521,
45.796252854625));
#20514=CARTESIAN_POINT('Ctrl Pts',(0.0293397344602783,-6.76914660243042,
45.8043959659054));
#20515=CARTESIAN_POINT('Ctrl Pts',(0.202229370063513,-6.76397754888969,
45.8125390771857));
#20516=CARTESIAN_POINT('Ctrl Pts',(0.374955056748411,-6.75881339709297,
45.820674466463));
#20517=CARTESIAN_POINT('Ctrl Pts',(0.547666713371004,-6.74702330894105,
45.8288098557404));
#20518=CARTESIAN_POINT('Ctrl Pts',(0.719812633999018,-6.7286074912968,45.8369452450177));
#20519=CARTESIAN_POINT('Ctrl Pts',(0.891831482975453,-6.71020526751731,
45.8450746290563));
#20520=CARTESIAN_POINT('Ctrl Pts',(1.06328506552707,-6.68518709153682,45.8532040130949));
#20521=CARTESIAN_POINT('Ctrl Pts',(1.23362344560039,-6.6536052027803,45.8613333971335));
#20522=CARTESIAN_POINT('Ctrl Pts',(1.40387186748705,-6.62203999288054,45.8694584879256));
#20523=CARTESIAN_POINT('Ctrl Pts',(1.5730059011896,-6.58391804016423,45.8775835787178));
#20524=CARTESIAN_POINT('Ctrl Pts',(1.74048249575696,-6.53934321487744,45.8857086695099));
#20525=CARTESIAN_POINT('Ctrl Pts',(1.90859838479267,-6.49459823781926,45.893864775535));
#20526=CARTESIAN_POINT('Ctrl Pts',(2.07504378685537,-6.44335107430534,45.9020208815601));
#20527=CARTESIAN_POINT('Ctrl Pts',(2.23928099763713,-6.38575834287685,45.9101769875852));
#20528=CARTESIAN_POINT('Ctrl Pts',(2.40285718334811,-6.32839741177661,45.9183002667586));
#20529=CARTESIAN_POINT('Ctrl Pts',(2.56424257946716,-6.26474203966973,45.926423545932));
#20530=CARTESIAN_POINT('Ctrl Pts',(2.72292270399433,-6.19499644455687,45.9345468251054));
#20531=CARTESIAN_POINT('Ctrl Pts',(2.881623958121,-6.12524156222864,45.9426711859621));
#20532=CARTESIAN_POINT('Ctrl Pts',(3.03761888820817,-6.04939498882009,45.9507955468188));
#20533=CARTESIAN_POINT('Ctrl Pts',(3.19041463624472,-5.96770839173929,45.9589199076755));
#20534=CARTESIAN_POINT('Ctrl Pts',(3.3432598005035,-5.88599537610242,45.9670468960609));
#20535=CARTESIAN_POINT('Ctrl Pts',(3.49290339993014,-5.79843874809302,45.9751738844463));
#20536=CARTESIAN_POINT('Ctrl Pts',(3.6388787853827,-5.70533523864214,45.9833008728317));
#20537=CARTESIAN_POINT('Ctrl Pts',(3.78579788508253,-5.61162982560273,45.9914804012718));
#20538=CARTESIAN_POINT('Ctrl Pts',(3.9290008603406,-5.51230576465283,45.9996599297119));
#20539=CARTESIAN_POINT('Ctrl Pts',(4.06804386164321,-5.40770821510804,46.0078394581519));
#20540=CARTESIAN_POINT('Ctrl Pts',(4.20643206462738,-5.30360324914469,46.0159804665556));
#20541=CARTESIAN_POINT('Ctrl Pts',(4.34069914794465,-5.19427463737249,46.0241214749593));
#20542=CARTESIAN_POINT('Ctrl Pts',(4.47044314019526,-5.0801010944942,46.032262483363));
#20543=CARTESIAN_POINT('Ctrl Pts',(4.60110797843696,-4.96511721544986,46.0404612718212));
#20544=CARTESIAN_POINT('Ctrl Pts',(4.72718501160129,-4.845219639765,46.0486600602795));
#20545=CARTESIAN_POINT('Ctrl Pts',(4.84830387431723,-4.72083028102902,46.0568588487377));
#20546=CARTESIAN_POINT('Ctrl Pts',(4.96942273703317,-4.59644092229304,46.0650576371959));
#20547=CARTESIAN_POINT('Ctrl Pts',(5.08558322879314,-4.46756009973438,46.0732564256542));
#20548=CARTESIAN_POINT('Ctrl Pts',(5.19645862884004,-4.33464032172843,46.0814552141124));
#20549=CARTESIAN_POINT('Ctrl Pts',(5.30779736280562,-4.20116508920697,46.0896882642445));
#20550=CARTESIAN_POINT('Ctrl Pts',(5.41415293398444,-4.06320223827321,46.0979213143765));
#20551=CARTESIAN_POINT('Ctrl Pts',(5.51514317079271,-3.92115860501186,46.1061543645085));
#20552=CARTESIAN_POINT('Ctrl Pts',(5.61601314375281,-3.77928412388327,46.1143776103433));
#20553=CARTESIAN_POINT('Ctrl Pts',(5.71153029948196,-3.63333882611836,46.1226008561782));
#20554=CARTESIAN_POINT('Ctrl Pts',(5.80135125192717,-3.48376414984756,46.1308241020131));
#20555=CARTESIAN_POINT('Ctrl Pts',(5.89108321928234,-3.33433765633003,46.1390392011266));
#20556=CARTESIAN_POINT('Ctrl Pts',(5.97513003871564,-3.18128924995496,46.1472543002401));
#20557=CARTESIAN_POINT('Ctrl Pts',(6.0531903082959,-3.02509108814142,46.1554693993536));
#20558=CARTESIAN_POINT('Ctrl Pts',(6.13118886231285,-2.86901641882408,46.1636780034925));
#20559=CARTESIAN_POINT('Ctrl Pts',(6.20321013436888,-2.7097972730889,46.1718866076314));
#20560=CARTESIAN_POINT('Ctrl Pts',(6.26899750750128,-2.54793234818798,46.1800952117703));
#20561=CARTESIAN_POINT('Ctrl Pts',(6.33474602750618,-2.38616301850946,46.1882989680192));
#20562=CARTESIAN_POINT('Ctrl Pts',(6.39426784844422,-2.2217513534322,46.1965027242682));
#20563=CARTESIAN_POINT('Ctrl Pts',(6.44735351411134,-2.05521815486243,46.2047064805171));
#20564=CARTESIAN_POINT('Ctrl Pts',(6.50042347306808,-1.88873422926848,46.2129078094814));
#20565=CARTESIAN_POINT('Ctrl Pts',(6.54706095771878,-1.72013036021124,46.2211091384457));
#20566=CARTESIAN_POINT('Ctrl Pts',(6.58710555702563,-1.54994496050733,46.22931046741));
#20567=CARTESIAN_POINT('Ctrl Pts',(6.62714463379993,-1.37978303099479,46.2375106653327));
#20568=CARTESIAN_POINT('Ctrl Pts',(6.66059255326884,-1.20804035368517,46.2457108632554));
#20569=CARTESIAN_POINT('Ctrl Pts',(6.68733945682799,-1.03526807598394,46.2539110611781));
#20570=CARTESIAN_POINT('Ctrl Pts',(6.71408751881694,-0.862488315377161,
46.262111614258));
#20571=CARTESIAN_POINT('Ctrl Pts',(6.73413393181892,-0.68867921961648,46.2703121673378));
#20572=CARTESIAN_POINT('Ctrl Pts',(6.74742039178061,-0.514399705076941,
46.2785127204177));
#20573=CARTESIAN_POINT('Ctrl Pts',(6.76070983495631,-0.34008105949039,46.2867151147709));
#20574=CARTESIAN_POINT('Ctrl Pts',(6.76723627480314,-0.165292141927449,
46.2949175091241));
#20575=CARTESIAN_POINT('Ctrl Pts',(6.76699346374685,0.00940540309585271,
46.3031199034773));
#20576=CARTESIAN_POINT('Ctrl Pts',(6.76675042561955,0.18426632103387,46.3113299685111));
#20577=CARTESIAN_POINT('Ctrl Pts',(6.75972548939747,0.359035336963717,46.3195400335449));
#20578=CARTESIAN_POINT('Ctrl Pts',(6.74596454714927,0.533152256494463,46.3277500985788));
#20579=CARTESIAN_POINT('Ctrl Pts',(6.73219701915824,0.707352505294048,46.3359640928041));
#20580=CARTESIAN_POINT('Ctrl Pts',(6.71168709957096,0.880899679843116,46.3441780870294));
#20581=CARTESIAN_POINT('Ctrl Pts',(6.68453229939796,1.05324115866476,46.3523920812547));
#20582=CARTESIAN_POINT('Ctrl Pts',(6.65734047818814,1.2258175963221,46.3606172738899));
#20583=CARTESIAN_POINT('Ctrl Pts',(6.62348574094907,1.39718470157754,46.3688424665251));
#20584=CARTESIAN_POINT('Ctrl Pts',(6.58311649814029,1.56680125475861,46.3770676591603));
#20585=CARTESIAN_POINT('Ctrl Pts',(6.54681252454595,1.71933705774644,46.3844645572802));
#20586=CARTESIAN_POINT('Ctrl Pts',(6.50524075859181,1.87045713637758,46.3918614554002));
#20587=CARTESIAN_POINT('Ctrl Pts',(6.45854278735461,2.01978069698413,46.3992583535202));
#20588=CARTESIAN_POINT('Ctrl Pts',(6.40395921895036,2.19431960239687,46.4079043200111));
#20589=CARTESIAN_POINT('Ctrl Pts',(6.3422476711174,2.366800036713,46.416550286502));
#20590=CARTESIAN_POINT('Ctrl Pts',(6.27357789492636,2.53663347693185,46.4251962529929));
#20591=CARTESIAN_POINT('Ctrl Pts',(6.20499595671444,2.70624967709252,46.4338311601173));
#20592=CARTESIAN_POINT('Ctrl Pts',(6.12947365207117,2.87322535340952,46.4424660672416));
#20593=CARTESIAN_POINT('Ctrl Pts',(6.0472301950042,3.03698797637222,46.451100974366));
#20594=CARTESIAN_POINT('Ctrl Pts',(5.96225632154287,3.20618738624136,46.4600225534375));
#20595=CARTESIAN_POINT('Ctrl Pts',(5.87010742063523,3.37195642021525,46.468944132509));
#20596=CARTESIAN_POINT('Ctrl Pts',(5.77108014181708,3.53368405445713,46.4778657115805));
#20597=CARTESIAN_POINT('Ctrl Pts',(5.67549955778911,3.68978267615799,46.4864767705563));
#20598=CARTESIAN_POINT('Ctrl Pts',(5.57351148267702,3.8421161671724,46.495087829532));
#20599=CARTESIAN_POINT('Ctrl Pts',(5.46543034541433,3.99015790908383,46.5036988885077));
#20600=CARTESIAN_POINT('Ctrl Pts',(5.35745113365368,4.13806004079822,46.5123018268572));
#20601=CARTESIAN_POINT('Ctrl Pts',(5.24339049506426,4.28167824720971,46.5209047652068));
#20602=CARTESIAN_POINT('Ctrl Pts',(5.123606713071,4.42051391240586,46.5295077035563));
#20603=CARTESIAN_POINT('Ctrl Pts',(5.00395706120337,4.55919411377457,46.5381010086051));
#20604=CARTESIAN_POINT('Ctrl Pts',(4.87859724969166,4.69310222727563,46.5466943136539));
#20605=CARTESIAN_POINT('Ctrl Pts',(4.74792660553026,4.82177166075893,46.5552876187026));
#20606=CARTESIAN_POINT('Ctrl Pts',(4.73336775691013,4.83610754175304,46.5562450535432));
#20607=CARTESIAN_POINT('Ctrl Pts',(4.71874302327827,4.85037842513139,46.5572024883837));
#20608=CARTESIAN_POINT('Ctrl Pts',(4.70405298792322,4.86458369100693,46.5581599232242));
#20609=CARTESIAN_POINT('Ctrl Pts',(4.57214264457756,4.99214100817269,46.5667572856872));
#20610=CARTESIAN_POINT('Ctrl Pts',(4.43511836880952,5.1142549251199,46.5753546481503));
#20611=CARTESIAN_POINT('Ctrl Pts',(4.29345710661388,5.23053678637927,46.5839520106134));
#20612=CARTESIAN_POINT('Ctrl Pts',(4.15168870009091,5.34690659646538,46.5925558756206));
#20613=CARTESIAN_POINT('Ctrl Pts',(4.00527654830392,5.45743535961786,46.6011597406278));
#20614=CARTESIAN_POINT('Ctrl Pts',(3.85472814895607,5.56177668534487,46.6097636056351));
#20615=CARTESIAN_POINT('Ctrl Pts',(3.70396633532926,5.66626592316454,46.6183796673024));
#20616=CARTESIAN_POINT('Ctrl Pts',(3.54905680859,5.76455002212831,46.6269957289696));
#20617=CARTESIAN_POINT('Ctrl Pts',(3.39053480736998,5.85632672585919,46.6356117906369));
#20618=CARTESIAN_POINT('Ctrl Pts',(3.29469437704921,5.91181377946244,46.6408209543587));
#20619=CARTESIAN_POINT('Ctrl Pts',(3.19753396979732,5.96492310283268,46.6460301180806));
#20620=CARTESIAN_POINT('Ctrl Pts',(3.09917575053265,6.01559628526636,46.6512392818024));
#20621=CARTESIAN_POINT('Origin',(0.,0.,-3.69717978381041));
#20622=CARTESIAN_POINT('',(3.0991757505326,6.01559628526639,49.0457515827422));
#20623=CARTESIAN_POINT('',(3.09917575053255,6.01559628526641,48.6513920151221));
#20624=CARTESIAN_POINT('',(3.09917575053259,6.01559628526639,-3.69717978381041));
#20625=CARTESIAN_POINT('',(-6.76699998408371,-0.000464124033430669,47.6972016155329));
#20626=CARTESIAN_POINT('Ctrl Pts',(-6.76699998408371,-0.000464124033430669,
47.6972016155329));
#20627=CARTESIAN_POINT('Ctrl Pts',(-6.76698722651986,-0.186471372351812,
47.7059511273078));
#20628=CARTESIAN_POINT('Ctrl Pts',(-6.75930084199275,-0.372477951060072,
47.7147006390827));
#20629=CARTESIAN_POINT('Ctrl Pts',(-6.74396693763965,-0.557852080773529,
47.7234501508577));
#20630=CARTESIAN_POINT('Ctrl Pts',(-6.72863309805146,-0.743225427533112,
47.7321996256778));
#20631=CARTESIAN_POINT('Ctrl Pts',(-6.70565182690122,-0.927966045015493,
47.7409491004979));
#20632=CARTESIAN_POINT('Ctrl Pts',(-6.67510118041105,-1.11144645902309,
47.749698575318));
#20633=CARTESIAN_POINT('Ctrl Pts',(-6.64455066041847,-1.29492611331422,
47.7584480139102));
#20634=CARTESIAN_POINT('Ctrl Pts',(-6.60643087487681,-1.47714529186708,
47.7671974525023));
#20635=CARTESIAN_POINT('Ctrl Pts',(-6.56087129712167,-1.65748508970822,
47.7759468910945));
#20636=CARTESIAN_POINT('Ctrl Pts',(-6.51531190422601,-1.8378241558147,47.7846962941855));
#20637=CARTESIAN_POINT('Ctrl Pts',(-6.46231284972204,-2.01628357860759,
47.7934456972765));
#20638=CARTESIAN_POINT('Ctrl Pts',(-6.40205414272168,-2.19225722798676,
47.8021951003675));
#20639=CARTESIAN_POINT('Ctrl Pts',(-6.34179567521861,-2.36823017796141,
47.8109444686842));
#20640=CARTESIAN_POINT('Ctrl Pts',(-6.27427770580163,-2.5417171031626,47.8196938370009));
#20641=CARTESIAN_POINT('Ctrl Pts',(-6.19972955465985,-2.71212876705314,
47.8284432053175));
#20642=CARTESIAN_POINT('Ctrl Pts',(-6.12518169361748,-2.88253976779748,
47.8371925395866));
#20643=CARTESIAN_POINT('Ctrl Pts',(-6.04360382045395,-3.0498752686225,47.8459418738556));
#20644=CARTESIAN_POINT('Ctrl Pts',(-5.95527300671056,-3.21356693030418,
47.8546912081246));
#20645=CARTESIAN_POINT('Ctrl Pts',(-5.86694252936545,-3.377257968584,47.8634405090728));
#20646=CARTESIAN_POINT('Ctrl Pts',(-5.77185929899606,-3.53730494329142,
47.872189810021));
#20647=CARTESIAN_POINT('Ctrl Pts',(-5.67034625435664,-3.69316427412912,
47.8809391109691));
#20648=CARTESIAN_POINT('Ctrl Pts',(-5.56883358788884,-3.84902302433627,
47.8896883793231));
#20649=CARTESIAN_POINT('Ctrl Pts',(-5.46089131148301,-4.00069392176395,
47.898437647677));
#20650=CARTESIAN_POINT('Ctrl Pts',(-5.34688603536768,-4.14766183828794,
47.907186916031));
#20651=CARTESIAN_POINT('Ctrl Pts',(-5.23288117449473,-4.29462921950947,
47.9159361525174));
#20652=CARTESIAN_POINT('Ctrl Pts',(-5.11281353374605,-4.43689342767989,
47.9246853890038));
#20653=CARTESIAN_POINT('Ctrl Pts',(-4.98709090241752,-4.57397128664188,
47.9334346254902));
#20654=CARTESIAN_POINT('Ctrl Pts',(-4.86136871856977,-4.71104865770678,
47.9421838308358));
#20655=CARTESIAN_POINT('Ctrl Pts',(-4.72999177811196,-4.84293950531728,
47.9509330361813));
#20656=CARTESIAN_POINT('Ctrl Pts',(-4.59340627727753,-4.96919588785424,
47.9596822415268));
#20657=CARTESIAN_POINT('Ctrl Pts',(-4.4568212512464,-5.09545183149432,47.968431416458));
#20658=CARTESIAN_POINT('Ctrl Pts',(-4.31502791149598,-5.21607315474496,
47.9771805913893));
#20659=CARTESIAN_POINT('Ctrl Pts',(-4.16850782818983,-5.33065019358053,
47.9859297663205));
#20660=CARTESIAN_POINT('Ctrl Pts',(-4.02198824205588,-5.44522684363309,
47.994678911564));
#20661=CARTESIAN_POINT('Ctrl Pts',(-3.87074217018864,-5.55375907379691,
48.0034280568075));
#20662=CARTESIAN_POINT('Ctrl Pts',(-3.7152832834129,-5.65587828051423,48.012177202051));
#20663=CARTESIAN_POINT('Ctrl Pts',(-3.55982491123215,-5.75799714919987,
48.0209263183334));
#20664=CARTESIAN_POINT('Ctrl Pts',(-3.40015399154343,-5.85370287959801,
48.0296754346158));
#20665=CARTESIAN_POINT('Ctrl Pts',(-3.23681280454993,-5.94267043241518,
48.0384245508981));
#20666=CARTESIAN_POINT('Ctrl Pts',(-3.07347214468129,-6.03163769812162,
48.0471736389459));
#20667=CARTESIAN_POINT('Ctrl Pts',(-2.90646149284465,-6.11386669270314,
48.0559227269936));
#20668=CARTESIAN_POINT('Ctrl Pts',(-2.73634805305211,-6.18907814884882,
48.0646718150414));
#20669=CARTESIAN_POINT('Ctrl Pts',(-2.56623514811494,-6.2642893685214,48.073420875581));
#20670=CARTESIAN_POINT('Ctrl Pts',(-2.39301973680805,-6.33248297804565,
48.0821699361207));
#20671=CARTESIAN_POINT('Ctrl Pts',(-2.21729009214273,-6.39342737874497,
48.0909189966604));
#20672=CARTESIAN_POINT('Ctrl Pts',(-2.04156098540153,-6.45437159288803,
48.0996680304184));
#20673=CARTESIAN_POINT('Ctrl Pts',(-1.86331793141591,-6.50806654872686,
48.1084170641764));
#20674=CARTESIAN_POINT('Ctrl Pts',(-1.68316627434103,-6.55432988892998,
48.1171660979344));
#20675=CARTESIAN_POINT('Ctrl Pts',(-1.50301515376888,-6.60059309135803,
48.1259151056372));
#20676=CARTESIAN_POINT('Ctrl Pts',(-1.32095571900333,-6.63942465117082,
48.13466411334));
#20677=CARTESIAN_POINT('Ctrl Pts',(-1.13760627160799,-6.67069269047812,
48.1434131210429));
#20678=CARTESIAN_POINT('Ctrl Pts',(-0.954257355016002,-6.7019606392633,
48.152162103417));
#20679=CARTESIAN_POINT('Ctrl Pts',(-0.769618715712151,-6.72566506319355,
48.1609110857912));
#20680=CARTESIAN_POINT('Ctrl Pts',(-0.584317411004386,-6.74172545890124,
48.1696600681653));
#20681=CARTESIAN_POINT('Ctrl Pts',(-0.391031954869637,-6.75847785530213,
48.1787860214422));
#20682=CARTESIAN_POINT('Ctrl Pts',(-0.197025793659618,-6.76691286680797,
48.187911974719));
#20683=CARTESIAN_POINT('Ctrl Pts',(-0.003015734995512,-6.76699932801404,
48.1970379279958));
#20684=CARTESIAN_POINT('Ctrl Pts',(0.184931509335365,-6.76708308730742,
48.2058786952328));
#20685=CARTESIAN_POINT('Ctrl Pts',(0.372882094257411,-6.75933222422522,
48.2147194624697));
#20686=CARTESIAN_POINT('Ctrl Pts',(0.560184265596068,-6.74377361635002,
48.2235602297067));
#20687=CARTESIAN_POINT('Ctrl Pts',(0.745562970101919,-6.72837478487249,
48.2323102082334));
#20688=CARTESIAN_POINT('Ctrl Pts',(0.930306227486469,-6.70532786008224,
48.2410601867601));
#20689=CARTESIAN_POINT('Ctrl Pts',(1.1137864824089,-6.67471113019906,48.2498101652868));
#20690=CARTESIAN_POINT('Ctrl Pts',(1.29726485910632,-6.64409471372894,48.258560054243));
#20691=CARTESIAN_POINT('Ctrl Pts',(1.47947997644983,-6.60590869441571,48.2673099431992));
#20692=CARTESIAN_POINT('Ctrl Pts',(1.65981287961014,-6.56028278389585,48.2760598321554));
#20693=CARTESIAN_POINT('Ctrl Pts',(1.84014399669517,-6.51465732526974,48.2848096344498));
#20694=CARTESIAN_POINT('Ctrl Pts',(2.01859265899936,-6.46159219320578,48.2935594367442));
#20695=CARTESIAN_POINT('Ctrl Pts',(2.19455271771757,-6.40126763767603,48.3023092390387));
#20696=CARTESIAN_POINT('Ctrl Pts',(2.37051109214448,-6.34094365957348,48.3110589575799));
#20697=CARTESIAN_POINT('Ctrl Pts',(2.54398063950056,-6.2733604900174,48.3198086761212));
#20698=CARTESIAN_POINT('Ctrl Pts',(2.71437213515056,-6.19874768900285,48.3285583946625));
#20699=CARTESIAN_POINT('Ctrl Pts',(2.88476205643078,-6.12413557738972,48.3373080323588));
#20700=CARTESIAN_POINT('Ctrl Pts',(3.05207372035493,-6.04249407926827,48.3460576700551));
#20701=CARTESIAN_POINT('Ctrl Pts',(3.21573882928381,-5.95410050148941,48.3548073077514));
#20702=CARTESIAN_POINT('Ctrl Pts',(3.37940248037333,-5.86570771107224,48.3635568675107));
#20703=CARTESIAN_POINT('Ctrl Pts',(3.53941938927846,-5.77056309755689,48.37230642727));
#20704=CARTESIAN_POINT('Ctrl Pts',(3.69524604569606,-5.66898982727678,48.3810559870293));
#20705=CARTESIAN_POINT('Ctrl Pts',(3.85107136586769,-5.56741742800858,48.3898054717593));
#20706=CARTESIAN_POINT('Ctrl Pts',(4.00270626535449,-5.45941663879865,48.3985549564893));
#20707=CARTESIAN_POINT('Ctrl Pts',(4.14963571284667,-5.34535428673044,48.4073044412193));
#20708=CARTESIAN_POINT('Ctrl Pts',(4.2965639492015,-5.23129287487658,48.4160538538275));
#20709=CARTESIAN_POINT('Ctrl Pts',(4.43878658479358,-5.11117017589603,48.4248032664356));
#20710=CARTESIAN_POINT('Ctrl Pts',(4.57582056523246,-4.98539418248905,48.4335526790438));
#20711=CARTESIAN_POINT('Ctrl Pts',(4.71285346162535,-4.85961918406859,48.4423020224372));
#20712=CARTESIAN_POINT('Ctrl Pts',(4.84469757387159,-4.7281911745026,48.4510513658306));
#20713=CARTESIAN_POINT('Ctrl Pts',(4.97090510496334,-4.59155653754252,48.4598007092241));
#20714=CARTESIAN_POINT('Ctrl Pts',(5.0971116795788,-4.45492293608158,48.4685499863098));
#20715=CARTESIAN_POINT('Ctrl Pts',(5.21768156407691,-4.31308299669927,48.4772992633954));
#20716=CARTESIAN_POINT('Ctrl Pts',(5.33220525957991,-4.16651845906247,48.4860485404811));
#20717=CARTESIAN_POINT('Ctrl Pts',(5.44672812519458,-4.01995498349585,48.4947977541657));
#20718=CARTESIAN_POINT('Ctrl Pts',(5.55520471305057,-3.86866720398892,48.5035469678503));
#20719=CARTESIAN_POINT('Ctrl Pts',(5.65726660280775,-3.713168941047,48.512296181535));
#20720=CARTESIAN_POINT('Ctrl Pts',(5.75932778687966,-3.5576717532648,48.521045334725));
#20721=CARTESIAN_POINT('Ctrl Pts',(5.85497420437281,-3.397964379865,48.529794487915));
#20722=CARTESIAN_POINT('Ctrl Pts',(5.94388101469654,-3.23458922942776,48.5385436411051));
#20723=CARTESIAN_POINT('Ctrl Pts',(6.03278723982154,-3.07121515435168,48.5472927367068));
#20724=CARTESIAN_POINT('Ctrl Pts',(6.11495380958366,-2.90417360223718,48.5560418323085));
#20725=CARTESIAN_POINT('Ctrl Pts',(6.19010166819865,-2.73403188301899,48.5647909279102));
#20726=CARTESIAN_POINT('Ctrl Pts',(6.26524905713621,-2.56389122719403,48.5735399688297));
#20727=CARTESIAN_POINT('Ctrl Pts',(6.33337770694414,-2.3906507051453,48.5822890097492));
#20728=CARTESIAN_POINT('Ctrl Pts',(6.39425624059827,-2.21489867252887,48.5910380506687));
#20729=CARTESIAN_POINT('Ctrl Pts',(6.45513441397643,-2.03914768000375,48.5997870398119));
#20730=CARTESIAN_POINT('Ctrl Pts',(6.50876246327865,-1.86088547739572,48.608536028955));
#20731=CARTESIAN_POINT('Ctrl Pts',(6.55495826025521,-1.68071746772384,48.6172850180981));
#20732=CARTESIAN_POINT('Ctrl Pts',(6.6020907396664,-1.49689630731125,48.6262114048615));
#20733=CARTESIAN_POINT('Ctrl Pts',(6.64148625753709,-1.3110915225784,48.6351377916249));
#20734=CARTESIAN_POINT('Ctrl Pts',(6.67300554640953,-1.12395995372949,48.6440641783884));
#20735=CARTESIAN_POINT('Ctrl Pts',(6.70390170574978,-0.940527935572548,
48.6528140924137));
#20736=CARTESIAN_POINT('Ctrl Pts',(6.72723010571988,-0.755821395994563,
48.6615640064391));
#20737=CARTESIAN_POINT('Ctrl Pts',(6.74291150312266,-0.570467756368566,
48.6703139204645));
#20738=CARTESIAN_POINT('Ctrl Pts',(6.75859259215796,-0.385117761636668,
48.6790636624268));
#20739=CARTESIAN_POINT('Ctrl Pts',(6.76662695537733,-0.199120977954146,
48.6878134043892));
#20740=CARTESIAN_POINT('Ctrl Pts',(6.76698730228438,-0.0131091846437382,
48.6965631463516));
#20741=CARTESIAN_POINT('Ctrl Pts',(6.76734764258434,0.172899198075617,48.7053127278843));
#20742=CARTESIAN_POINT('Ctrl Pts',(6.76003424758483,0.35892230324573,48.7140623094171));
#20743=CARTESIAN_POINT('Ctrl Pts',(6.74507195794377,0.544328285284334,48.7228118909499));
#20744=CARTESIAN_POINT('Ctrl Pts',(6.73010992275648,0.729731114246022,48.7315613236843));
#20745=CARTESIAN_POINT('Ctrl Pts',(6.70749927628582,0.914516555404612,48.7403107564188));
#20746=CARTESIAN_POINT('Ctrl Pts',(6.67731681518376,1.09805698834996,48.7490601891532));
#20747=CARTESIAN_POINT('Ctrl Pts',(6.64713482726716,1.28159454384065,48.7578094847184));
#20748=CARTESIAN_POINT('Ctrl Pts',(6.60938130876791,1.46388684739616,48.7665587802837));
#20749=CARTESIAN_POINT('Ctrl Pts',(6.56418448481257,1.64431476589672,48.7753080758489));
#20750=CARTESIAN_POINT('Ctrl Pts',(6.51898830937794,1.82474009547105,48.7840572458721));
#20751=CARTESIAN_POINT('Ctrl Pts',(6.46634911184241,2.00330081555438,48.7928064158953));
#20752=CARTESIAN_POINT('Ctrl Pts',(6.40644566956322,2.17939048427185,48.8015555859186));
#20753=CARTESIAN_POINT('Ctrl Pts',(6.34654300724299,2.35547786025438,48.8103046420252));
#20754=CARTESIAN_POINT('Ctrl Pts',(6.27937638173278,2.52909397798304,48.8190536981319));
#20755=CARTESIAN_POINT('Ctrl Pts',(6.20517390364207,2.699649204167,48.8278027542386));
#20756=CARTESIAN_POINT('Ctrl Pts',(6.12815443731935,2.87667930932306,48.8368839554263));
#20757=CARTESIAN_POINT('Ctrl Pts',(6.04355456528832,3.05041126288029,48.8459651566139));
#20758=CARTESIAN_POINT('Ctrl Pts',(5.95168380961829,3.22020943889175,48.8550463578016));
#20759=CARTESIAN_POINT('Ctrl Pts',(5.86316590408054,3.38381078074475,48.8637961378925));
#20760=CARTESIAN_POINT('Ctrl Pts',(5.76789857594155,3.54376012680152,48.8725459179834));
#20761=CARTESIAN_POINT('Ctrl Pts',(5.6662054246254,3.69951416890729,48.8812956980743));
#20762=CARTESIAN_POINT('Ctrl Pts',(5.56451592882081,3.85526261220236,48.8900451636413));
#20763=CARTESIAN_POINT('Ctrl Pts',(5.45640122875607,4.00681581333296,48.8987946292084));
#20764=CARTESIAN_POINT('Ctrl Pts',(5.34222853680848,4.1536590207321,48.9075440947754));
#20765=CARTESIAN_POINT('Ctrl Pts',(5.2280593420745,4.30049773018996,48.9162932923383));
#20766=CARTESIAN_POINT('Ctrl Pts',(5.10783270268491,4.44262650838489,48.9250424899013));
#20767=CARTESIAN_POINT('Ctrl Pts',(4.98195694431792,4.57956264341503,48.9337916874642));
#20768=CARTESIAN_POINT('Ctrl Pts',(4.85608437269241,4.71649531169298,48.9425406635275));
#20769=CARTESIAN_POINT('Ctrl Pts',(4.72456316218971,4.8482353889234,48.9512896395909));
#20770=CARTESIAN_POINT('Ctrl Pts',(4.58783997564082,4.97433546897594,48.9600386156542));
#20771=CARTESIAN_POINT('Ctrl Pts',(4.45110790519902,5.10044374266142,48.9687881602017));
#20772=CARTESIAN_POINT('Ctrl Pts',(4.30917339295186,5.22091109149112,48.9775377047492));
#20773=CARTESIAN_POINT('Ctrl Pts',(4.16251852921304,5.33532833984546,48.9862872492967));
#20774=CARTESIAN_POINT('Ctrl Pts',(4.01587228434862,5.44973886392304,48.9950362796354));
#20775=CARTESIAN_POINT('Ctrl Pts',(3.86450646904683,5.55809982276747,49.003785309974));
#20776=CARTESIAN_POINT('Ctrl Pts',(3.708935147323,5.6600432041595,49.0125343403127));
#20777=CARTESIAN_POINT('Ctrl Pts',(3.55336172014134,5.76198796522413,49.0212834890583));
#20778=CARTESIAN_POINT('Ctrl Pts',(3.39358291230957,5.85751481797819,49.0300326378038));
#20779=CARTESIAN_POINT('Ctrl Pts',(3.23014137446734,5.94629932823384,49.0387817865494));
#20780=CARTESIAN_POINT('Ctrl Pts',(3.18674080140078,5.96987533391392,49.041105051947));
#20781=CARTESIAN_POINT('Ctrl Pts',(3.14308210500722,5.9929761653931,49.0434283173446));
#20782=CARTESIAN_POINT('Ctrl Pts',(3.0991757505326,6.01559628526638,49.0457515827422));
#20783=CARTESIAN_POINT('Ctrl Pts',(3.09917575053261,6.01559628526638,47.0456199604263));
#20784=CARTESIAN_POINT('Ctrl Pts',(2.94420070234753,6.0954378983828,47.0538464887508));
#20785=CARTESIAN_POINT('Ctrl Pts',(2.78631654012032,6.16919515578224,47.0620730170753));
#20786=CARTESIAN_POINT('Ctrl Pts',(2.62604879104489,6.23667834243932,47.0702995453998));
#20787=CARTESIAN_POINT('Ctrl Pts',(2.60052446512196,6.24742575020221,47.071609706623));
#20788=CARTESIAN_POINT('Ctrl Pts',(2.57493971154706,6.25801412625621,47.0729198678462));
#20789=CARTESIAN_POINT('Ctrl Pts',(2.54929668466128,6.26844282207113,47.0742300290694));
#20790=CARTESIAN_POINT('Ctrl Pts',(2.38831649159949,6.33391143750199,47.0824548773914));
#20791=CARTESIAN_POINT('Ctrl Pts',(2.22458678934626,6.39326674151772,47.0906797257135));
#20792=CARTESIAN_POINT('Ctrl Pts',(2.05861209918271,6.44627064472929,47.0989045740355));
#20793=CARTESIAN_POINT('Ctrl Pts',(1.89282433332024,6.4992148537938,47.1071201593547));
#20794=CARTESIAN_POINT('Ctrl Pts',(1.72479695279772,6.54582179752411,47.1153357446739));
#20795=CARTESIAN_POINT('Ctrl Pts',(1.55505540613306,6.58590097738011,47.1235513299931));
#20796=CARTESIAN_POINT('Ctrl Pts',(1.38547092162903,6.62594307189839,47.1317593134164));
#20797=CARTESIAN_POINT('Ctrl Pts',(1.21417577674592,6.65946934970275,47.1399672968396));
#20798=CARTESIAN_POINT('Ctrl Pts',(1.041711658641,6.68633874555062,47.1481752802628));
#20799=CARTESIAN_POINT('Ctrl Pts',(0.869372481601259,6.71318867595272,47.1563773174394));
#20800=CARTESIAN_POINT('Ctrl Pts',(0.695866371181164,6.73339127501541,47.1645793546159));
#20801=CARTESIAN_POINT('Ctrl Pts',(0.521746405112546,6.74685628191028,47.1727813917924));
#20802=CARTESIAN_POINT('Ctrl Pts',(0.347717614848954,6.76031423801786,47.1809791340718));
#20803=CARTESIAN_POINT('Ctrl Pts',(0.173075966149704,6.76704160281862,47.1891768763513));
#20804=CARTESIAN_POINT('Ctrl Pts',(-0.00161903260454401,6.76699980631989,
47.1973746186307));
#20805=CARTESIAN_POINT('Ctrl Pts',(-0.176280815995487,6.76695801776807,
47.205570802245));
#20806=CARTESIAN_POINT('Ctrl Pts',(-0.350995570826527,6.76014962539898,
47.2137669858594));
#20807=CARTESIAN_POINT('Ctrl Pts',(-0.525202157850227,6.7465881520506,47.2219631694738));
#20808=CARTESIAN_POINT('Ctrl Pts',(-0.699395920838457,6.73302767701587,
47.2301587497346));
#20809=CARTESIAN_POINT('Ctrl Pts',(-0.873081232707041,6.71271513798809,
47.2383543299955));
#20810=CARTESIAN_POINT('Ctrl Pts',(-1.04570050552152,6.68571607628922,47.2465499102564));
#20811=CARTESIAN_POINT('Ctrl Pts',(-1.21833847718382,6.65871408993809,47.2547463782971));
#20812=CARTESIAN_POINT('Ctrl Pts',(-1.38990982513253,6.62502419332592,47.2629428463378));
#20813=CARTESIAN_POINT('Ctrl Pts',(-1.55986555218957,6.58476335634716,47.2711393143786));
#20814=CARTESIAN_POINT('Ctrl Pts',(-1.72987061113206,6.54449083313086,47.2793381615519));
#20815=CARTESIAN_POINT('Ctrl Pts',(-1.89825876600454,6.49764365313928,47.2875370087253));
#20816=CARTESIAN_POINT('Ctrl Pts',(-2.06449456563181,6.44438912453902,47.2957358558987));
#20817=CARTESIAN_POINT('Ctrl Pts',(-2.23090409783499,6.39107893977773,47.3039432716647));
#20818=CARTESIAN_POINT('Ctrl Pts',(-2.39515643856376,6.33134813769041,47.3121506874306));
#20819=CARTESIAN_POINT('Ctrl Pts',(-2.55673362096148,6.26541317005074,47.3203581031966));
#20820=CARTESIAN_POINT('Ctrl Pts',(-2.71839740304603,6.19944286358745,47.3285699178487));
#20821=CARTESIAN_POINT('Ctrl Pts',(-2.87738284207945,6.12726191087421,47.3367817325009));
#20822=CARTESIAN_POINT('Ctrl Pts',(-3.03319520514806,6.04913347905854,47.344993547153));
#20823=CARTESIAN_POINT('Ctrl Pts',(-3.18923702560847,5.97088999124964,47.3532174549506));
#20824=CARTESIAN_POINT('Ctrl Pts',(-3.34209611727311,5.8866816937324,47.3614413627483));
#20825=CARTESIAN_POINT('Ctrl Pts',(-3.49130433125497,5.79681663213184,47.3696652705459));
#20826=CARTESIAN_POINT('Ctrl Pts',(-3.6291699653541,5.71378297486666,47.3772640094694));
#20827=CARTESIAN_POINT('Ctrl Pts',(-3.76391883116865,5.6259205046909,47.3848627483929));
#20828=CARTESIAN_POINT('Ctrl Pts',(-3.89520661056735,5.53350291054341,47.3924614873164));
#20829=CARTESIAN_POINT('Ctrl Pts',(-4.03509486809112,5.43503116954024,47.4005580089596));
#20830=CARTESIAN_POINT('Ctrl Pts',(-4.17148000542102,5.33108698804352,47.4086545306027));
#20831=CARTESIAN_POINT('Ctrl Pts',(-4.30389637344467,5.22195030679628,47.4167510522459));
#20832=CARTESIAN_POINT('Ctrl Pts',(-4.43615862108418,5.11294065053463,47.424838150288));
#20833=CARTESIAN_POINT('Ctrl Pts',(-4.5644610092719,4.99875075525649,47.4329252483302));
#20834=CARTESIAN_POINT('Ctrl Pts',(-4.68836577643363,4.87970443227517,47.4410123463723));
#20835=CARTESIAN_POINT('Ctrl Pts',(-4.8121531637216,4.76077088657177,47.4490917831874));
#20836=CARTESIAN_POINT('Ctrl Pts',(-4.93155095663324,4.63699032549633,47.4571712200025));
#20837=CARTESIAN_POINT('Ctrl Pts',(-5.0461535513924,4.50872746301768,47.4652506568177));
#20838=CARTESIAN_POINT('Ctrl Pts',(-5.16067237307605,4.38055835910084,47.4733241876647));
#20839=CARTESIAN_POINT('Ctrl Pts',(-5.27040272860054,4.24791375180502,47.4813977185117));
#20840=CARTESIAN_POINT('Ctrl Pts',(-5.37497511899457,4.11119586862379,47.4894712493587));
#20841=CARTESIAN_POINT('Ctrl Pts',(-5.47949367726756,3.9745483655267,47.4975406240868));
#20842=CARTESIAN_POINT('Ctrl Pts',(-5.57885933259808,3.8338320556282,47.5056099988149));
#20843=CARTESIAN_POINT('Ctrl Pts',(-5.67274227269699,3.68948290517203,47.513679373543));
#20844=CARTESIAN_POINT('Ctrl Pts',(-5.76661107747611,3.54515548839186,47.5217475333199));
#20845=CARTESIAN_POINT('Ctrl Pts',(-5.8549986018577,3.39719662643701,47.5298156930968));
#20846=CARTESIAN_POINT('Ctrl Pts',(-5.93761777482627,3.24607211257962,47.5378838528736));
#20847=CARTESIAN_POINT('Ctrl Pts',(-6.0202340176665,3.09495295842514,47.5459517265094));
#20848=CARTESIAN_POINT('Ctrl Pts',(-6.09708213755128,2.94066870104229,47.5540196001451));
#20849=CARTESIAN_POINT('Ctrl Pts',(-6.16792066567482,2.78371041273002,47.5620874737809));
#20850=CARTESIAN_POINT('Ctrl Pts',(-6.23877054869785,2.62672696514868,47.5701566406379));
#20851=CARTESIAN_POINT('Ctrl Pts',(-6.30360876960811,2.46706897157694,47.578225807495));
#20852=CARTESIAN_POINT('Ctrl Pts',(-6.3622417676081,2.30524807569663,47.5862949743521));
#20853=CARTESIAN_POINT('Ctrl Pts',(-6.42089564396256,2.14336955775808,47.5943670145217));
#20854=CARTESIAN_POINT('Ctrl Pts',(-6.47333977272037,1.97932695298936,47.6024390546912));
#20855=CARTESIAN_POINT('Ctrl Pts',(-6.51943030803423,1.81364755635838,47.6105110948607));
#20856=CARTESIAN_POINT('Ctrl Pts',(-6.56557201593449,1.6477842121299,47.6185920971127));
#20857=CARTESIAN_POINT('Ctrl Pts',(-6.60534594483719,1.48028080479,47.6266730993646));
#20858=CARTESIAN_POINT('Ctrl Pts',(-6.63865911135347,1.31167610454852,47.6347541016165));
#20859=CARTESIAN_POINT('Ctrl Pts',(-6.67199286151105,1.14296722631874,47.6428400969828));
#20860=CARTESIAN_POINT('Ctrl Pts',(-6.69885784039119,0.973156065076676,
47.6509260923491));
#20861=CARTESIAN_POINT('Ctrl Pts',(-6.71921295318792,0.802786577934436,
47.6590120877154));
#20862=CARTESIAN_POINT('Ctrl Pts',(-6.73959751400368,0.632170614933792,
47.6671097812014));
#20863=CARTESIAN_POINT('Ctrl Pts',(-6.75345337276775,0.460995081396149,
47.6752074746874));
#20864=CARTESIAN_POINT('Ctrl Pts',(-6.7607915301348,0.289804910340657,47.6833051681734));
#20865=CARTESIAN_POINT('Ctrl Pts',(-6.76494034071624,0.193018270645183,
47.6878834014736));
#20866=CARTESIAN_POINT('Ctrl Pts',(-6.76700672276788,0.0962268956752369,
47.6924616347738));
#20867=CARTESIAN_POINT('Ctrl Pts',(-6.76699998356599,-0.000471612025413017,
47.697039868074));
#20868=CARTESIAN_POINT('',(-6.767,1.57869390845534E-12,47.3028202161899));
#20869=CARTESIAN_POINT('Ctrl Pts',(3.09917575053265,6.01559628526636,46.6512392818024));
#20870=CARTESIAN_POINT('Ctrl Pts',(2.93619253716553,6.09956362593521,46.6598710590822));
#20871=CARTESIAN_POINT('Ctrl Pts',(2.76991958324212,6.17683924023712,46.6685028363621));
#20872=CARTESIAN_POINT('Ctrl Pts',(2.60092745572062,6.24719660088257,46.6771346136419));
#20873=CARTESIAN_POINT('Ctrl Pts',(2.43165828803,6.31766930308491,46.6857805415752));
#20874=CARTESIAN_POINT('Ctrl Pts',(2.25966132069246,6.3812009694572,46.6944264695086));
#20875=CARTESIAN_POINT('Ctrl Pts',(2.08552446834769,6.43761420806832,46.7030723974419));
#20876=CARTESIAN_POINT('Ctrl Pts',(1.99160676613167,6.46803971348879,46.7077354292705));
#20877=CARTESIAN_POINT('Ctrl Pts',(1.89706683779563,6.49639548331203,46.7123984610992));
#20878=CARTESIAN_POINT('Ctrl Pts',(1.80199820030188,6.52265984749387,46.7170614929278));
#20879=CARTESIAN_POINT('Ctrl Pts',(1.63428887905408,6.56899246365482,46.7252874854692));
#20880=CARTESIAN_POINT('Ctrl Pts',(1.46457135062787,6.60891357559464,46.7335134780105));
#20881=CARTESIAN_POINT('Ctrl Pts',(1.29337652475002,6.64224857749434,46.7417394705518));
#20882=CARTESIAN_POINT('Ctrl Pts',(1.12236117451943,6.67554863195325,46.7499568392032));
#20883=CARTESIAN_POINT('Ctrl Pts',(0.949871959778354,6.70227625823853,46.7581742078546));
#20884=CARTESIAN_POINT('Ctrl Pts',(0.776454648957584,6.72230668581196,46.766391576506));
#20885=CARTESIAN_POINT('Ctrl Pts',(0.603184443719548,6.74232012207289,46.7746019745684));
#20886=CARTESIAN_POINT('Ctrl Pts',(0.428988064300652,6.75564763335025,46.7828123726308));
#20887=CARTESIAN_POINT('Ctrl Pts',(0.254421263079605,6.76221552606045,46.7910227706932));
#20888=CARTESIAN_POINT('Ctrl Pts',(0.079967622301007,6.76877916122775,46.799227846482));
#20889=CARTESIAN_POINT('Ctrl Pts',(-0.0948556052224034,6.76859189268669,
46.8074329222707));
#20890=CARTESIAN_POINT('Ctrl Pts',(-0.26948765704395,6.76163185944791,46.8156379980595));
#20891=CARTESIAN_POINT('Ctrl Pts',(-0.444041432302684,6.75467494595418,
46.823839396029));
#20892=CARTESIAN_POINT('Ctrl Pts',(-0.618403845327353,6.74095133021332,
46.8320407939985));
#20893=CARTESIAN_POINT('Ctrl Pts',(-0.792014147959577,6.72049124613907,
46.840242191968));
#20894=CARTESIAN_POINT('Ctrl Pts',(-0.965610851987389,6.70003276466896,
46.8484429475357));
#20895=CARTESIAN_POINT('Ctrl Pts',(-1.13845520640495,6.67283889913459,46.8566437031034));
#20896=CARTESIAN_POINT('Ctrl Pts',(-1.30999122033133,6.63899179112724,46.8648444586711));
#20897=CARTESIAN_POINT('Ctrl Pts',(-1.48152636293633,6.6051448550471,46.8730451725829));
#20898=CARTESIAN_POINT('Ctrl Pts',(-1.65175282648683,6.56464481213974,46.8812458864946));
#20899=CARTESIAN_POINT('Ctrl Pts',(-1.82012457539106,6.51762499151781,46.8894466004064));
#20900=CARTESIAN_POINT('Ctrl Pts',(-1.98852598220045,6.47059688857186,46.897648758836));
#20901=CARTESIAN_POINT('Ctrl Pts',(-2.15507167829978,6.41704681625701,46.9058509172656));
#20902=CARTESIAN_POINT('Ctrl Pts',(-2.31923050400422,6.35715808119449,46.9140530756952));
#20903=CARTESIAN_POINT('Ctrl Pts',(-2.48344799550768,6.29724794356357,46.9222581653482));
#20904=CARTESIAN_POINT('Ctrl Pts',(-2.64527658093408,6.23099475339782,46.9304632550011));
#20905=CARTESIAN_POINT('Ctrl Pts',(-2.80420475171964,6.15863010014671,46.938668344654));
#20906=CARTESIAN_POINT('Ctrl Pts',(-2.96331447915035,6.08618277883488,46.9468828076518));
#20907=CARTESIAN_POINT('Ctrl Pts',(-3.11951684590354,6.00761019503864,46.9550972706496));
#20908=CARTESIAN_POINT('Ctrl Pts',(-3.27232370178156,5.92319057525238,46.9633117336474));
#20909=CARTESIAN_POINT('Ctrl Pts',(-3.4252210908921,5.83872093950955,46.9715310634548));
#20910=CARTESIAN_POINT('Ctrl Pts',(-3.57471865275116,5.74839754733832,46.9797503932623));
#20911=CARTESIAN_POINT('Ctrl Pts',(-3.72035705695915,5.65254211560907,46.9879697230698));
#20912=CARTESIAN_POINT('Ctrl Pts',(-3.86622111904454,5.55653816169999,46.9962017882305));
#20913=CARTESIAN_POINT('Ctrl Pts',(-4.00821378275411,5.45498524724284,47.0044338533911));
#20914=CARTESIAN_POINT('Ctrl Pts',(-4.14590759872467,5.34824636519645,47.0126659185518));
#20915=CARTESIAN_POINT('Ctrl Pts',(-4.26967668747936,5.25230179373944,47.0200654898131));
#20916=CARTESIAN_POINT('Ctrl Pts',(-4.38997275868149,5.15216776742733,47.0274650610743));
#20917=CARTESIAN_POINT('Ctrl Pts',(-4.50651135356984,5.04813276570121,47.0348646323356));
#20918=CARTESIAN_POINT('Ctrl Pts',(-4.63308913785861,4.93513569361889,47.0429016378944));
#20919=CARTESIAN_POINT('Ctrl Pts',(-4.75564675297842,4.81716699154376,47.0509386434532));
#20920=CARTESIAN_POINT('Ctrl Pts',(-4.87375585167972,4.69454927529978,47.058975649012));
#20921=CARTESIAN_POINT('Ctrl Pts',(-4.99172100065018,4.57208100382716,47.06700285918));
#20922=CARTESIAN_POINT('Ctrl Pts',(-5.10524816249726,4.44497525956722,47.0750300693479));
#20923=CARTESIAN_POINT('Ctrl Pts',(-5.21394127849122,4.31359540806105,47.0830572795159));
#20924=CARTESIAN_POINT('Ctrl Pts',(-5.32252614494393,4.18234640024746,47.0910764952326));
#20925=CARTESIAN_POINT('Ctrl Pts',(-5.42628630775912,4.0468320435427,47.0990957109493));
#20926=CARTESIAN_POINT('Ctrl Pts',(-5.5248619918402,3.90745300305961,47.107114926666));
#20927=CARTESIAN_POINT('Ctrl Pts',(-5.62495660593286,3.76592630304417,47.1152577086306));
#20928=CARTESIAN_POINT('Ctrl Pts',(-5.71970536117816,3.62041510074397,47.1234004905953));
#20929=CARTESIAN_POINT('Ctrl Pts',(-5.80877294194265,3.47137521869287,47.1315432725599));
#20930=CARTESIAN_POINT('Ctrl Pts',(-5.89637343232061,3.32479027003381,47.1395519294362));
#20931=CARTESIAN_POINT('Ctrl Pts',(-5.97847825535804,3.17479232576088,47.1475605863125));
#20932=CARTESIAN_POINT('Ctrl Pts',(-6.05481135274774,3.0218452115615,47.1555692431888));
#20933=CARTESIAN_POINT('Ctrl Pts',(-6.13112427005438,2.86893853179454,47.1635757828267));
#20934=CARTESIAN_POINT('Ctrl Pts',(-6.20166832973967,2.71308457008167,47.1715823224647));
#20935=CARTESIAN_POINT('Ctrl Pts',(-6.26621333059703,2.55477190673612,47.1795888621026));
#20936=CARTESIAN_POINT('Ctrl Pts',(-6.33075423601889,2.39646928846443,47.1875948937188));
#20937=CARTESIAN_POINT('Ctrl Pts',(-6.38929669877065,2.2357086280691,47.1956009253349));
#20938=CARTESIAN_POINT('Ctrl Pts',(-6.44165866722065,2.07299845996594,47.2036069569511));
#20939=CARTESIAN_POINT('Ctrl Pts',(-6.49558069562354,1.90544054406604,47.2118515183566));
#20940=CARTESIAN_POINT('Ctrl Pts',(-6.54294808136012,1.73581554642876,47.2200960797621));
#20941=CARTESIAN_POINT('Ctrl Pts',(-6.58361741644066,1.56469508657096,47.2283406411677));
#20942=CARTESIAN_POINT('Ctrl Pts',(-6.62314407831425,1.39838254315073,47.2363535577872));
#20943=CARTESIAN_POINT('Ctrl Pts',(-6.65634397652307,1.23065782574296,47.2443664744068));
#20944=CARTESIAN_POINT('Ctrl Pts',(-6.68313760284297,1.0620549804348,47.2523793910263));
#20945=CARTESIAN_POINT('Ctrl Pts',(-6.71109309146522,0.886140945230387,
47.2607397748249));
#20946=CARTESIAN_POINT('Ctrl Pts',(-6.73207423179778,0.709271383199012,
47.2691001586234));
#20947=CARTESIAN_POINT('Ctrl Pts',(-6.74605103415646,0.532056805760918,
47.2774605424219));
#20948=CARTESIAN_POINT('Ctrl Pts',(-6.76002783651515,0.35484222832276,47.2858209262205));
#20949=CARTESIAN_POINT('Ctrl Pts',(-6.76700033878351,0.177283097596419,
47.294181310019));
#20950=CARTESIAN_POINT('Ctrl Pts',(-6.76699999998765,-1.29310941174092E-5,
47.3025416938175));
#20951=CARTESIAN_POINT('Ctrl Pts',(-6.767,1.57869394139717E-12,47.3028202161899));
#20952=CARTESIAN_POINT('Ctrl Pts',(-6.76700000000004,-0.186007249414218,
47.3115697279959));
#20953=CARTESIAN_POINT('Ctrl Pts',(-6.75932637295446,-0.372014355526194,
47.3203192398018));
#20954=CARTESIAN_POINT('Ctrl Pts',(-6.74400518266938,-0.557389537153829,
47.3290687516078));
#20955=CARTESIAN_POINT('Ctrl Pts',(-6.72868405709658,-0.742763935810309,
47.3378182264583));
#20956=CARTESIAN_POINT('Ctrl Pts',(-6.70571545653005,-0.927506129694079,
47.3465677013089));
#20957=CARTESIAN_POINT('Ctrl Pts',(-6.67517739415664,-1.11098863924893,
47.3553171761594));
#20958=CARTESIAN_POINT('Ctrl Pts',(-6.64463945823081,-1.294470389066,47.3640666147814));
#20959=CARTESIAN_POINT('Ctrl Pts',(-6.60653217027132,-1.47669218228331,
47.3728160534034));
#20960=CARTESIAN_POINT('Ctrl Pts',(-6.56098496116679,-1.65703510504251,
47.3815654920254));
#20961=CARTESIAN_POINT('Ctrl Pts',(-6.51543793687479,-1.83737729604157,
47.3903148951456));
#20962=CARTESIAN_POINT('Ctrl Pts',(-6.46245112202595,-2.01584035397196,
47.3990642982659));
#20963=CARTESIAN_POINT('Ctrl Pts',(-6.40220448416191,-2.19181813638292,
47.4078137013861));
#20964=CARTESIAN_POINT('Ctrl Pts',(-6.34195808575127,-2.36779521936104,
47.4165630697314));
#20965=CARTESIAN_POINT('Ctrl Pts',(-6.27445201489166,-2.54128677544999,
47.4253124380766));
#20966=CARTESIAN_POINT('Ctrl Pts',(-6.19991555136104,-2.71170355238023,
47.4340618064219));
#20967=CARTESIAN_POINT('Ctrl Pts',(-6.12537937788949,-2.88211966613263,
47.442811140719));
#20968=CARTESIAN_POINT('Ctrl Pts',(-6.04381298133517,-3.04946076210644,
47.451560475016));
#20969=CARTESIAN_POINT('Ctrl Pts',(-5.95549339426195,-3.21315848207062,
47.4603098093131));
#20970=CARTESIAN_POINT('Ctrl Pts',(-5.86717414355043,-3.37685557859841,
47.4690591102887));
#20971=CARTESIAN_POINT('Ctrl Pts',(-5.77210188986114,-3.53690907467513,
47.4778084112642));
#20972=CARTESIAN_POINT('Ctrl Pts',(-5.67059953466938,-3.69277536785104,
47.4865577122398));
#20973=CARTESIAN_POINT('Ctrl Pts',(-5.56909755761628,-3.84864108035993,
47.4953069806206));
#20974=CARTESIAN_POINT('Ctrl Pts',(-5.46116568337924,-4.00031938104479,
47.5040562490013));
#20975=CARTESIAN_POINT('Ctrl Pts',(-5.3471704868596,-4.14729511663418,47.5128055173821));
#20976=CARTESIAN_POINT('Ctrl Pts',(-5.23317570555375,-4.29427031688213,
47.5215547538947));
#20977=CARTESIAN_POINT('Ctrl Pts',(-5.11311782178677,-4.43654275987276,
47.5303039904073));
#20978=CARTESIAN_POINT('Ctrl Pts',(-4.98740459171902,-4.57362924147772,
47.5390532269199));
#20979=CARTESIAN_POINT('Ctrl Pts',(-4.86169180910708,-4.71071523514563,
47.547802432291));
#20980=CARTESIAN_POINT('Ctrl Pts',(-4.73032391415299,-4.84261509316654,
47.5565516376621));
#20981=CARTESIAN_POINT('Ctrl Pts',(-4.5937470723715,-4.96888084331656,47.5653008430333));
#20982=CARTESIAN_POINT('Ctrl Pts',(-4.45717070537264,-5.09514615452845,
47.5740500179895));
#20983=CARTESIAN_POINT('Ctrl Pts',(-4.31538563819377,-5.21577720253742,
47.5827991929457));
#20984=CARTESIAN_POINT('Ctrl Pts',(-4.16887341290522,-5.33036429028748,
47.5915483679019));
#20985=CARTESIAN_POINT('Ctrl Pts',(-4.02236168477222,-5.44495098921262,
47.6002975131699));
#20986=CARTESIAN_POINT('Ctrl Pts',(-3.87112305634334,-5.55349359238832,
47.6090466584378));
#20987=CARTESIAN_POINT('Ctrl Pts',(-3.71567117316639,-5.65562346102535,
47.6177958037057));
#20988=CARTESIAN_POINT('Ctrl Pts',(-3.56021980457248,-5.757752991588,47.6265449200118));
#20989=CARTESIAN_POINT('Ctrl Pts',(-3.40055544862379,-5.85346967275357,
47.635294036318));
#20990=CARTESIAN_POINT('Ctrl Pts',(-3.2372203632344,-5.94244842803541,47.6440431526241));
#20991=CARTESIAN_POINT('Ctrl Pts',(-3.07388580496105,-6.03142689616445,
47.652792240695));
#20992=CARTESIAN_POINT('Ctrl Pts',(-2.90688079257788,-6.11366734484783,
47.661541328766));
#20993=CARTESIAN_POINT('Ctrl Pts',(-2.73677251094719,-6.18889046787256,
47.6702904168369));
#20994=CARTESIAN_POINT('Ctrl Pts',(-2.56666476416749,-6.26411335438228,
47.6790394773991));
#20995=CARTESIAN_POINT('Ctrl Pts',(-2.39345402972197,-6.33231884350251,
47.6877885379614));
#20996=CARTESIAN_POINT('Ctrl Pts',(-2.21772856474142,-6.39327529621007,
47.6965375985236));
#20997=CARTESIAN_POINT('Ctrl Pts',(-2.04200363768377,-6.45423156232048,
47.7052866323036));
#20998=CARTESIAN_POINT('Ctrl Pts',(-1.86376426620204,-6.50793874252024,
47.7140356660836));
#20999=CARTESIAN_POINT('Ctrl Pts',(-1.68361578194803,-6.55421443796093,
47.7227846998636));
#21000=CARTESIAN_POINT('Ctrl Pts',(-1.50346783419996,-6.6004899955865,47.7315337075878));
#21001=CARTESIAN_POINT('Ctrl Pts',(-1.32141106257388,-6.63933404145467,
47.740282715312));
#21002=CARTESIAN_POINT('Ctrl Pts',(-1.13806375959199,-6.67061465527003,
47.7490317230363));
#21003=CARTESIAN_POINT('Ctrl Pts',(-0.954716987420964,-6.70189517852454,
47.7577807054311));
#21004=CARTESIAN_POINT('Ctrl Pts',(-0.770079973811953,-6.72561226535803,
47.766529687826));
#21005=CARTESIAN_POINT('Ctrl Pts',(-0.584779770554797,-6.74168536939762,
47.7752786702209));
#21006=CARTESIAN_POINT('Ctrl Pts',(-0.391490647556247,-6.7584514394238,
47.7844048508969));
#21007=CARTESIAN_POINT('Ctrl Pts',(-0.197480213106664,-6.7668997592402,
47.793531031573));
#21008=CARTESIAN_POINT('Ctrl Pts',(-0.00346532630011522,-6.76699911271707,
47.802657212249));
#21009=CARTESIAN_POINT('Ctrl Pts',(0.184486595293761,-6.7670953613978,47.811498199779));
#21010=CARTESIAN_POINT('Ctrl Pts',(0.372442378182964,-6.75935659726783,
47.8203391873089));
#21011=CARTESIAN_POINT('Ctrl Pts',(0.559750217719851,-6.74380965729035,
47.8291801748388));
#21012=CARTESIAN_POINT('Ctrl Pts',(0.745129914455523,-6.72842275717278,
47.8379301534366));
#21013=CARTESIAN_POINT('Ctrl Pts',(0.92987465631196,-6.70538772273504,47.8466801320344));
#21014=CARTESIAN_POINT('Ctrl Pts',(1.11335688289556,-6.67478280180779,47.8554301106321));
#21015=CARTESIAN_POINT('Ctrl Pts',(1.29683723118635,-6.64417819418067,47.8641799996571));
#21016=CARTESIAN_POINT('Ctrl Pts',(1.47905480730015,-6.60600390230124,47.872929888682));
#21017=CARTESIAN_POINT('Ctrl Pts',(1.65939064804589,-6.5603895979719,47.8816797777069));
#21018=CARTESIAN_POINT('Ctrl Pts',(1.8397247026404,-6.51477574543319,47.8904295800679));
#21019=CARTESIAN_POINT('Ctrl Pts',(2.01817678125617,-6.46172209820172,47.8991793824288));
#21020=CARTESIAN_POINT('Ctrl Pts',(2.19414072347444,-6.40140886724095,47.9079291847898));
#21021=CARTESIAN_POINT('Ctrl Pts',(2.37010298131865,-6.34109621361461,47.9166789033953));
#21022=CARTESIAN_POINT('Ctrl Pts',(2.54357687926684,-6.27352420826064,47.9254286220008));
#21023=CARTESIAN_POINT('Ctrl Pts',(2.71397317789746,-6.19892237325595,47.9341783406062));
#21024=CARTESIAN_POINT('Ctrl Pts',(2.88436790206983,-6.12432122757066,47.9429279783645));
#21025=CARTESIAN_POINT('Ctrl Pts',(3.05168482126046,-6.04269049717523,47.9516776161228));
#21026=CARTESIAN_POINT('Ctrl Pts',(3.21535561997186,-5.95430745235039,47.9604272538811));
#21027=CARTESIAN_POINT('Ctrl Pts',(3.37902496075074,-5.86592519481635,47.9691768137001));
#21028=CARTESIAN_POINT('Ctrl Pts',(3.53904799384665,-5.7707908794036,47.9779263735191));
#21029=CARTESIAN_POINT('Ctrl Pts',(3.69488118814772,-5.66922763747163,47.9866759333381));
#21030=CARTESIAN_POINT('Ctrl Pts',(3.85071304610632,-5.56766526649191,47.9954254181255));
#21031=CARTESIAN_POINT('Ctrl Pts',(4.00235489705778,-5.45967423580853,48.004174902913));
#21032=CARTESIAN_POINT('Ctrl Pts',(4.14929168607474,-5.34562133936468,48.0129243877004));
#21033=CARTESIAN_POINT('Ctrl Pts',(4.29622726385572,-5.23156938308683,48.0216738003637));
#21034=CARTESIAN_POINT('Ctrl Pts',(4.43845763091876,-5.11145583677367,48.030423213027));
#21035=CARTESIAN_POINT('Ctrl Pts',(4.57549970660767,-4.9856886620439,48.0391726256903));
#21036=CARTESIAN_POINT('Ctrl Pts',(4.71254069815098,-4.85992248226352,48.0479219691366));
#21037=CARTESIAN_POINT('Ctrl Pts',(4.84439326931116,-4.72850295734205,48.0566713125829));
#21038=CARTESIAN_POINT('Ctrl Pts',(4.970609594345,-4.59187644221896,48.0654206560293));
#21039=CARTESIAN_POINT('Ctrl Pts',(5.09682496280332,-4.45525096256874,48.0741699331656));
#21040=CARTESIAN_POINT('Ctrl Pts',(5.2174039761567,-4.31341878218531,48.0829192103019));
#21041=CARTESIAN_POINT('Ctrl Pts',(5.33193710451779,-4.16686161438876,48.0916684874381));
#21042=CARTESIAN_POINT('Ctrl Pts',(5.4464694028923,-4.02030550864721,48.1004177011711));
#21043=CARTESIAN_POINT('Ctrl Pts',(5.55495572749514,-3.8690247098035,48.1091669149041));
#21044=CARTESIAN_POINT('Ctrl Pts',(5.65702762491308,-3.71353301466007,48.117916128637));
#21045=CARTESIAN_POINT('Ctrl Pts',(5.7590988165501,-3.55804239467125,48.1266652818732));
#21046=CARTESIAN_POINT('Ctrl Pts',(5.85475551250643,-3.39834117619792,48.1354144351093));
#21047=CARTESIAN_POINT('Ctrl Pts',(5.94367283727961,-3.23497174692215,48.1441635883454));
#21048=CARTESIAN_POINT('Ctrl Pts',(6.0325895767618,-3.07160339301223,48.1529126839909));
#21049=CARTESIAN_POINT('Ctrl Pts',(6.11476689685156,-2.90456712829773,48.1616617796364));
#21050=CARTESIAN_POINT('Ctrl Pts',(6.18992570525137,-2.73443024476185,48.170410875282));
#21051=CARTESIAN_POINT('Ctrl Pts',(6.26508404388581,-2.56429442463313,48.179159916243));
#21052=CARTESIAN_POINT('Ctrl Pts',(6.33322384283207,-2.39105828656279,48.187908957204));
#21053=CARTESIAN_POINT('Ctrl Pts',(6.39411368719933,-2.2153101713237,48.196657998165));
#21054=CARTESIAN_POINT('Ctrl Pts',(6.45500317120803,-2.03956309619792,48.2054069873475));
#21055=CARTESIAN_POINT('Ctrl Pts',(6.50864269269998,-1.86130434438897,48.2141559765299));
#21056=CARTESIAN_POINT('Ctrl Pts',(6.55485008446269,-1.68113930720195,48.2229049657123));
#21057=CARTESIAN_POINT('Ctrl Pts',(6.60199664749348,-1.49731239212087,48.2318317792417));
#21058=CARTESIAN_POINT('Ctrl Pts',(6.64140563640859,-1.31150116499914,48.240758592771));
#21059=CARTESIAN_POINT('Ctrl Pts',(6.67293772282132,-1.12436255155899,48.2496854063004));
#21060=CARTESIAN_POINT('Ctrl Pts',(6.70384494949837,-0.940932395053742,
48.2584353204559));
#21061=CARTESIAN_POINT('Ctrl Pts',(6.72718449348903,-0.756227260509118,
48.2671852346114));
#21062=CARTESIAN_POINT('Ctrl Pts',(6.74287707373912,-0.570874564544097,
48.275935148767));
#21063=CARTESIAN_POINT('Ctrl Pts',(6.75856934538656,-0.385525513634903,
48.284684890851));
#21064=CARTESIAN_POINT('Ctrl Pts',(6.76661493004096,-0.199529212420676,
48.2934346329349));
#21065=CARTESIAN_POINT('Ctrl Pts',(6.76698649908906,-0.0135174386028909,
48.3021843750189));
#21066=CARTESIAN_POINT('Ctrl Pts',(6.76735806132396,0.172490924443328,48.3109339566648));
#21067=CARTESIAN_POINT('Ctrl Pts',(6.76005588896302,0.358514472898973,48.3196835383107));
#21068=CARTESIAN_POINT('Ctrl Pts',(6.74510478454604,0.543921359659797,48.3284331199566));
#21069=CARTESIAN_POINT('Ctrl Pts',(6.73015393440714,0.729325093148028,48.3371825527956));
#21070=CARTESIAN_POINT('Ctrl Pts',(6.7075544355693,0.914111900253936,48.3459319856347));
#21071=CARTESIAN_POINT('Ctrl Pts',(6.67738304682358,1.09765415591297,48.3546814184737));
#21072=CARTESIAN_POINT('Ctrl Pts',(6.64721213111906,1.28119353391034,48.3634307141351));
#21073=CARTESIAN_POINT('Ctrl Pts',(6.60946960955546,1.46348811672417,48.3721800097964));
#21074=CARTESIAN_POINT('Ctrl Pts',(6.56428366991241,1.64391876347989,48.3809293054577));
#21075=CARTESIAN_POINT('Ctrl Pts',(6.51909837867783,1.82434682109482,48.3896784755685));
#21076=CARTESIAN_POINT('Ctrl Pts',(6.46646995271994,2.00291071820211,48.3984276456794));
#21077=CARTESIAN_POINT('Ctrl Pts',(6.40657713281629,2.17900400212469,48.4071768157902));
#21078=CARTESIAN_POINT('Ctrl Pts',(6.34668509279148,2.35509499309419,48.415925871976));
#21079=CARTESIAN_POINT('Ctrl Pts',(6.27952894037623,2.52871516397879,48.4246749281617));
#21080=CARTESIAN_POINT('Ctrl Pts',(6.20533675061554,2.69927486771173,48.4334239843475));
#21081=CARTESIAN_POINT('Ctrl Pts',(6.12832117908028,2.87632521635686,48.4425059856298));
#21082=CARTESIAN_POINT('Ctrl Pts',(6.04372366626194,3.05007728919771,48.4515879869121));
#21083=CARTESIAN_POINT('Ctrl Pts',(5.95185378007985,3.21989527477979,48.4606699881943));
#21084=CARTESIAN_POINT('Ctrl Pts',(5.86334450817496,3.38350129286534,48.4694197685014));
#21085=CARTESIAN_POINT('Ctrl Pts',(5.76808562057389,3.54345567124744,48.4781695488086));
#21086=CARTESIAN_POINT('Ctrl Pts',(5.66640068804626,3.69921508465091,48.4869193291157));
#21087=CARTESIAN_POINT('Ctrl Pts',(5.56471941108072,3.85496889852069,48.4956687948692));
#21088=CARTESIAN_POINT('Ctrl Pts',(5.45661270815268,4.00652780919426,48.5044182606226));
#21089=CARTESIAN_POINT('Ctrl Pts',(5.34244776449275,4.15337704569023,48.5131677263761));
#21090=CARTESIAN_POINT('Ctrl Pts',(5.22828631819766,4.30022178356042,48.5219169240957));
#21091=CARTESIAN_POINT('Ctrl Pts',(5.10806717844251,4.4423569097247,48.5306661218153));
#21092=CARTESIAN_POINT('Ctrl Pts',(4.98219864544912,4.57929969070436,48.5394153195349));
#21093=CARTESIAN_POINT('Ctrl Pts',(4.85633329944224,4.71623900429795,48.5481642957252));
#21094=CARTESIAN_POINT('Ctrl Pts',(4.72481904033855,4.84798602483416,48.5569132719154));
#21095=CARTESIAN_POINT('Ctrl Pts',(4.58810250737412,4.97409332258929,48.5656622481056));
#21096=CARTESIAN_POINT('Ctrl Pts',(4.45137708685855,5.1002088182195,48.5744117930418));
#21097=CARTESIAN_POINT('Ctrl Pts',(4.30944892636264,5.22068366307758,48.583161337978));
#21098=CARTESIAN_POINT('Ctrl Pts',(4.16280009466872,5.33510865604686,48.5919108829142));
#21099=CARTESIAN_POINT('Ctrl Pts',(4.01615988349011,5.44952692272727,48.6006599135224));
#21100=CARTESIAN_POINT('Ctrl Pts',(3.86479978232465,5.55789587288463,48.6094089441307));
#21101=CARTESIAN_POINT('Ctrl Pts',(3.70923383581313,5.65984746713717,48.618157974739));
#21102=CARTESIAN_POINT('Ctrl Pts',(3.55366577799788,5.7618004450523,48.626907124087));
#21103=CARTESIAN_POINT('Ctrl Pts',(3.39389200027089,5.85733573570915,48.635656273435));
#21104=CARTESIAN_POINT('Ctrl Pts',(3.23045513626291,5.94612887621792,48.6444054227831));
#21105=CARTESIAN_POINT('Ctrl Pts',(3.18695122151745,5.969763992066,48.6467342868961));
#21106=CARTESIAN_POINT('Ctrl Pts',(3.14318791262746,5.99292165435291,48.6490631510091));
#21107=CARTESIAN_POINT('Ctrl Pts',(3.09917575053254,6.01559628526641,48.6513920151221));
#21108=CARTESIAN_POINT('Origin',(0.,0.,-3.69717978381041));
#21109=CARTESIAN_POINT('',(3.0991757505326,6.01559628526638,51.0457515827422));
#21110=CARTESIAN_POINT('',(3.09917575053255,6.01559628526641,50.6515095859174));
#21111=CARTESIAN_POINT('',(3.09917575053259,6.01559628526639,-3.69717978381041));
#21112=CARTESIAN_POINT('',(-6.767,6.11874741909821E-10,49.6971797837813));
#21113=CARTESIAN_POINT('Ctrl Pts',(-6.767,1.9002451714841E-12,49.69717978381));
#21114=CARTESIAN_POINT('Ctrl Pts',(-6.76700000000005,-0.186007249413768,
49.705929295616));
#21115=CARTESIAN_POINT('Ctrl Pts',(-6.75932637295449,-0.372014355525611,
49.7146788074219));
#21116=CARTESIAN_POINT('Ctrl Pts',(-6.74400518266944,-0.55738953715312,
49.7234283192279));
#21117=CARTESIAN_POINT('Ctrl Pts',(-6.72868405709666,-0.7427639358096,49.7321777940784));
#21118=CARTESIAN_POINT('Ctrl Pts',(-6.70571545653015,-0.927506129693374,
49.7409272689289));
#21119=CARTESIAN_POINT('Ctrl Pts',(-6.67517739415676,-1.11098863924823,
49.7496767437795));
#21120=CARTESIAN_POINT('Ctrl Pts',(-6.64463945823095,-1.2944703890653,49.7584261824015));
#21121=CARTESIAN_POINT('Ctrl Pts',(-6.60653217027148,-1.47669218228261,
49.7671756210235));
#21122=CARTESIAN_POINT('Ctrl Pts',(-6.56098496116696,-1.65703510504182,
49.7759250596455));
#21123=CARTESIAN_POINT('Ctrl Pts',(-6.515437936875,-1.83737729604082,49.7846744627657));
#21124=CARTESIAN_POINT('Ctrl Pts',(-6.4624511220262,-2.01584035397116,49.7934238658859));
#21125=CARTESIAN_POINT('Ctrl Pts',(-6.40220448416221,-2.19181813638206,
49.8021732690062));
#21126=CARTESIAN_POINT('Ctrl Pts',(-6.34195808575155,-2.36779521936031,
49.8109226373514));
#21127=CARTESIAN_POINT('Ctrl Pts',(-6.2744520148919,-2.54128677544938,49.8196720056967));
#21128=CARTESIAN_POINT('Ctrl Pts',(-6.19991555136125,-2.71170355237975,
49.828421374042));
#21129=CARTESIAN_POINT('Ctrl Pts',(-6.12537937788979,-2.88211966613198,
49.8371707083391));
#21130=CARTESIAN_POINT('Ctrl Pts',(-6.04381298133557,-3.04946076210563,
49.8459200426361));
#21131=CARTESIAN_POINT('Ctrl Pts',(-5.95549339426247,-3.21315848206964,
49.8546693769332));
#21132=CARTESIAN_POINT('Ctrl Pts',(-5.86717414355095,-3.3768555785975,49.8634186779087));
#21133=CARTESIAN_POINT('Ctrl Pts',(-5.77210188986166,-3.5369090746743,49.8721679788843));
#21134=CARTESIAN_POINT('Ctrl Pts',(-5.67059953466988,-3.69277536785027,
49.8809172798599));
#21135=CARTESIAN_POINT('Ctrl Pts',(-5.56909755761694,-3.84864108035896,
49.8896665482406));
#21136=CARTESIAN_POINT('Ctrl Pts',(-5.46116568338008,-4.00031938104363,
49.8984158166214));
#21137=CARTESIAN_POINT('Ctrl Pts',(-5.34717048686063,-4.14729511663284,
49.9071650850021));
#21138=CARTESIAN_POINT('Ctrl Pts',(-5.23317570555455,-4.29427031688118,
49.9159143215148));
#21139=CARTESIAN_POINT('Ctrl Pts',(-5.1131178217873,-4.43654275987217,49.9246635580274));
#21140=CARTESIAN_POINT('Ctrl Pts',(-4.98740459171925,-4.57362924147747,
49.93341279454));
#21141=CARTESIAN_POINT('Ctrl Pts',(-4.86169180910732,-4.71071523514538,
49.9421619999111));
#21142=CARTESIAN_POINT('Ctrl Pts',(-4.73032391415324,-4.84261509316629,
49.9509112052823));
#21143=CARTESIAN_POINT('Ctrl Pts',(-4.59374707237176,-4.96888084331632,
49.9596604106534));
#21144=CARTESIAN_POINT('Ctrl Pts',(-4.4571707053729,-5.09514615452822,49.9684095856096));
#21145=CARTESIAN_POINT('Ctrl Pts',(-4.31538563819403,-5.2157772025372,49.9771587605658));
#21146=CARTESIAN_POINT('Ctrl Pts',(-4.1688734129055,-5.33036429028727,49.985907935522));
#21147=CARTESIAN_POINT('Ctrl Pts',(-4.02236168477225,-5.44495098921261,
49.99465708079));
#21148=CARTESIAN_POINT('Ctrl Pts',(-3.8711230563431,-5.55349359238849,50.0034062260579));
#21149=CARTESIAN_POINT('Ctrl Pts',(-3.71567117316588,-5.65562346102568,
50.0121553713258));
#21150=CARTESIAN_POINT('Ctrl Pts',(-3.56021980457148,-5.75775299158864,
50.020904487632));
#21151=CARTESIAN_POINT('Ctrl Pts',(-3.40055544862227,-5.85346967275447,
50.0296536039382));
#21152=CARTESIAN_POINT('Ctrl Pts',(-3.23722036323235,-5.94244842803653,
50.0384027202443));
#21153=CARTESIAN_POINT('Ctrl Pts',(-3.07388580495869,-6.03142689616566,
50.0471518083153));
#21154=CARTESIAN_POINT('Ctrl Pts',(-2.9068807925752,-6.11366734484912,50.0559008963862));
#21155=CARTESIAN_POINT('Ctrl Pts',(-2.73677251094418,-6.18889046787389,
50.0646499844572));
#21156=CARTESIAN_POINT('Ctrl Pts',(-2.56666476416444,-6.26411335438353,
50.0733990450194));
#21157=CARTESIAN_POINT('Ctrl Pts',(-2.39345402971889,-6.33231884350368,
50.0821481055816));
#21158=CARTESIAN_POINT('Ctrl Pts',(-2.21772856473831,-6.39327529621115,
50.0908971661439));
#21159=CARTESIAN_POINT('Ctrl Pts',(-2.04200363768051,-6.45423156232151,
50.0996461999239));
#21160=CARTESIAN_POINT('Ctrl Pts',(-1.86376426619863,-6.50793874252122,
50.1083952337039));
#21161=CARTESIAN_POINT('Ctrl Pts',(-1.68361578194447,-6.55421443796185,
50.1171442674839));
#21162=CARTESIAN_POINT('Ctrl Pts',(-1.50346783419613,-6.60048999558738,
50.1258932752081));
#21163=CARTESIAN_POINT('Ctrl Pts',(-1.32141106256977,-6.63933404145549,
50.1346422829323));
#21164=CARTESIAN_POINT('Ctrl Pts',(-1.13806375958761,-6.67061465527078,
50.1433912906566));
#21165=CARTESIAN_POINT('Ctrl Pts',(-0.954716987415931,-6.70189517852527,
50.1521402730515));
#21166=CARTESIAN_POINT('Ctrl Pts',(-0.770079973806263,-6.7256122653587,
50.1608892554464));
#21167=CARTESIAN_POINT('Ctrl Pts',(-0.584779770548455,-6.74168536939817,
50.1696382378413));
#21168=CARTESIAN_POINT('Ctrl Pts',(-0.391490647549954,-6.75845143942417,
50.1787644185173));
#21169=CARTESIAN_POINT('Ctrl Pts',(-0.197480213100428,-6.76689975924038,
50.1878905991934));
#21170=CARTESIAN_POINT('Ctrl Pts',(-0.00346532629394415,-6.76699911271708,
50.1970167798694));
#21171=CARTESIAN_POINT('Ctrl Pts',(0.184486595299868,-6.76709536139763,
50.2058577673994));
#21172=CARTESIAN_POINT('Ctrl Pts',(0.372442378188994,-6.75935659726749,
50.2146987549293));
#21173=CARTESIAN_POINT('Ctrl Pts',(0.559750217725802,-6.74380965728986,
50.2235397424592));
#21174=CARTESIAN_POINT('Ctrl Pts',(0.745129914461395,-6.72842275717213,
50.232289721057));
#21175=CARTESIAN_POINT('Ctrl Pts',(0.92987465631775,-6.70538772273423,50.2410396996547));
#21176=CARTESIAN_POINT('Ctrl Pts',(1.11335688290126,-6.67478280180684,50.2497896782525));
#21177=CARTESIAN_POINT('Ctrl Pts',(1.29683723119203,-6.64417819417956,50.2585395672775));
#21178=CARTESIAN_POINT('Ctrl Pts',(1.47905480730579,-6.60600390229998,50.2672894563024));
#21179=CARTESIAN_POINT('Ctrl Pts',(1.65939064805149,-6.56038959797048,50.2760393453273));
#21180=CARTESIAN_POINT('Ctrl Pts',(1.83972470264602,-6.51477574543161,50.2847891476883));
#21181=CARTESIAN_POINT('Ctrl Pts',(2.01817678126181,-6.46172209819996,50.2935389500492));
#21182=CARTESIAN_POINT('Ctrl Pts',(2.19414072348009,-6.40140886723902,50.3022887524102));
#21183=CARTESIAN_POINT('Ctrl Pts',(2.37010298132424,-6.34109621361252,50.3110384710157));
#21184=CARTESIAN_POINT('Ctrl Pts',(2.54357687927237,-6.27352420825839,50.3197881896212));
#21185=CARTESIAN_POINT('Ctrl Pts',(2.71397317790293,-6.19892237325356,50.3285379082266));
#21186=CARTESIAN_POINT('Ctrl Pts',(2.88436790207529,-6.12432122756809,50.3372875459849));
#21187=CARTESIAN_POINT('Ctrl Pts',(3.0516848212659,-6.04269049717249,50.3460371837432));
#21188=CARTESIAN_POINT('Ctrl Pts',(3.21535561997727,-5.95430745234747,50.3547868215015));
#21189=CARTESIAN_POINT('Ctrl Pts',(3.37902496075602,-5.86592519481331,50.3635363813205));
#21190=CARTESIAN_POINT('Ctrl Pts',(3.53904799385179,-5.77079087940045,50.3722859411395));
#21191=CARTESIAN_POINT('Ctrl Pts',(3.69488118815271,-5.66922763746837,50.3810355009585));
#21192=CARTESIAN_POINT('Ctrl Pts',(3.85071304611117,-5.56766526648856,50.3897849857459));
#21193=CARTESIAN_POINT('Ctrl Pts',(4.00235489706248,-5.45967423580509,50.3985344705334));
#21194=CARTESIAN_POINT('Ctrl Pts',(4.1492916860793,-5.34562133936114,50.4072839553208));
#21195=CARTESIAN_POINT('Ctrl Pts',(4.29622726386022,-5.23156938308313,50.4160333679841));
#21196=CARTESIAN_POINT('Ctrl Pts',(4.43845763092321,-5.11145583676981,50.4247827806474));
#21197=CARTESIAN_POINT('Ctrl Pts',(4.57549970661206,-4.98568866203988,50.4335321933107));
#21198=CARTESIAN_POINT('Ctrl Pts',(4.71254069815535,-4.85992248225929,50.442281536757));
#21199=CARTESIAN_POINT('Ctrl Pts',(4.8443932693155,-4.7285029573376,50.4510308802033));
#21200=CARTESIAN_POINT('Ctrl Pts',(4.9706095943493,-4.59187644221431,50.4597802236497));
#21201=CARTESIAN_POINT('Ctrl Pts',(5.09682496280745,-4.45525096256402,50.468529500786));
#21202=CARTESIAN_POINT('Ctrl Pts',(5.21740397616065,-4.31341878218052,50.4772787779223));
#21203=CARTESIAN_POINT('Ctrl Pts',(5.33193710452157,-4.16686161438392,50.4860280550586));
#21204=CARTESIAN_POINT('Ctrl Pts',(5.44646940289602,-4.02030550864217,50.4947772687915));
#21205=CARTESIAN_POINT('Ctrl Pts',(5.5549557274988,-3.86902470979825,50.5035264825245));
#21206=CARTESIAN_POINT('Ctrl Pts',(5.65702762491666,-3.71353301465461,50.5122756962575));
#21207=CARTESIAN_POINT('Ctrl Pts',(5.75909881655357,-3.55804239466565,50.5210248494936));
#21208=CARTESIAN_POINT('Ctrl Pts',(5.85475551250977,-3.39834117619217,50.5297740027297));
#21209=CARTESIAN_POINT('Ctrl Pts',(5.94367283728282,-3.23497174691626,50.5385231559658));
#21210=CARTESIAN_POINT('Ctrl Pts',(6.03258957676485,-3.07160339300625,50.5472722516113));
#21211=CARTESIAN_POINT('Ctrl Pts',(6.11476689685444,-2.90456712829166,50.5560213472569));
#21212=CARTESIAN_POINT('Ctrl Pts',(6.18992570525408,-2.73443024475571,50.5647704429024));
#21213=CARTESIAN_POINT('Ctrl Pts',(6.26508404388836,-2.56429442462692,50.5735194838634));
#21214=CARTESIAN_POINT('Ctrl Pts',(6.33322384283444,-2.39105828655651,50.5822685248245));
#21215=CARTESIAN_POINT('Ctrl Pts',(6.39411368720152,-2.21531017131736,50.5910175657855));
#21216=CARTESIAN_POINT('Ctrl Pts',(6.45500317121003,-2.03956309619158,50.5997665549679));
#21217=CARTESIAN_POINT('Ctrl Pts',(6.50864269270179,-1.86130434438265,50.6085155441503));
#21218=CARTESIAN_POINT('Ctrl Pts',(6.55485008446431,-1.68113930719564,50.6172645333327));
#21219=CARTESIAN_POINT('Ctrl Pts',(6.60199664749489,-1.49731239211464,50.6261913468621));
#21220=CARTESIAN_POINT('Ctrl Pts',(6.6414056364098,-1.311501164993,50.6351181603914));
#21221=CARTESIAN_POINT('Ctrl Pts',(6.67293772282234,-1.12436255155295,50.6440449739208));
#21222=CARTESIAN_POINT('Ctrl Pts',(6.70384494949923,-0.940932395047674,
50.6527948880763));
#21223=CARTESIAN_POINT('Ctrl Pts',(6.72718449348972,-0.756227260503029,
50.6615448022319));
#21224=CARTESIAN_POINT('Ctrl Pts',(6.74287707373963,-0.570874564537995,
50.6702947163874));
#21225=CARTESIAN_POINT('Ctrl Pts',(6.75856934538691,-0.385525513628787,
50.6790444584714));
#21226=CARTESIAN_POINT('Ctrl Pts',(6.76661493004114,-0.199529212414554,
50.6877942005553));
#21227=CARTESIAN_POINT('Ctrl Pts',(6.76698649908907,-0.0135174385967701,
50.6965439426393));
#21228=CARTESIAN_POINT('Ctrl Pts',(6.7673580613238,0.172490924449449,50.7052935242852));
#21229=CARTESIAN_POINT('Ctrl Pts',(6.7600558889627,0.358514472905087,50.7140431059311));
#21230=CARTESIAN_POINT('Ctrl Pts',(6.74510478454555,0.543921359665896,50.722792687577));
#21231=CARTESIAN_POINT('Ctrl Pts',(6.73015393440647,0.729325093154176,50.7315421204161));
#21232=CARTESIAN_POINT('Ctrl Pts',(6.70755443556846,0.914111900260126,50.7402915532551));
#21233=CARTESIAN_POINT('Ctrl Pts',(6.67738304682256,1.09765415591919,50.7490409860941));
#21234=CARTESIAN_POINT('Ctrl Pts',(6.64721213111787,1.28119353391654,50.7577902817555));
#21235=CARTESIAN_POINT('Ctrl Pts',(6.6094696095541,1.46348811673033,50.7665395774168));
#21236=CARTESIAN_POINT('Ctrl Pts',(6.56428366991088,1.64391876348601,50.7752888730781));
#21237=CARTESIAN_POINT('Ctrl Pts',(6.51909837867613,1.8243468211009,50.784038043189));
#21238=CARTESIAN_POINT('Ctrl Pts',(6.46646995271807,2.00291071820813,50.7927872132998));
#21239=CARTESIAN_POINT('Ctrl Pts',(6.40657713281426,2.17900400213066,50.8015363834106));
#21240=CARTESIAN_POINT('Ctrl Pts',(6.34668509278925,2.35509499310022,50.8102854395964));
#21241=CARTESIAN_POINT('Ctrl Pts',(6.27952894037379,2.52871516398488,50.8190344957822));
#21242=CARTESIAN_POINT('Ctrl Pts',(6.20533675061288,2.69927486771786,50.8277835519679));
#21243=CARTESIAN_POINT('Ctrl Pts',(6.12832117907754,2.87632521636268,50.8368655532502));
#21244=CARTESIAN_POINT('Ctrl Pts',(6.04372366625915,3.05007728920321,50.8459475545325));
#21245=CARTESIAN_POINT('Ctrl Pts',(5.95185378007704,3.21989527478499,50.8550295558147));
#21246=CARTESIAN_POINT('Ctrl Pts',(5.86334450817198,3.38350129287052,50.8637793361218));
#21247=CARTESIAN_POINT('Ctrl Pts',(5.76808562057073,3.54345567125259,50.872529116429));
#21248=CARTESIAN_POINT('Ctrl Pts',(5.66640068804293,3.69921508465602,50.8812788967361));
#21249=CARTESIAN_POINT('Ctrl Pts',(5.56471941107724,3.85496889852571,50.8900283624896));
#21250=CARTESIAN_POINT('Ctrl Pts',(5.45661270814907,4.00652780919919,50.8987778282431));
#21251=CARTESIAN_POINT('Ctrl Pts',(5.342447764489,4.15337704569505,50.9075272939965));
#21252=CARTESIAN_POINT('Ctrl Pts',(5.2282863181937,4.30022178356523,50.9162764917161));
#21253=CARTESIAN_POINT('Ctrl Pts',(5.10806717843834,4.4423569097295,50.9250256894357));
#21254=CARTESIAN_POINT('Ctrl Pts',(4.98219864544473,4.57929969070913,50.9337748871553));
#21255=CARTESIAN_POINT('Ctrl Pts',(4.85633329943768,4.71623900430265,50.9425238633456));
#21256=CARTESIAN_POINT('Ctrl Pts',(4.72481904033381,4.84798602483877,50.9512728395358));
#21257=CARTESIAN_POINT('Ctrl Pts',(4.58810250736921,4.97409332259381,50.9600218157261));
#21258=CARTESIAN_POINT('Ctrl Pts',(4.45137708685352,5.10020881822388,50.9687713606622));
#21259=CARTESIAN_POINT('Ctrl Pts',(4.30944892635749,5.22068366308183,50.9775209055984));
#21260=CARTESIAN_POINT('Ctrl Pts',(4.16280009466346,5.33510865605096,50.9862704505346));
#21261=CARTESIAN_POINT('Ctrl Pts',(4.01615988348459,5.44952692273135,50.9950194811429));
#21262=CARTESIAN_POINT('Ctrl Pts',(3.86479978231886,5.55789587288866,51.0037685117512));
#21263=CARTESIAN_POINT('Ctrl Pts',(3.70923383580707,5.65984746714114,51.0125175423594));
#21264=CARTESIAN_POINT('Ctrl Pts',(3.55366577799171,5.7618004450561,51.0212666917075));
#21265=CARTESIAN_POINT('Ctrl Pts',(3.39389200026462,5.85733573571278,51.0300158410555));
#21266=CARTESIAN_POINT('Ctrl Pts',(3.23045513625655,5.94612887622138,51.0387649904035));
#21267=CARTESIAN_POINT('Ctrl Pts',(3.1869512215132,5.96976399206825,51.0410938545164));
#21268=CARTESIAN_POINT('Ctrl Pts',(3.14318791262535,5.99292165435399,51.0434227186293));
#21269=CARTESIAN_POINT('Ctrl Pts',(3.0991757505326,6.01559628526638,51.0457515827422));
#21270=CARTESIAN_POINT('Ctrl Pts',(3.0991757505326,6.01559628526638,49.0457515827422));
#21271=CARTESIAN_POINT('Ctrl Pts',(2.93382384459263,6.1007839529376,49.0545010306546));
#21272=CARTESIAN_POINT('Ctrl Pts',(2.76495772122979,6.17915010267052,49.063250478567));
#21273=CARTESIAN_POINT('Ctrl Pts',(2.59315093316703,6.25042856433181,49.0719999264794));
#21274=CARTESIAN_POINT('Ctrl Pts',(2.42134553245604,6.32170645041456,49.0807493037394));
#21275=CARTESIAN_POINT('Ctrl Pts',(2.24659977927573,6.38589665313464,49.0894986809994));
#21276=CARTESIAN_POINT('Ctrl Pts',(2.06950718689896,6.44278115439082,49.0982480582595));
#21277=CARTESIAN_POINT('Ctrl Pts',(1.8924159657284,6.4996652151973,49.1069973677741));
#21278=CARTESIAN_POINT('Ctrl Pts',(1.71297821457178,6.54924360009551,49.1157466772888));
#21279=CARTESIAN_POINT('Ctrl Pts',(1.53180337335826,6.5913479217356,49.1244959868034));
#21280=CARTESIAN_POINT('Ctrl Pts',(1.3506298747776,6.63345193135309,49.1332452314795));
#21281=CARTESIAN_POINT('Ctrl Pts',(1.16771959102925,6.66808192368243,49.1419944761557));
#21282=CARTESIAN_POINT('Ctrl Pts',(0.983693746906534,6.69512028363173,49.1507437208318));
#21283=CARTESIAN_POINT('Ctrl Pts',(0.79966920541951,6.72215845218871,49.159492903576));
#21284=CARTESIAN_POINT('Ctrl Pts',(0.614529402873065,6.74160505424583,49.1682420863201));
#21285=CARTESIAN_POINT('Ctrl Pts',(0.428903127362787,6.75339404354125,49.1769912690643));
#21286=CARTESIAN_POINT('Ctrl Pts',(0.24327810416352,6.76518295330331,49.1857403927829));
#21287=CARTESIAN_POINT('Ctrl Pts',(0.0571669005388619,6.76931433552276,
49.1944895165015));
#21288=CARTESIAN_POINT('Ctrl Pts',(-0.128798404777666,6.76577415902473,
49.2032386402201));
#21289=CARTESIAN_POINT('Ctrl Pts',(-0.314762517259134,6.76223400523441,
49.2119877078193));
#21290=CARTESIAN_POINT('Ctrl Pts',(-0.50058044681943,6.75102239665089,49.2207367754186));
#21291=CARTESIAN_POINT('Ctrl Pts',(-0.685621118842415,6.732177410125,49.2294858430178));
#21292=CARTESIAN_POINT('Ctrl Pts',(-0.870660665414357,6.71333253821774,
49.2382348574035));
#21293=CARTESIAN_POINT('Ctrl Pts',(-1.0549226788548,6.68685441030613,49.2469838717893));
#21294=CARTESIAN_POINT('Ctrl Pts',(-1.23778137635252,6.65283295028177,49.2557328861751));
#21295=CARTESIAN_POINT('Ctrl Pts',(-1.42999922977601,6.61707018862097,49.2649296965419));
#21296=CARTESIAN_POINT('Ctrl Pts',(-1.62066601231224,6.57297172934985,49.2741265069087));
#21297=CARTESIAN_POINT('Ctrl Pts',(-1.80906628496722,6.5207030431231,49.2833233172755));
#21298=CARTESIAN_POINT('Ctrl Pts',(-1.98831342541891,6.47097374916148,49.2920733150132));
#21299=CARTESIAN_POINT('Ctrl Pts',(-2.16550875893095,6.41384933990746,49.300823312751));
#21300=CARTESIAN_POINT('Ctrl Pts',(-2.34005036710439,6.34952386241792,49.3095733104888));
#21301=CARTESIAN_POINT('Ctrl Pts',(-2.5145884354355,6.28519968950012,49.3183231307696));
#21302=CARTESIAN_POINT('Ctrl Pts',(-2.68647261714554,6.21367483972613,49.3270729510505));
#21303=CARTESIAN_POINT('Ctrl Pts',(-2.85511905905272,6.13519226745454,49.3358227713314));
#21304=CARTESIAN_POINT('Ctrl Pts',(-3.02376230485472,6.0567111825464,49.3445724257899));
#21305=CARTESIAN_POINT('Ctrl Pts',(-3.18916767376544,5.97127275994428,49.3533220802484));
#21306=CARTESIAN_POINT('Ctrl Pts',(-3.35077334099482,5.8791672043988,49.362071734707));
#21307=CARTESIAN_POINT('Ctrl Pts',(-3.51237616034115,5.78706327197617,49.3708212349754));
#21308=CARTESIAN_POINT('Ctrl Pts',(-3.67017916299103,5.68829258364361,49.3795707352439));
#21309=CARTESIAN_POINT('Ctrl Pts',(-3.82364636563326,5.5831906174319,49.3883202355123));
#21310=CARTESIAN_POINT('Ctrl Pts',(-3.9771110677573,5.47809036369929,49.3970695932207));
#21311=CARTESIAN_POINT('Ctrl Pts',(-4.12623987478931,5.36665920045529,49.4058189509292));
#21312=CARTESIAN_POINT('Ctrl Pts',(-4.27052628211007,5.24927559514712,49.4145683086376));
#21313=CARTESIAN_POINT('Ctrl Pts',(-4.41481053022136,5.13189374645482,49.4233175354141));
#21314=CARTESIAN_POINT('Ctrl Pts',(-4.5542523013377,5.00855981479864,49.4320667621907));
#21315=CARTESIAN_POINT('Ctrl Pts',(-4.68837800627872,4.87969268194648,49.4408159889672));
#21316=CARTESIAN_POINT('Ctrl Pts',(-4.82250188226293,4.75082730634451,49.449565096438));
#21317=CARTESIAN_POINT('Ctrl Pts',(-4.95130963050442,4.61642907906233,49.4583142039089));
#21318=CARTESIAN_POINT('Ctrl Pts',(-5.07436379030924,4.47695444734459,49.4670633113798));
#21319=CARTESIAN_POINT('Ctrl Pts',(-5.1974164356044,4.33748153223421,49.4758123111695));
#21320=CARTESIAN_POINT('Ctrl Pts',(-5.31471544460488,4.19293255257486,49.4845613109592));
#21321=CARTESIAN_POINT('Ctrl Pts',(-5.42586245273424,4.04379841782559,49.493310310749));
#21322=CARTESIAN_POINT('Ctrl Pts',(-5.53702160017027,3.89464799487365,49.5020602660911));
#21323=CARTESIAN_POINT('Ctrl Pts',(-5.64202723079206,3.74091164446935,49.5108102214333));
#21324=CARTESIAN_POINT('Ctrl Pts',(-5.74052265231004,3.58311159166377,49.5195601767754));
#21325=CARTESIAN_POINT('Ctrl Pts',(-5.8390142706505,3.42531763194968,49.5283097942579));
#21326=CARTESIAN_POINT('Ctrl Pts',(-5.93099603113968,3.26346052698834,49.5370594117404));
#21327=CARTESIAN_POINT('Ctrl Pts',(-6.01615550621079,3.0980900447033,49.5458090292228));
#21328=CARTESIAN_POINT('Ctrl Pts',(-6.10131214577217,2.9327250686712,49.5545583553739));
#21329=CARTESIAN_POINT('Ctrl Pts',(-6.1796468232726,2.76384720420222,49.563307681525));
#21330=CARTESIAN_POINT('Ctrl Pts',(-6.25089348287171,2.59203002794952,49.5720570076761));
#21331=CARTESIAN_POINT('Ctrl Pts',(-6.32213814888022,2.42021765940446,49.5808060890077));
#21332=CARTESIAN_POINT('Ctrl Pts',(-6.38629508411364,2.24546640835389,49.5895551703392));
#21333=CARTESIAN_POINT('Ctrl Pts',(-6.44314639818681,2.06836976663565,49.5983042516708));
#21334=CARTESIAN_POINT('Ctrl Pts',(-6.50000285282666,1.89125711161829,49.6070541241052));
#21335=CARTESIAN_POINT('Ctrl Pts',(-6.54955227672314,1.71179891443835,49.6158039965396));
#21336=CARTESIAN_POINT('Ctrl Pts',(-6.59162635925548,1.53060476282034,49.624553868974));
#21337=CARTESIAN_POINT('Ctrl Pts',(-6.63369752054463,1.34942319168304,49.6333031338965));
#21338=CARTESIAN_POINT('Ctrl Pts',(-6.66829431423623,1.16650618646313,49.642052398819));
#21339=CARTESIAN_POINT('Ctrl Pts',(-6.69529923744888,0.982474997654602,
49.6508016637415));
#21340=CARTESIAN_POINT('Ctrl Pts',(-6.72230554731013,0.798434359213978,
49.6595513779212));
#21341=CARTESIAN_POINT('Ctrl Pts',(-6.74171916496372,0.613279706276726,
49.6683010921009));
#21342=CARTESIAN_POINT('Ctrl Pts',(-6.75347414817044,0.427639953691877,
49.6770508062806));
#21343=CARTESIAN_POINT('Ctrl Pts',(-6.76248837757382,0.285283364425952,
49.6837604654475));
#21344=CARTESIAN_POINT('Ctrl Pts',(-6.76699999998711,0.142641701524115,
49.6904701246144));
#21345=CARTESIAN_POINT('Ctrl Pts',(-6.767,6.11779405774452E-10,49.6971797837813));
#21346=CARTESIAN_POINT('',(-6.76699999998378,1.48178903510378E-5,49.3031392543722));
#21347=CARTESIAN_POINT('Ctrl Pts',(3.09917575053254,6.01559628526641,48.6513920151221));
#21348=CARTESIAN_POINT('Ctrl Pts',(2.9338238445926,6.10078395293762,48.6601414630345));
#21349=CARTESIAN_POINT('Ctrl Pts',(2.76495772122978,6.17915010267052,48.6688909109469));
#21350=CARTESIAN_POINT('Ctrl Pts',(2.59315093316705,6.2504285643318,48.6776403588593));
#21351=CARTESIAN_POINT('Ctrl Pts',(2.42134553245609,6.32170645041454,48.6863897361193));
#21352=CARTESIAN_POINT('Ctrl Pts',(2.24659977927581,6.38589665313461,48.6951391133793));
#21353=CARTESIAN_POINT('Ctrl Pts',(2.06950718689908,6.44278115439079,48.7038884906393));
#21354=CARTESIAN_POINT('Ctrl Pts',(1.89241596572848,6.49966521519728,48.712637800154));
#21355=CARTESIAN_POINT('Ctrl Pts',(1.71297821457183,6.5492436000955,48.7213871096686));
#21356=CARTESIAN_POINT('Ctrl Pts',(1.53180337335827,6.5913479217356,48.7301364191833));
#21357=CARTESIAN_POINT('Ctrl Pts',(1.35062987477764,6.63345193135308,48.7388856638594));
#21358=CARTESIAN_POINT('Ctrl Pts',(1.16771959102932,6.66808192368241,48.7476349085356));
#21359=CARTESIAN_POINT('Ctrl Pts',(0.983693746906633,6.69512028363171,48.7563841532117));
#21360=CARTESIAN_POINT('Ctrl Pts',(0.799669205419703,6.72215845218869,48.7651333359559));
#21361=CARTESIAN_POINT('Ctrl Pts',(0.614529402873353,6.7416050542458,48.7738825187));
#21362=CARTESIAN_POINT('Ctrl Pts',(0.42890312736317,6.75339404354123,48.7826317014442));
#21363=CARTESIAN_POINT('Ctrl Pts',(0.243278104163996,6.76518295330329,48.7913808251628));
#21364=CARTESIAN_POINT('Ctrl Pts',(0.0571669005394296,6.76931433552275,
48.8001299488814));
#21365=CARTESIAN_POINT('Ctrl Pts',(-0.128798404777005,6.76577415902474,
48.8088790726));
#21366=CARTESIAN_POINT('Ctrl Pts',(-0.314762517258572,6.76223400523444,
48.8176281401992));
#21367=CARTESIAN_POINT('Ctrl Pts',(-0.500580446818966,6.75102239665093,
48.8263772077984));
#21368=CARTESIAN_POINT('Ctrl Pts',(-0.68562111884205,6.73217741012503,48.8351262753976));
#21369=CARTESIAN_POINT('Ctrl Pts',(-0.870660665413836,6.7133325382178,48.8438752897834));
#21370=CARTESIAN_POINT('Ctrl Pts',(-1.05492267885412,6.68685441030623,48.8526243041692));
#21371=CARTESIAN_POINT('Ctrl Pts',(-1.23778137635169,6.65283295028193,48.8613733185549));
#21372=CARTESIAN_POINT('Ctrl Pts',(-1.4299992297877,6.61707018861882,48.8705701289223));
#21373=CARTESIAN_POINT('Ctrl Pts',(-1.62066601233624,6.57297172934431,48.8797669392897));
#21374=CARTESIAN_POINT('Ctrl Pts',(-1.8090662850032,6.52070304311312,48.8889637496571));
#21375=CARTESIAN_POINT('Ctrl Pts',(-1.98831342545458,6.47097374915052,48.8977137473949));
#21376=CARTESIAN_POINT('Ctrl Pts',(-2.16550875896629,6.41384933989553,48.9064637451326));
#21377=CARTESIAN_POINT('Ctrl Pts',(-2.34005036713935,6.34952386240504,48.9152137428704));
#21378=CARTESIAN_POINT('Ctrl Pts',(-2.51458843547014,6.28519968948626,48.9239635631513));
#21379=CARTESIAN_POINT('Ctrl Pts',(-2.68647261717981,6.21367483971131,48.9327133834321));
#21380=CARTESIAN_POINT('Ctrl Pts',(-2.85511905908659,6.13519226743878,48.941463203713));
#21381=CARTESIAN_POINT('Ctrl Pts',(-3.02376230488808,6.05671118252975,48.9502128581715));
#21382=CARTESIAN_POINT('Ctrl Pts',(-3.18916767379824,5.97127275992676,48.9589625126301));
#21383=CARTESIAN_POINT('Ctrl Pts',(-3.35077334102703,5.87916720438044,48.9677121670886));
#21384=CARTESIAN_POINT('Ctrl Pts',(-3.51237616037283,5.78706327195694,48.9764616673571));
#21385=CARTESIAN_POINT('Ctrl Pts',(-3.67017916302215,5.68829258362353,48.9852111676255));
#21386=CARTESIAN_POINT('Ctrl Pts',(-3.82364636566377,5.583190617411,48.9939606678939));
#21387=CARTESIAN_POINT('Ctrl Pts',(-3.97711106778711,5.47809036367765,49.0027100256024));
#21388=CARTESIAN_POINT('Ctrl Pts',(-4.12623987481839,5.36665920043293,49.0114593833108));
#21389=CARTESIAN_POINT('Ctrl Pts',(-4.2705262821384,5.24927559512408,49.0202087410192));
#21390=CARTESIAN_POINT('Ctrl Pts',(-4.41481053024908,5.13189374643098,49.0289579677958));
#21391=CARTESIAN_POINT('Ctrl Pts',(-4.55425230136478,5.00855981477402,49.0377071945723));
#21392=CARTESIAN_POINT('Ctrl Pts',(-4.68837800630512,4.87969268192111,49.0464564213488));
#21393=CARTESIAN_POINT('Ctrl Pts',(-4.82250188228871,4.75082730631834,49.0552055288197));
#21394=CARTESIAN_POINT('Ctrl Pts',(-4.95130963052954,4.61642907903539,49.0639546362905));
#21395=CARTESIAN_POINT('Ctrl Pts',(-5.07436379033366,4.47695444731691,49.0727037437614));
#21396=CARTESIAN_POINT('Ctrl Pts',(-5.19741643562795,4.33748153220598,49.0814527435511));
#21397=CARTESIAN_POINT('Ctrl Pts',(-5.31471544462755,4.19293255254612,49.0902017433408));
#21398=CARTESIAN_POINT('Ctrl Pts',(-5.42586245275602,4.04379841779637,49.0989507431306));
#21399=CARTESIAN_POINT('Ctrl Pts',(-5.53702160019123,3.89464799484385,49.1077006984727));
#21400=CARTESIAN_POINT('Ctrl Pts',(-5.64202723081217,3.74091164443901,49.1164506538149));
#21401=CARTESIAN_POINT('Ctrl Pts',(-5.74052265232929,3.58311159163293,49.125200609157));
#21402=CARTESIAN_POINT('Ctrl Pts',(-5.83901427066885,3.42531763191839,49.1339502266395));
#21403=CARTESIAN_POINT('Ctrl Pts',(-5.93099603115712,3.26346052695664,49.1426998441219));
#21404=CARTESIAN_POINT('Ctrl Pts',(-6.0161555062273,3.09809004467122,49.1514494616044));
#21405=CARTESIAN_POINT('Ctrl Pts',(-6.10131214578779,2.9327250686387,49.1601987877555));
#21406=CARTESIAN_POINT('Ctrl Pts',(-6.17964682328731,2.76384720416932,49.1689481139066));
#21407=CARTESIAN_POINT('Ctrl Pts',(-6.2508934828855,2.59203002791627,49.1776974400577));
#21408=CARTESIAN_POINT('Ctrl Pts',(-6.3221381488933,2.42021765937033,49.1864465213893));
#21409=CARTESIAN_POINT('Ctrl Pts',(-6.38629508412596,2.24546640831891,49.1951956027209));
#21410=CARTESIAN_POINT('Ctrl Pts',(-6.44314639819831,2.06836976659982,49.2039446840524));
#21411=CARTESIAN_POINT('Ctrl Pts',(-6.50000285283717,1.89125711158218,49.2126945564868));
#21412=CARTESIAN_POINT('Ctrl Pts',(-6.54955227673264,1.71179891440199,49.2214444289212));
#21413=CARTESIAN_POINT('Ctrl Pts',(-6.59162635926397,1.53060476278377,49.2301943013556));
#21414=CARTESIAN_POINT('Ctrl Pts',(-6.6336975205521,1.34942319164633,49.2389435662781));
#21415=CARTESIAN_POINT('Ctrl Pts',(-6.66829431424267,1.16650618642632,49.2476928312006));
#21416=CARTESIAN_POINT('Ctrl Pts',(-6.69529923745429,0.982474997617739,
49.2564420961231));
#21417=CARTESIAN_POINT('Ctrl Pts',(-6.72230554731453,0.798434359176932,
49.2651918103028));
#21418=CARTESIAN_POINT('Ctrl Pts',(-6.7417191649671,0.61327970623954,49.2739415244825));
#21419=CARTESIAN_POINT('Ctrl Pts',(-6.7534741481728,0.427639953654592,49.2826912386622));
#21420=CARTESIAN_POINT('Ctrl Pts',(-6.76248837758746,0.285283364198101,
49.2894008978381));
#21421=CARTESIAN_POINT('Ctrl Pts',(-6.76699999999996,0.14264170110496,49.296110557014));
#21422=CARTESIAN_POINT('Ctrl Pts',(-6.767,1.72760381084485E-12,49.3028202161899));
#21423=CARTESIAN_POINT('Ctrl Pts',(-6.76699999998378,1.48178903510378E-5,
49.3031392543722));
#21424=CARTESIAN_POINT('Ctrl Pts',(-6.76700037226677,-0.169998519403827,
49.3111672172146));
#21425=CARTESIAN_POINT('Ctrl Pts',(-6.76058934995979,-0.34027818884635,
49.3191951800569));
#21426=CARTESIAN_POINT('Ctrl Pts',(-6.74773259984795,-0.510287919658342,
49.3272231428992));
#21427=CARTESIAN_POINT('Ctrl Pts',(-6.73488877417485,-0.680126745666957,
49.3352430355128));
#21428=CARTESIAN_POINT('Ctrl Pts',(-6.71561214204822,-0.849695800879844,
49.3432629281264));
#21429=CARTESIAN_POINT('Ctrl Pts',(-6.68992035983133,-1.01845695987328,
49.3512828207401));
#21430=CARTESIAN_POINT('Ctrl Pts',(-6.66424869218064,-1.18708599266867,
49.3592964344331));
#21431=CARTESIAN_POINT('Ctrl Pts',(-6.63217192635893,-1.35490801784299,
49.3673100481261));
#21432=CARTESIAN_POINT('Ctrl Pts',(-6.59375966618062,-1.52138833459762,
49.3753236618191));
#21433=CARTESIAN_POINT('Ctrl Pts',(-6.55342219520463,-1.69621259419569,
49.3837389153931));
#21434=CARTESIAN_POINT('Ctrl Pts',(-6.50609782033658,-1.86955676459864,
49.3921541689672));
#21435=CARTESIAN_POINT('Ctrl Pts',(-6.4519283527089,-2.04081099847856,49.4005694225413));
#21436=CARTESIAN_POINT('Ctrl Pts',(-6.40038451205324,-2.20376443570606,
49.4085767836673));
#21437=CARTESIAN_POINT('Ctrl Pts',(-6.34264360673731,-2.36482535153571,
49.4165841447933));
#21438=CARTESIAN_POINT('Ctrl Pts',(-6.27887940922215,-2.52348219023754,
49.4245915059194));
#21439=CARTESIAN_POINT('Ctrl Pts',(-6.21511890076893,-2.68212984988709,
49.4325984037815));
#21440=CARTESIAN_POINT('Ctrl Pts',(-6.14533593344823,-2.83837335948393,
49.4406053016436));
#21441=CARTESIAN_POINT('Ctrl Pts',(-6.06975281374618,-2.99172020416688,
49.4486121995057));
#21442=CARTESIAN_POINT('Ctrl Pts',(-5.99415888392195,-3.14508898097084,
49.4566202425382));
#21443=CARTESIAN_POINT('Ctrl Pts',(-5.91276331761375,-3.29555993067592,
49.4646282855706));
#21444=CARTESIAN_POINT('Ctrl Pts',(-5.82583475976305,-3.4426644262746,49.472636328603));
#21445=CARTESIAN_POINT('Ctrl Pts',(-5.73887630095644,-3.58981952164332,
49.4806471261749));
#21446=CARTESIAN_POINT('Ctrl Pts',(-5.64638125516209,-3.73360553489412,
49.4886579237468));
#21447=CARTESIAN_POINT('Ctrl Pts',(-5.54866191440153,-3.87358231610869,
49.4966687213186));
#21448=CARTESIAN_POINT('Ctrl Pts',(-5.45083898367368,-4.01370748340604,
49.504688010948));
#21449=CARTESIAN_POINT('Ctrl Pts',(-5.34778091813517,-4.15001504905328,
49.5127073005773));
#21450=CARTESIAN_POINT('Ctrl Pts',(-5.23984105520187,-4.28209699986127,
49.5207265902067));
#21451=CARTESIAN_POINT('Ctrl Pts',(-5.13183455085293,-4.41426049726332,
49.5287508308967));
#21452=CARTESIAN_POINT('Ctrl Pts',(-5.01894049648163,-4.54219290453409,
49.5367750715868));
#21453=CARTESIAN_POINT('Ctrl Pts',(-4.90154905527637,-4.66552310665367,
49.5447993122769));
#21454=CARTESIAN_POINT('Ctrl Pts',(-4.78399975275928,-4.78901915619189,
49.5528343435079));
#21455=CARTESIAN_POINT('Ctrl Pts',(-4.66194126130477,-4.90790038788604,
49.560869374739));
#21456=CARTESIAN_POINT('Ctrl Pts',(-4.53579723218991,-5.0218355676444,49.5689044059701));
#21457=CARTESIAN_POINT('Ctrl Pts',(-4.49191601804543,-5.06146973865232,
49.5716995198457));
#21458=CARTESIAN_POINT('Ctrl Pts',(-4.44754067122288,-5.10050576622392,
49.5744946337214));
#21459=CARTESIAN_POINT('Ctrl Pts',(-4.40268982281328,-5.13893095148168,
49.577289747597));
#21460=CARTESIAN_POINT('Ctrl Pts',(-4.27069073999476,-5.25201887269187,
49.585515956934));
#21461=CARTESIAN_POINT('Ctrl Pts',(-4.13414715702875,-5.36017579829563,
49.5937421662709));
#21462=CARTESIAN_POINT('Ctrl Pts',(-3.99346254917625,-5.46301618781482,
49.6019683756079));
#21463=CARTESIAN_POINT('Ctrl Pts',(-3.85293599445357,-5.56574104056219,
49.6101853431511));
#21464=CARTESIAN_POINT('Ctrl Pts',(-3.70827796566465,-5.66316104117019,
49.6184023106943));
#21465=CARTESIAN_POINT('Ctrl Pts',(-3.55992683843884,-5.75492918331432,
49.6266192782375));
#21466=CARTESIAN_POINT('Ctrl Pts',(-3.41171260208985,-5.84661264648313,
49.6348286635809));
#21467=CARTESIAN_POINT('Ctrl Pts',(-3.2598123571534,-5.93265445006514,49.6430380489243));
#21468=CARTESIAN_POINT('Ctrl Pts',(-3.10469551541618,-6.01274935088389,
49.6512474342676));
#21469=CARTESIAN_POINT('Ctrl Pts',(-2.94969068441236,-6.09278641472968,
49.6594508915682));
#21470=CARTESIAN_POINT('Ctrl Pts',(-2.79147420044349,-6.16688496542816,
49.6676543488688));
#21471=CARTESIAN_POINT('Ctrl Pts',(-2.63054234718681,-6.23478435550556,
49.6758578061694));
#21472=CARTESIAN_POINT('Ctrl Pts',(-2.46969442118183,-6.30264833550667,
49.6840569853013));
#21473=CARTESIAN_POINT('Ctrl Pts',(-2.30613427663016,-6.3643194563415,49.6922561644331));
#21474=CARTESIAN_POINT('Ctrl Pts',(-2.14038064566728,-6.41958407466192,
49.7004553435649));
#21475=CARTESIAN_POINT('Ctrl Pts',(-1.97465824626051,-6.47483827993728,
49.7086529777947));
#21476=CARTESIAN_POINT('Ctrl Pts',(-1.8067435215996,-6.52368826794435,49.7168506120245));
#21477=CARTESIAN_POINT('Ctrl Pts',(-1.63717322747893,-6.56596929807216,
49.7250482462543));
#21478=CARTESIAN_POINT('Ctrl Pts',(-1.46761517312772,-6.60824727630894,
49.7332452887699));
#21479=CARTESIAN_POINT('Ctrl Pts',(-1.2964021351184,-6.64395715333708,49.7414423312855));
#21480=CARTESIAN_POINT('Ctrl Pts',(-1.12408395493887,-6.67298465922476,
49.7496393738011));
#21481=CARTESIAN_POINT('Ctrl Pts',(-0.951746894333704,-6.70201534557585,
49.757837314444));
#21482=CARTESIAN_POINT('Ctrl Pts',(-0.778304804087646,-6.72436214250033,
49.7660352550868));
#21483=CARTESIAN_POINT('Ctrl Pts',(-0.604315646037443,-6.73996228475756,
49.7742331957296));
#21484=CARTESIAN_POINT('Ctrl Pts',(-0.430275802121834,-6.75556697158941,
49.7824335245656));
#21485=CARTESIAN_POINT('Ctrl Pts',(-0.255688930114081,-6.76442105687205,
49.7906338534016));
#21486=CARTESIAN_POINT('Ctrl Pts',(-0.0811160685115168,-6.7665138131411,
49.7988341822376));
#21487=CARTESIAN_POINT('Ctrl Pts',(0.0936387025426088,-6.76860875011647,
49.807043056029));
#21488=CARTESIAN_POINT('Ctrl Pts',(0.268379074897014,-6.76392827796832,
49.8152519298204));
#21489=CARTESIAN_POINT('Ctrl Pts',(0.442545051686371,-6.75251381910677,
49.8234608036118));
#21490=CARTESIAN_POINT('Ctrl Pts',(0.616804501434506,-6.74109323423105,
49.8316740830152));
#21491=CARTESIAN_POINT('Ctrl Pts',(0.79048858467799,-6.72293149516101,49.8398873624187));
#21492=CARTESIAN_POINT('Ctrl Pts',(0.963044560249353,-6.6981216900691,49.8481006418221));
#21493=CARTESIAN_POINT('Ctrl Pts',(1.1358529260556,-6.67327559673789,49.8563259344376));
#21494=CARTESIAN_POINT('Ctrl Pts',(1.30752953393986,-6.6417620696749,49.864551227053));
#21495=CARTESIAN_POINT('Ctrl Pts',(1.47753267223525,-6.60372517617726,49.8727765196685));
#21496=CARTESIAN_POINT('Ctrl Pts',(1.63128008929183,-6.56932537516913,49.8802153087805));
#21497=CARTESIAN_POINT('Ctrl Pts',(1.78365876575744,-6.52959079986507,49.8876540978925));
#21498=CARTESIAN_POINT('Ctrl Pts',(1.93428095369982,-6.48466238073765,49.8950928870045));
#21499=CARTESIAN_POINT('Ctrl Pts',(2.10084682581374,-6.43497819133045,49.9033190880233));
#21500=CARTESIAN_POINT('Ctrl Pts',(2.26572998687126,-6.37880278601693,49.9115452890422));
#21501=CARTESIAN_POINT('Ctrl Pts',(2.42838779218591,-6.31626643918403,49.919771490061));
#21502=CARTESIAN_POINT('Ctrl Pts',(2.59086288573823,-6.25380033875656,49.9279884506768));
#21503=CARTESIAN_POINT('Ctrl Pts',(2.75111726945716,-6.18498765233058,49.9362054112926));
#21504=CARTESIAN_POINT('Ctrl Pts',(2.9086217813601,-6.11000886521432,49.9444223719083));
#21505=CARTESIAN_POINT('Ctrl Pts',(3.06598098254605,-6.03509925212478,49.9526317517099));
#21506=CARTESIAN_POINT('Ctrl Pts',(3.22059504262432,-5.95403502084389,49.9608411315115));
#21507=CARTESIAN_POINT('Ctrl Pts',(3.37195308983396,-5.86704536883423,49.9690505113131));
#21508=CARTESIAN_POINT('Ctrl Pts',(3.52320186595561,-5.78011851793818,49.9772539644535));
#21509=CARTESIAN_POINT('Ctrl Pts',(3.67119900159623,-5.68727494490937,49.9854574175939));
#21510=CARTESIAN_POINT('Ctrl Pts',(3.81545655206118,-5.58879059361983,49.9936608707343));
#21511=CARTESIAN_POINT('Ctrl Pts',(3.95963889525941,-5.49035758618611,50.0018600470844));
#21512=CARTESIAN_POINT('Ctrl Pts',(4.10008524173568,-5.38628986074918,50.0100592234346));
#21513=CARTESIAN_POINT('Ctrl Pts',(4.23633499460492,-5.27690769423587,50.0182583997847));
#21514=CARTESIAN_POINT('Ctrl Pts',(4.3725591100272,-5.16754610962774,50.0264560333361));
#21515=CARTESIAN_POINT('Ctrl Pts',(4.50458792147498,-5.05287229525539,50.0346536668875));
#21516=CARTESIAN_POINT('Ctrl Pts',(4.63199217272379,-4.93324817050851,50.0428513004388));
#21517=CARTESIAN_POINT('Ctrl Pts',(4.75938724773965,-4.81363266163453,50.0510483435594));
#21518=CARTESIAN_POINT('Ctrl Pts',(4.88215816381982,-4.68906779733273,50.05924538668));
#21519=CARTESIAN_POINT('Ctrl Pts',(4.9999109985639,-4.55995383819176,50.0674424298005));
#21520=CARTESIAN_POINT('Ctrl Pts',(5.11767675359486,-4.43082571217832,50.0756403723317));
#21521=CARTESIAN_POINT('Ctrl Pts',(5.23042308858188,-4.29714776195844,50.0838383148629));
#21522=CARTESIAN_POINT('Ctrl Pts',(5.33779497401187,-4.15935497588432,50.0920362573941));
#21523=CARTESIAN_POINT('Ctrl Pts',(5.44519815542578,-4.02152202696123,50.1002365894025));
#21524=CARTESIAN_POINT('Ctrl Pts',(5.54722354658387,-3.87957213605305,50.1084369214109));
#21525=CARTESIAN_POINT('Ctrl Pts',(5.64355819131297,-3.7339710686164,50.1166372534193));
#21526=CARTESIAN_POINT('Ctrl Pts',(5.7399932427791,-3.58821824551458,50.1248461323901));
#21527=CARTESIAN_POINT('Ctrl Pts',(5.83072549980653,-3.43880694257282,50.1330550113609));
#21528=CARTESIAN_POINT('Ctrl Pts',(5.91548640475926,-3.28623030159306,50.1412638903316));
#21529=CARTESIAN_POINT('Ctrl Pts',(6.00029281133168,-3.13357175393362,50.149477176019));
#21530=CARTESIAN_POINT('Ctrl Pts',(6.07912131368349,-2.97774480051613,50.1576904617064));
#21531=CARTESIAN_POINT('Ctrl Pts',(6.15175071231138,-2.8192644738613,50.1659037473938));
#21532=CARTESIAN_POINT('Ctrl Pts',(6.22448635879819,-2.66055231002063,50.1741290481059));
#21533=CARTESIAN_POINT('Ctrl Pts',(6.29100464202356,-2.49917934749279,50.1823543488179));
#21534=CARTESIAN_POINT('Ctrl Pts',(6.35113318783342,-2.33567896561169,50.19057964953));
#21535=CARTESIAN_POINT('Ctrl Pts',(6.40551220434368,-2.18781259289312,50.1980184418241));
#21536=CARTESIAN_POINT('Ctrl Pts',(6.45466563267677,-2.0382065863057,50.2054572341182));
#21537=CARTESIAN_POINT('Ctrl Pts',(6.49850187116025,-1.88726321177699,50.2128960264123));
#21538=CARTESIAN_POINT('Ctrl Pts',(6.54654426625421,-1.72183658105326,50.2210485826255));
#21539=CARTESIAN_POINT('Ctrl Pts',(6.58834100216934,-1.55431554506159,50.2292011388388));
#21540=CARTESIAN_POINT('Ctrl Pts',(6.62370465993362,-1.38521679818492,50.237353695052));
#21541=CARTESIAN_POINT('Ctrl Pts',(6.6590273480479,-1.21631395628283,50.2454968063324));
#21542=CARTESIAN_POINT('Ctrl Pts',(6.6879317196072,-1.04583739610205,50.2536399176127));
#21543=CARTESIAN_POINT('Ctrl Pts',(6.71027965269082,-0.874320297536072,
50.2617830288931));
#21544=CARTESIAN_POINT('Ctrl Pts',(6.73260639352983,-0.702965846329679,
50.2699184181704));
#21545=CARTESIAN_POINT('Ctrl Pts',(6.7483890269995,-0.530573181193096,50.2780538074478));
#21546=CARTESIAN_POINT('Ctrl Pts',(6.75754015748445,-0.357687041958609,
50.2861891967251));
#21547=CARTESIAN_POINT('Ctrl Pts',(6.76668453294861,-0.184928520778165,
50.2943185807637));
#21548=CARTESIAN_POINT('Ctrl Pts',(6.76920713324293,-0.0116776143251095,
50.3024479648023));
#21549=CARTESIAN_POINT('Ctrl Pts',(6.76507221624997,0.161514423265437,50.3105773488409));
#21550=CARTESIAN_POINT('Ctrl Pts',(6.76093948296706,0.334614995611171,50.318702439633));
#21551=CARTESIAN_POINT('Ctrl Pts',(6.75015624322899,0.507656396368457,50.3268275304251));
#21552=CARTESIAN_POINT('Ctrl Pts',(6.73273882396683,0.680085971219667,50.3349526212172));
#21553=CARTESIAN_POINT('Ctrl Pts',(6.71525491863941,0.853173747139149,50.3431087272423));
#21554=CARTESIAN_POINT('Ctrl Pts',(6.69108607376356,1.02564464489716,50.3512648332674));
#21555=CARTESIAN_POINT('Ctrl Pts',(6.66030154434002,1.19694291361867,50.3594209392925));
#21556=CARTESIAN_POINT('Ctrl Pts',(6.62964091707995,1.36755173778832,50.367544218466));
#21557=CARTESIAN_POINT('Ctrl Pts',(6.59241784662351,1.53699699592338,50.3756674976394));
#21558=CARTESIAN_POINT('Ctrl Pts',(6.54875227082131,1.70473830701746,50.3837907768128));
#21559=CARTESIAN_POINT('Ctrl Pts',(6.50508088057863,1.87250195428485,50.3919151376695));
#21560=CARTESIAN_POINT('Ctrl Pts',(6.45496536843223,2.03856084851579,50.4000394985262));
#21561=CARTESIAN_POINT('Ctrl Pts',(6.39857595315297,2.20238842435493,50.4081638593829));
#21562=CARTESIAN_POINT('Ctrl Pts',(6.34216830077025,2.36626898425916,50.4162908477683));
#21563=CARTESIAN_POINT('Ctrl Pts',(6.2794828237427,2.5279164430318,50.4244178361537));
#21564=CARTESIAN_POINT('Ctrl Pts',(6.21073839413157,2.68682295651575,50.4325448245392));
#21565=CARTESIAN_POINT('Ctrl Pts',(6.14154953960981,2.84675678251727,50.4407243529792));
#21566=CARTESIAN_POINT('Ctrl Pts',(6.06622326924259,3.00391375563312,50.4489038814193));
#21567=CARTESIAN_POINT('Ctrl Pts',(5.98502988923725,3.15780085264045,50.4570834098594));
#21568=CARTESIAN_POINT('Ctrl Pts',(5.90421887503382,3.31096324569722,50.465224418263));
#21569=CARTESIAN_POINT('Ctrl Pts',(5.81759613095532,3.46088620999193,50.4733654266667));
#21570=CARTESIAN_POINT('Ctrl Pts',(5.72547174231819,3.60711274122614,50.4815064350704));
#21571=CARTESIAN_POINT('Ctrl Pts',(5.63269350934899,3.75437710174812,50.4897052235287));
#21572=CARTESIAN_POINT('Ctrl Pts',(5.53433546335785,3.89789205475113,50.4979040119869));
#21573=CARTESIAN_POINT('Ctrl Pts',(5.43075535893094,4.03722494189299,50.5061028004452));
#21574=CARTESIAN_POINT('Ctrl Pts',(5.32717525450403,4.17655782903485,50.5143015889034));
#21575=CARTESIAN_POINT('Ctrl Pts',(5.21837337498346,4.31170840166453,50.5225003773617));
#21576=CARTESIAN_POINT('Ctrl Pts',(5.10474461150638,4.44228223453852,50.5306991658199));
#21577=CARTESIAN_POINT('Ctrl Pts',(4.99061989257435,4.57342598301052,50.5389337395295));
#21578=CARTESIAN_POINT('Ctrl Pts',(4.87127132453099,4.70036077080625,50.5471683132391));
#21579=CARTESIAN_POINT('Ctrl Pts',(4.74704009445691,4.82264443450049,50.5554028869487));
#21580=CARTESIAN_POINT('Ctrl Pts',(4.62299741549927,4.94474250298411,50.5636249626892));
#21581=CARTESIAN_POINT('Ctrl Pts',(4.49408709554759,5.06220326617622,50.5718470384298));
#21582=CARTESIAN_POINT('Ctrl Pts',(4.36069029164882,5.17461778108487,50.5800691141703));
#21583=CARTESIAN_POINT('Ctrl Pts',(4.22740969371894,5.28693436832779,50.5882840274133));
#21584=CARTESIAN_POINT('Ctrl Pts',(4.08965066291297,5.39421322799149,50.5964989406564));
#21585=CARTESIAN_POINT('Ctrl Pts',(3.94783148302989,5.49608183905572,50.6047138538994));
#21586=CARTESIAN_POINT('Ctrl Pts',(3.80613172030727,5.5978646728627,50.612921849872));
#21587=CARTESIAN_POINT('Ctrl Pts',(3.66037890926252,5.69424612619518,50.6211298458447));
#21588=CARTESIAN_POINT('Ctrl Pts',(3.51102457414039,5.78489372761353,50.6293378418173));
#21589=CARTESIAN_POINT('Ctrl Pts',(3.37654407855222,5.86651395211287,50.636728423184));
#21590=CARTESIAN_POINT('Ctrl Pts',(3.23914426110165,5.94348589201141,50.6441190045507));
#21591=CARTESIAN_POINT('Ctrl Pts',(3.09917575053255,6.01559628526641,50.6515095859174));
#21592=CARTESIAN_POINT('Origin',(0.,0.,-3.69717978381041));
#21593=CARTESIAN_POINT('',(3.09917575053258,6.01559628526639,53.0455807084606));
#21594=CARTESIAN_POINT('',(3.09917575053253,6.01559628526642,52.6511649350805));
#21595=CARTESIAN_POINT('',(3.09917575053259,6.01559628526639,-3.69717978381041));
#21596=CARTESIAN_POINT('',(-6.76699995210602,-0.000805106932658668,51.69717978381));
#21597=CARTESIAN_POINT('Ctrl Pts',(-6.76699995210602,-0.000805106932658668,
51.69717978381));
#21598=CARTESIAN_POINT('Ctrl Pts',(-6.76697776002256,-0.187331668327564,
51.7059085008878));
#21599=CARTESIAN_POINT('Ctrl Pts',(-6.75923913773472,-0.373667474836227,
51.7146372179655));
#21600=CARTESIAN_POINT('Ctrl Pts',(-6.74385683031687,-0.55918159142499,
51.7233659350433));
#21601=CARTESIAN_POINT('Ctrl Pts',(-6.72844715360874,-0.745025787862566,
51.7321101828724));
#21602=CARTESIAN_POINT('Ctrl Pts',(-6.70536664484977,-0.930045094505219,
51.7408544307015));
#21603=CARTESIAN_POINT('Ctrl Pts',(-6.67473938789428,-1.11361712616714,
51.7495986785305));
#21604=CARTESIAN_POINT('Ctrl Pts',(-6.64402544099753,-1.29770875541049,
51.7583676768076));
#21605=CARTESIAN_POINT('Ctrl Pts',(-6.60572205444346,-1.48034463564412,
51.7671366750847));
#21606=CARTESIAN_POINT('Ctrl Pts',(-6.56000430699961,-1.66091315009141,
51.7759056733618));
#21607=CARTESIAN_POINT('Ctrl Pts',(-6.51422000550895,-1.84174452887551,
51.7846874371918));
#21608=CARTESIAN_POINT('Ctrl Pts',(-6.46099986358177,-2.02050226191529,
51.7934692010217));
#21609=CARTESIAN_POINT('Ctrl Pts',(-6.40056811135066,-2.19659209958543,
51.8022509648517));
#21610=CARTESIAN_POINT('Ctrl Pts',(-6.33999002914278,-2.37310832273842,
51.8110539929219));
#21611=CARTESIAN_POINT('Ctrl Pts',(-6.27216550584455,-2.54694346518936,
51.8198570209921));
#21612=CARTESIAN_POINT('Ctrl Pts',(-6.19736705102892,-2.71752288579529,
51.8286600490622));
#21613=CARTESIAN_POINT('Ctrl Pts',(-6.14343480472519,-2.84051648705539,
51.8350073336321));
#21614=CARTESIAN_POINT('Ctrl Pts',(-6.08587786014791,-2.96181796013422,
51.8413546182019));
#21615=CARTESIAN_POINT('Ctrl Pts',(-6.0248127130065,-3.08122066285349,51.8477019027718));
#21616=CARTESIAN_POINT('Ctrl Pts',(-5.94639478163091,-3.23455383875197,
51.8558528849461));
#21617=CARTESIAN_POINT('Ctrl Pts',(-5.86199628252426,-3.38513229218628,
51.8640038671204));
#21618=CARTESIAN_POINT('Ctrl Pts',(-5.77183468666551,-3.5324514646071,51.8721548492947));
#21619=CARTESIAN_POINT('Ctrl Pts',(-5.68177782185669,-3.67959951215535,
51.8802963633477));
#21620=CARTESIAN_POINT('Ctrl Pts',(-5.5859713748947,-3.82349550620328,51.8884378774007));
#21621=CARTESIAN_POINT('Ctrl Pts',(-5.48468001845993,-3.96365665706635,
51.8965793914538));
#21622=CARTESIAN_POINT('Ctrl Pts',(-5.38348500590702,-4.10368449280921,
51.9047131616569));
#21623=CARTESIAN_POINT('Ctrl Pts',(-5.27681568289663,-4.23998426334832,
51.9128469318599));
#21624=CARTESIAN_POINT('Ctrl Pts',(-5.1649815891154,-4.3720995167195,51.920980702063));
#21625=CARTESIAN_POINT('Ctrl Pts',(-5.05323034599209,-4.50411689443139,
51.929108446481));
#21626=CARTESIAN_POINT('Ctrl Pts',(-4.93632218602984,-4.63195564968424,
51.937236190899));
#21627=CARTESIAN_POINT('Ctrl Pts',(-4.81460873288302,-4.75518998035269,
51.945363935317));
#21628=CARTESIAN_POINT('Ctrl Pts',(-4.69295986003724,-4.87835892375318,
51.953487367211));
#21629=CARTESIAN_POINT('Ctrl Pts',(-4.56651102810959,-4.99692804838911,
51.9616107991051));
#21630=CARTESIAN_POINT('Ctrl Pts',(-4.43565274173749,-5.11050621315704,
51.9697342309991));
#21631=CARTESIAN_POINT('Ctrl Pts',(-4.303964341867,-5.22480487312867,51.9779091947499));
#21632=CARTESIAN_POINT('Ctrl Pts',(-4.16781059763206,-5.33404875060903,
51.9860841585008));
#21633=CARTESIAN_POINT('Ctrl Pts',(-4.02762598954331,-5.43787806854432,
51.9942591222516));
#21634=CARTESIAN_POINT('Ctrl Pts',(-3.88835665086666,-5.54102948182173,
52.0023807114246));
#21635=CARTESIAN_POINT('Ctrl Pts',(-3.74510924011445,-5.63883662977525,
52.0105023005976));
#21636=CARTESIAN_POINT('Ctrl Pts',(-3.59834138050517,-5.73098842341739,
52.0186238897707));
#21637=CARTESIAN_POINT('Ctrl Pts',(-3.45155414452848,-5.82315238298616,
52.0267465511601));
#21638=CARTESIAN_POINT('Ctrl Pts',(-3.30124584393747,-5.90965930647105,
52.0348692125494));
#21639=CARTESIAN_POINT('Ctrl Pts',(-3.14790123780602,-5.99024263256667,
52.0429918739388));
#21640=CARTESIAN_POINT('Ctrl Pts',(-2.99450718569254,-6.07085194276305,
52.051117154481));
#21641=CARTESIAN_POINT('Ctrl Pts',(-2.83807520224387,-6.14553368188226,
52.0592424350233));
#21642=CARTESIAN_POINT('Ctrl Pts',(-2.67911263257415,-6.21406827303833,
52.0673677155656));
#21643=CARTESIAN_POINT('Ctrl Pts',(-2.51841819869326,-6.28334953434384,
52.0755815193533));
#21644=CARTESIAN_POINT('Ctrl Pts',(-2.35513806783831,-6.3463487670734,52.0837953231411));
#21645=CARTESIAN_POINT('Ctrl Pts',(-2.18981398807035,-6.40289026125323,
52.0920091269288));
#21646=CARTESIAN_POINT('Ctrl Pts',(-2.02598866772291,-6.45891917373793,
52.100148467784));
#21647=CARTESIAN_POINT('Ctrl Pts',(-1.86015667324503,-6.50860690949064,
52.1082878086392));
#21648=CARTESIAN_POINT('Ctrl Pts',(-1.69285694530543,-6.5518336641532,52.1164271494943));
#21649=CARTESIAN_POINT('Ctrl Pts',(-1.52326139969761,-6.5956536101396,52.1246781847484));
#21650=CARTESIAN_POINT('Ctrl Pts',(-1.35215792933208,-6.63283388052945,
52.1329292200024));
#21651=CARTESIAN_POINT('Ctrl Pts',(-1.18011453005237,-6.66330388740895,
52.1411802552564));
#21652=CARTESIAN_POINT('Ctrl Pts',(-1.00807113077267,-6.69377389428846,
52.1494312905105));
#21653=CARTESIAN_POINT('Ctrl Pts',(-0.835088192012403,-6.71753365186203,
52.1576823257645));
#21654=CARTESIAN_POINT('Ctrl Pts',(-0.661734484834696,-6.73456728168786,
52.1659333610185));
#21655=CARTESIAN_POINT('Ctrl Pts',(-0.488785496707557,-6.75156114406595,
52.1741651330494));
#21656=CARTESIAN_POINT('Ctrl Pts',(-0.314927570707862,-6.76191347781179,
52.1823969050802));
#21657=CARTESIAN_POINT('Ctrl Pts',(-0.140711821677379,-6.76553687324519,
52.190628677111));
#21658=CARTESIAN_POINT('Ctrl Pts',(0.0332958963387049,-6.76915594198233,
52.1988506195834));
#21659=CARTESIAN_POINT('Ctrl Pts',(0.207660231874101,-6.76606206461893,
52.2070725620558));
#21660=CARTESIAN_POINT('Ctrl Pts',(0.381823245449463,-6.75621935769069,
52.2152945045282));
#21661=CARTESIAN_POINT('Ctrl Pts',(0.555813186072828,-6.74638643186528,
52.2235082765181));
#21662=CARTESIAN_POINT('Ctrl Pts',(0.729601847885147,-6.72981805269848,
52.231722048508));
#21663=CARTESIAN_POINT('Ctrl Pts',(0.902629477736182,-6.70653032692179,
52.2399358204979));
#21664=CARTESIAN_POINT('Ctrl Pts',(1.07551981792611,-6.68326107891067,52.2481430752283));
#21665=CARTESIAN_POINT('Ctrl Pts',(1.24764997537319,-6.65328315106042,52.2563503299586));
#21666=CARTESIAN_POINT('Ctrl Pts',(1.41846341614987,-6.61666460817264,52.264557584689));
#21667=CARTESIAN_POINT('Ctrl Pts',(1.58917552675394,-6.58006778818474,52.2727599707009));
#21668=CARTESIAN_POINT('Ctrl Pts',(1.75857212732575,-6.53683827572664,52.2809623567129));
#21669=CARTESIAN_POINT('Ctrl Pts',(1.92610490867979,-6.48709556587227,52.2891647427249));
#21670=CARTESIAN_POINT('Ctrl Pts',(2.09358768556224,-6.43736770301023,52.2973646805236));
#21671=CARTESIAN_POINT('Ctrl Pts',(2.25920740719941,-6.38113061332355,52.3055646183223));
#21672=CARTESIAN_POINT('Ctrl Pts',(2.4224287672088,-6.31855425455849,52.313764556121));
#21673=CARTESIAN_POINT('Ctrl Pts',(2.58562730465929,-6.25598664558351,52.3219633473567));
#21674=CARTESIAN_POINT('Ctrl Pts',(2.74642781353569,-6.18708166040106,52.3301621385925));
#21675=CARTESIAN_POINT('Ctrl Pts',(2.90431287157553,-6.11205822485362,52.3383609298282));
#21676=CARTESIAN_POINT('Ctrl Pts',(3.06220449437847,-6.0370316698781,52.3465600619647));
#21677=CARTESIAN_POINT('Ctrl Pts',(3.21718010105147,-5.95588631147893,52.3547591941011));
#21678=CARTESIAN_POINT('Ctrl Pts',(3.36874482540485,-5.86888808048919,52.3629583262375));
#21679=CARTESIAN_POINT('Ctrl Pts',(3.52034334625225,-5.78187045029421,52.3711592866484));
#21680=CARTESIAN_POINT('Ctrl Pts',(3.66852915914536,-5.68899752652939,52.3793602470593));
#21681=CARTESIAN_POINT('Ctrl Pts',(3.81283440679735,-5.59057982559433,52.3875612074702));
#21682=CARTESIAN_POINT('Ctrl Pts',(3.95727490320491,-5.49206988358146,52.3957698541553));
#21683=CARTESIAN_POINT('Ctrl Pts',(4.09782727131412,-5.38800498374804,52.4039785008403));
#21684=CARTESIAN_POINT('Ctrl Pts',(4.23405416241301,-5.27873795047198,52.4121871475253));
#21685=CARTESIAN_POINT('Ctrl Pts',(4.37034609205585,-5.1694187500453,52.4203997132489));
#21686=CARTESIAN_POINT('Ctrl Pts',(4.50230815666514,-5.05489269901851,52.4286122789724));
#21687=CARTESIAN_POINT('Ctrl Pts',(4.62953829304672,-4.93555105263983,52.4368248446959));
#21688=CARTESIAN_POINT('Ctrl Pts',(4.75694300753476,-4.81604565230128,52.4450486792446));
#21689=CARTESIAN_POINT('Ctrl Pts',(4.87960256561733,-4.69171170605568,52.4532725137934));
#21690=CARTESIAN_POINT('Ctrl Pts',(4.99715294271958,-4.56297616332466,52.4614963483422));
#21691=CARTESIAN_POINT('Ctrl Pts',(5.10515962701359,-4.44469241584614,52.4690525053167));
#21692=CARTESIAN_POINT('Ctrl Pts',(5.20885338823642,-4.32269332652127,52.4766086622911));
#21693=CARTESIAN_POINT('Ctrl Pts',(5.30798369569739,-4.1973322582577,52.4841648192656));
#21694=CARTESIAN_POINT('Ctrl Pts',(5.42140811126335,-4.05389473378399,52.492810537318));
#21695=CARTESIAN_POINT('Ctrl Pts',(5.52911641506232,-3.90572865115852,52.5014562553704));
#21696=CARTESIAN_POINT('Ctrl Pts',(5.63071799218921,-3.75330572861268,52.5101019734228));
#21697=CARTESIAN_POINT('Ctrl Pts',(5.73218913359683,-3.60107848603656,52.5187365921351));
#21698=CARTESIAN_POINT('Ctrl Pts',(5.82756901293679,-3.44460555341883,52.5273712108475));
#21699=CARTESIAN_POINT('Ctrl Pts',(5.91650808941616,-3.284390510867,52.5360058295599));
#21700=CARTESIAN_POINT('Ctrl Pts',(6.00858814857537,-3.11851729539922,52.5449453894623));
#21701=CARTESIAN_POINT('Ctrl Pts',(6.09376395189131,-2.94863306633431,52.5538849493647));
#21702=CARTESIAN_POINT('Ctrl Pts',(6.17169573986025,-2.77533073607288,52.5628245092671));
#21703=CARTESIAN_POINT('Ctrl Pts',(6.24676024105247,-2.60840459058642,52.5714351625376));
#21704=CARTESIAN_POINT('Ctrl Pts',(6.31510408129153,-2.43830767506642,52.5800458158081));
#21705=CARTESIAN_POINT('Ctrl Pts',(6.37646938595806,-2.26559642697891,52.5886564690786));
#21706=CARTESIAN_POINT('Ctrl Pts',(6.43777660425816,-2.09304866164275,52.5972589717897));
#21707=CARTESIAN_POINT('Ctrl Pts',(6.49211835510333,-1.91789178395019,52.6058614745008));
#21708=CARTESIAN_POINT('Ctrl Pts',(6.53928460601878,-1.74070268612588,52.6144639772119));
#21709=CARTESIAN_POINT('Ctrl Pts',(6.58639777226828,-1.56371301106435,52.6230567979794));
#21710=CARTESIAN_POINT('Ctrl Pts',(6.62635147144205,-1.38469597291436,52.6316496187469));
#21711=CARTESIAN_POINT('Ctrl Pts',(6.65898525322215,-1.20424432627685,52.6402424395144));
#21712=CARTESIAN_POINT('Ctrl Pts',(6.66283129263544,-1.18297728006574,52.6412551424725));
#21713=CARTESIAN_POINT('Ctrl Pts',(6.66657571754772,-1.16169032500973,52.6422678454306));
#21714=CARTESIAN_POINT('Ctrl Pts',(6.67021831111871,-1.14038444483285,52.6432805483887));
#21715=CARTESIAN_POINT('Ctrl Pts',(6.70113461328505,-0.959552019630638,
52.6518758061487));
#21716=CARTESIAN_POINT('Ctrl Pts',(6.72467477233005,-0.777568192048651,
52.6604710639087));
#21717=CARTESIAN_POINT('Ctrl Pts',(6.74078702283454,-0.595045639245815,
52.6690663216688));
#21718=CARTESIAN_POINT('Ctrl Pts',(6.75691436177832,-0.412352161812903,
52.6776696285232));
#21719=CARTESIAN_POINT('Ctrl Pts',(6.76559988104457,-0.229119256336365,
52.6862729353776));
#21720=CARTESIAN_POINT('Ctrl Pts',(6.7668439141714,-0.0459613015649521,
52.694876242232));
#21721=CARTESIAN_POINT('Ctrl Pts',(6.76813952534306,0.144790445526304,52.703836245172));
#21722=CARTESIAN_POINT('Ctrl Pts',(6.76136345946303,0.335460513310029,52.712796248112));
#21723=CARTESIAN_POINT('Ctrl Pts',(6.74657584249044,0.525360258798081,52.7217562510521));
#21724=CARTESIAN_POINT('Ctrl Pts',(6.7323380733906,0.708198963194397,52.7303830942568));
#21725=CARTESIAN_POINT('Ctrl Pts',(6.71067387788064,0.890323309720602,52.7390099374615));
#21726=CARTESIAN_POINT('Ctrl Pts',(6.68168941773004,1.07112815526175,52.7476367806663));
#21727=CARTESIAN_POINT('Ctrl Pts',(6.65267725576229,1.25210580453098,52.7562718689524));
#21728=CARTESIAN_POINT('Ctrl Pts',(6.61633092131939,1.43176113616266,52.7649069572385));
#21729=CARTESIAN_POINT('Ctrl Pts',(6.57280725018437,1.60950111895699,52.7735420455246));
#21730=CARTESIAN_POINT('Ctrl Pts',(6.52921893766329,1.78750508129504,52.7821899586497));
#21731=CARTESIAN_POINT('Ctrl Pts',(6.47843206682968,1.96358771594611,52.7908378717748));
#21732=CARTESIAN_POINT('Ctrl Pts',(6.42065313210189,2.13717157879993,52.7994857849));
#21733=CARTESIAN_POINT('Ctrl Pts',(6.41417121520304,2.15664504571831,52.8004559491041));
#21734=CARTESIAN_POINT('Ctrl Pts',(6.40760134973931,2.17608708599836,52.8014261133082));
#21735=CARTESIAN_POINT('Ctrl Pts',(6.40094386457128,2.19549690106985,52.8023962775123));
#21736=CARTESIAN_POINT('Ctrl Pts',(6.34449558867436,2.36007114624046,52.8106222209846));
#21737=CARTESIAN_POINT('Ctrl Pts',(6.28162179823061,2.52268390004036,52.818848164457));
#21738=CARTESIAN_POINT('Ctrl Pts',(6.21247796981053,2.68279825455043,52.8270741079293));
#21739=CARTESIAN_POINT('Ctrl Pts',(6.14340912648672,2.84273896825175,52.8352911305307));
#21740=CARTESIAN_POINT('Ctrl Pts',(6.06808392849906,3.00018635222957,52.8435081531322));
#21741=CARTESIAN_POINT('Ctrl Pts',(5.98670738887978,3.15461941285036,52.8517251757336));
#21742=CARTESIAN_POINT('Ctrl Pts',(5.90541625048179,3.30889040253464,52.8599335749189));
#21743=CARTESIAN_POINT('Ctrl Pts',(5.81808659401201,3.46015305840489,52.8681419741042));
#21744=CARTESIAN_POINT('Ctrl Pts',(5.72497110107103,3.60790727318505,52.8763503732895));
#21745=CARTESIAN_POINT('Ctrl Pts',(5.63191132478228,3.75557307764873,52.8845538608913));
#21746=CARTESIAN_POINT('Ctrl Pts',(5.53307279596194,3.89973431912708,52.8927573484931));
#21747=CARTESIAN_POINT('Ctrl Pts',(5.42875384719854,4.03991592320027,52.9009608360948));
#21748=CARTESIAN_POINT('Ctrl Pts',(5.32447839363699,4.18003907933818,52.9091609032983));
#21749=CARTESIAN_POINT('Ctrl Pts',(5.21472728457515,4.31618561582027,52.9173609705019));
#21750=CARTESIAN_POINT('Ctrl Pts',(5.09984188074631,4.44790982275787,52.9255610377054));
#21751=CARTESIAN_POINT('Ctrl Pts',(4.98498353674963,4.57960300369207,52.9337591734848));
#21752=CARTESIAN_POINT('Ctrl Pts',(4.86499354277201,4.70687566058062,52.9419573092641));
#21753=CARTESIAN_POINT('Ctrl Pts',(4.74025324529591,4.8293154970929,52.9501554450435));
#21754=CARTESIAN_POINT('Ctrl Pts',(4.61548608009013,4.95178170584009,52.9583553466139));
#21755=CARTESIAN_POINT('Ctrl Pts',(4.48596681833585,5.06941275856206,52.9665552481843));
#21756=CARTESIAN_POINT('Ctrl Pts',(4.35211370372905,5.18183319972901,52.9747551497547));
#21757=CARTESIAN_POINT('Ctrl Pts',(4.2182492492111,5.29426316505099,52.9829557460131));
#21758=CARTESIAN_POINT('Ctrl Pts',(4.08005048847611,5.40148141307023,52.9911563422715));
#21759=CARTESIAN_POINT('Ctrl Pts',(3.93796841058711,5.50315307775624,52.9993569385299));
#21760=CARTESIAN_POINT('Ctrl Pts',(3.79578526474136,5.60489706505721,53.0075633681596));
#21761=CARTESIAN_POINT('Ctrl Pts',(3.64971357664433,5.70108638035999,53.0157697977892));
#21762=CARTESIAN_POINT('Ctrl Pts',(3.50023361237609,5.79142932779056,53.0239762274189));
#21763=CARTESIAN_POINT('Ctrl Pts',(3.36905853787642,5.87070913574167,53.0311777210994));
#21764=CARTESIAN_POINT('Ctrl Pts',(3.23525936987647,5.94548734957398,53.03837921478));
#21765=CARTESIAN_POINT('Ctrl Pts',(3.09917575053258,6.01559628526639,53.0455807084606));
#21766=CARTESIAN_POINT('Ctrl Pts',(3.0991757505326,6.01559628526638,51.0457515827422));
#21767=CARTESIAN_POINT('Ctrl Pts',(2.93382384459266,6.10078395293759,51.0545010306546));
#21768=CARTESIAN_POINT('Ctrl Pts',(2.76495772122985,6.17915010267049,51.063250478567));
#21769=CARTESIAN_POINT('Ctrl Pts',(2.59315093316712,6.25042856433177,51.0719999264794));
#21770=CARTESIAN_POINT('Ctrl Pts',(2.42134553245628,6.32170645041447,51.0807493037394));
#21771=CARTESIAN_POINT('Ctrl Pts',(2.24659977927612,6.38589665313449,51.0894986809994));
#21772=CARTESIAN_POINT('Ctrl Pts',(2.06950718689951,6.44278115439065,51.0982480582594));
#21773=CARTESIAN_POINT('Ctrl Pts',(1.89241596572898,6.49966521519713,51.1069973677741));
#21774=CARTESIAN_POINT('Ctrl Pts',(1.71297821457239,6.54924360009535,51.1157466772887));
#21775=CARTESIAN_POINT('Ctrl Pts',(1.53180337335891,6.59134792173545,51.1244959868034));
#21776=CARTESIAN_POINT('Ctrl Pts',(1.35062987477834,6.63345193135294,51.1332452314795));
#21777=CARTESIAN_POINT('Ctrl Pts',(1.16771959103009,6.66808192368228,51.1419944761557));
#21778=CARTESIAN_POINT('Ctrl Pts',(0.983693746907472,6.69512028363159,51.1507437208318));
#21779=CARTESIAN_POINT('Ctrl Pts',(0.799669205420609,6.72215845218858,51.1594929035759));
#21780=CARTESIAN_POINT('Ctrl Pts',(0.614529402874324,6.74160505424571,51.1682420863201));
#21781=CARTESIAN_POINT('Ctrl Pts',(0.428903127364207,6.75339404354116,51.1769912690643));
#21782=CARTESIAN_POINT('Ctrl Pts',(0.243278104164781,6.76518295330327,51.1857403927829));
#21783=CARTESIAN_POINT('Ctrl Pts',(0.0571669005399603,6.76931433552275,
51.1944895165015));
#21784=CARTESIAN_POINT('Ctrl Pts',(-0.12879840477673,6.76577415902474,51.2032386402201));
#21785=CARTESIAN_POINT('Ctrl Pts',(-0.314762517258233,6.76223400523445,
51.2119877078193));
#21786=CARTESIAN_POINT('Ctrl Pts',(-0.500580446818562,6.75102239665096,
51.2207367754185));
#21787=CARTESIAN_POINT('Ctrl Pts',(-0.685621118841584,6.73217741012508,
51.2294858430177));
#21788=CARTESIAN_POINT('Ctrl Pts',(-0.870660665413498,6.71333253821785,
51.2382348574035));
#21789=CARTESIAN_POINT('Ctrl Pts',(-1.05492267885391,6.68685441030627,51.2469838717893));
#21790=CARTESIAN_POINT('Ctrl Pts',(-1.23778137635161,6.65283295028194,51.2557328861751));
#21791=CARTESIAN_POINT('Ctrl Pts',(-1.42999922978755,6.61707018861885,51.2649296965425));
#21792=CARTESIAN_POINT('Ctrl Pts',(-1.62066601233603,6.57297172934436,51.2741265069099));
#21793=CARTESIAN_POINT('Ctrl Pts',(-1.80906628500293,6.5207030431132,51.2833233172772));
#21794=CARTESIAN_POINT('Ctrl Pts',(-1.98831342545431,6.4709737491506,51.292073315015));
#21795=CARTESIAN_POINT('Ctrl Pts',(-2.16550875896602,6.41384933989562,51.3008233127528));
#21796=CARTESIAN_POINT('Ctrl Pts',(-2.34005036713908,6.34952386240514,51.3095733104905));
#21797=CARTESIAN_POINT('Ctrl Pts',(-2.51458843546987,6.28519968948637,51.3183231307714));
#21798=CARTESIAN_POINT('Ctrl Pts',(-2.68647261717955,6.21367483971142,51.3270729510523));
#21799=CARTESIAN_POINT('Ctrl Pts',(-2.85511905908633,6.1351922674389,51.3358227713331));
#21800=CARTESIAN_POINT('Ctrl Pts',(-3.02376230488782,6.05671118252988,51.3445724257917));
#21801=CARTESIAN_POINT('Ctrl Pts',(-3.18916767379798,5.97127275992689,51.3533220802502));
#21802=CARTESIAN_POINT('Ctrl Pts',(-3.35077334102678,5.87916720438059,51.3620717347087));
#21803=CARTESIAN_POINT('Ctrl Pts',(-3.51237616037259,5.78706327195709,51.3708212349772));
#21804=CARTESIAN_POINT('Ctrl Pts',(-3.67017916302191,5.68829258362369,51.3795707352456));
#21805=CARTESIAN_POINT('Ctrl Pts',(-3.82364636566354,5.58319061741116,51.3883202355141));
#21806=CARTESIAN_POINT('Ctrl Pts',(-3.97711106778698,5.47809036367774,51.3970695932225));
#21807=CARTESIAN_POINT('Ctrl Pts',(-4.12623987481836,5.36665920043295,51.4058189509309));
#21808=CARTESIAN_POINT('Ctrl Pts',(-4.27052628213847,5.24927559512402,51.4145683086394));
#21809=CARTESIAN_POINT('Ctrl Pts',(-4.41481053024885,5.13189374643116,51.4233175354159));
#21810=CARTESIAN_POINT('Ctrl Pts',(-4.55425230136427,5.00855981477447,51.4320667621924));
#21811=CARTESIAN_POINT('Ctrl Pts',(-4.68837800630435,4.87969268192185,51.4408159889689));
#21812=CARTESIAN_POINT('Ctrl Pts',(-4.82250188228773,4.75082730631932,51.4495650964397));
#21813=CARTESIAN_POINT('Ctrl Pts',(-4.95130963052837,4.61642907903663,51.4583142039106));
#21814=CARTESIAN_POINT('Ctrl Pts',(-5.07436379033232,4.47695444731843,51.4670633113814));
#21815=CARTESIAN_POINT('Ctrl Pts',(-5.19741643562648,4.33748153220773,51.4758123111711));
#21816=CARTESIAN_POINT('Ctrl Pts',(-5.31471544462597,4.19293255254811,51.4845613109609));
#21817=CARTESIAN_POINT('Ctrl Pts',(-5.42586245275435,4.04379841779862,51.4933103107506));
#21818=CARTESIAN_POINT('Ctrl Pts',(-5.53702160018961,3.89464799484615,51.5020602660927));
#21819=CARTESIAN_POINT('Ctrl Pts',(-5.64202723081062,3.74091164444135,51.5108102214349));
#21820=CARTESIAN_POINT('Ctrl Pts',(-5.74052265232781,3.58311159163531,51.519560176777));
#21821=CARTESIAN_POINT('Ctrl Pts',(-5.83901427066747,3.42531763192076,51.5283097942595));
#21822=CARTESIAN_POINT('Ctrl Pts',(-5.93099603115583,3.26346052695898,51.537059411742));
#21823=CARTESIAN_POINT('Ctrl Pts',(-6.0161555062261,3.09809004467355,51.5458090292244));
#21824=CARTESIAN_POINT('Ctrl Pts',(-6.10131214578663,2.93272506864111,51.5545583553755));
#21825=CARTESIAN_POINT('Ctrl Pts',(-6.17964682328618,2.76384720417183,51.5633076815266));
#21826=CARTESIAN_POINT('Ctrl Pts',(-6.25089348288442,2.59203002791887,51.5720570076777));
#21827=CARTESIAN_POINT('Ctrl Pts',(-6.32213814889222,2.42021765937313,51.5808060890093));
#21828=CARTESIAN_POINT('Ctrl Pts',(-6.38629508412489,2.24546640832192,51.5895551703408));
#21829=CARTESIAN_POINT('Ctrl Pts',(-6.44314639819727,2.06836976660304,51.5983042516724));
#21830=CARTESIAN_POINT('Ctrl Pts',(-6.50000285283626,1.89125711158531,51.6070541241068));
#21831=CARTESIAN_POINT('Ctrl Pts',(-6.54955227673185,1.71179891440502,51.6158039965412));
#21832=CARTESIAN_POINT('Ctrl Pts',(-6.59162635926329,1.5306047627867,51.6245538689756));
#21833=CARTESIAN_POINT('Ctrl Pts',(-6.63369752055148,1.34942319164934,51.6333031338981));
#21834=CARTESIAN_POINT('Ctrl Pts',(-6.66829431424213,1.1665061864294,51.6420523988206));
#21835=CARTESIAN_POINT('Ctrl Pts',(-6.69529923745383,0.982474997620903,
51.6508016637431));
#21836=CARTESIAN_POINT('Ctrl Pts',(-6.72230554731416,0.798434359180046,
51.6595513779228));
#21837=CARTESIAN_POINT('Ctrl Pts',(-6.74171916496683,0.613279706242597,
51.6683010921025));
#21838=CARTESIAN_POINT('Ctrl Pts',(-6.75347414817261,0.427639953657591,
51.6770508062822));
#21839=CARTESIAN_POINT('Ctrl Pts',(-6.76248837758738,0.285283364200273,
51.6837604654581));
#21840=CARTESIAN_POINT('Ctrl Pts',(-6.76699999999995,0.142641701106303,
51.6904701246341));
#21841=CARTESIAN_POINT('Ctrl Pts',(-6.767,2.23847959696427E-12,51.69717978381));
#21842=CARTESIAN_POINT('',(-6.76699991050681,0.00110054571900286,51.3028202161511));
#21843=CARTESIAN_POINT('Ctrl Pts',(3.09917575053255,6.01559628526641,50.6515095859174));
#21844=CARTESIAN_POINT('Ctrl Pts',(2.94372576997178,6.09568257884875,50.6597176158886));
#21845=CARTESIAN_POINT('Ctrl Pts',(2.78510729620925,6.1697715374377,50.6679256458599));
#21846=CARTESIAN_POINT('Ctrl Pts',(2.6238253565943,6.23761408698012,50.6761336758311));
#21847=CARTESIAN_POINT('Ctrl Pts',(2.46269641988174,6.30539227651415,50.6843339191127));
#21848=CARTESIAN_POINT('Ctrl Pts',(2.29890939798744,6.36693576138702,50.6925341623944));
#21849=CARTESIAN_POINT('Ctrl Pts',(2.13298918365071,6.42204376677932,50.700734405676));
#21850=CARTESIAN_POINT('Ctrl Pts',(1.96706474179028,6.47715317628262,50.7089348578937));
#21851=CARTESIAN_POINT('Ctrl Pts',(1.79900733918795,6.52582666653708,50.7171353101114));
#21852=CARTESIAN_POINT('Ctrl Pts',(1.62935819918338,6.5679129758816,50.7253357623291));
#21853=CARTESIAN_POINT('Ctrl Pts',(1.45967399289318,6.61000798441873,50.7335379095711));
#21854=CARTESIAN_POINT('Ctrl Pts',(1.28839774159573,6.64551301394018,50.741740056813));
#21855=CARTESIAN_POINT('Ctrl Pts',(1.11608211499278,6.67432765996645,50.7499422040549));
#21856=CARTESIAN_POINT('Ctrl Pts',(0.943531307150705,6.70318163303631,50.7581555458193));
#21857=CARTESIAN_POINT('Ctrl Pts',(0.769938641694908,6.72532690243689,50.7663688875837));
#21858=CARTESIAN_POINT('Ctrl Pts',(0.595864882246309,6.74071465366289,50.7745822293481));
#21859=CARTESIAN_POINT('Ctrl Pts',(0.421786699118565,6.75610279593274,50.7827957798354));
#21860=CARTESIAN_POINT('Ctrl Pts',(0.247227757010974,6.76473308307763,50.7910093303228));
#21861=CARTESIAN_POINT('Ctrl Pts',(0.0727493048034127,6.76660893939133,
50.7992228808101));
#21862=CARTESIAN_POINT('Ctrl Pts',(-0.101971380471242,6.76848740000614,
50.8074478343876));
#21863=CARTESIAN_POINT('Ctrl Pts',(-0.276610994058523,6.76359269692049,
50.8156727879652));
#21864=CARTESIAN_POINT('Ctrl Pts',(-0.450610895119438,6.75198036291573,
50.8238977415427));
#21865=CARTESIAN_POINT('Ctrl Pts',(-0.624115081960255,6.7404011116832,50.832099262771));
#21866=CARTESIAN_POINT('Ctrl Pts',(-0.79698285563322,6.72214256066124,50.8403007839993));
#21867=CARTESIAN_POINT('Ctrl Pts',(-0.968670483191178,6.69731039261241,
50.8485023052276));
#21868=CARTESIAN_POINT('Ctrl Pts',(-1.14966196433778,6.67113255476139,50.8571482717184));
#21869=CARTESIAN_POINT('Ctrl Pts',(-1.32975286856129,6.63759031909408,50.8657942382093));
#21870=CARTESIAN_POINT('Ctrl Pts',(-1.50833518579757,6.59675783755058,50.8744402047002));
#21871=CARTESIAN_POINT('Ctrl Pts',(-1.68668907197277,6.55597758630193,50.8830751118246));
#21872=CARTESIAN_POINT('Ctrl Pts',(-1.86353792321638,6.50792575185398,50.8917100189489));
#21873=CARTESIAN_POINT('Ctrl Pts',(-2.03828166633691,6.45272786104255,50.9003449260733));
#21874=CARTESIAN_POINT('Ctrl Pts',(-2.21882676069068,6.39569744480726,50.9092665051448));
#21875=CARTESIAN_POINT('Ctrl Pts',(-2.3971242476004,6.33103834858026,50.9181880842163));
#21876=CARTESIAN_POINT('Ctrl Pts',(-2.57252375267655,6.25894644024975,50.9271096632879));
#21877=CARTESIAN_POINT('Ctrl Pts',(-2.74181838879493,6.18936372744451,50.9357207222635));
#21878=CARTESIAN_POINT('Ctrl Pts',(-2.90841303997573,6.11285698168042,50.9443317812392));
#21879=CARTESIAN_POINT('Ctrl Pts',(-3.07173784346953,6.0296530265843,50.9529428402149));
#21880=CARTESIAN_POINT('Ctrl Pts',(-3.23490862413441,5.9465275366586,50.9615457785645));
#21881=CARTESIAN_POINT('Ctrl Pts',(-3.39481543420343,5.85671756737965,50.970148716914));
#21882=CARTESIAN_POINT('Ctrl Pts',(-3.55090909497626,5.76049768676413,50.9787516552636));
#21883=CARTESIAN_POINT('Ctrl Pts',(-3.7068279669575,5.66438555015677,50.9873449603123));
#21884=CARTESIAN_POINT('Ctrl Pts',(-3.85894194881801,5.56187798104296,50.995938265361));
#21885=CARTESIAN_POINT('Ctrl Pts',(-4.00672696246917,5.45329515506199,51.0045315704097));
#21886=CARTESIAN_POINT('Ctrl Pts',(-4.02319263198647,5.44119725092621,51.0054890052503));
#21887=CARTESIAN_POINT('Ctrl Pts',(-4.03960458966874,5.42902397727664,51.0064464400909));
#21888=CARTESIAN_POINT('Ctrl Pts',(-4.05596213087828,5.4167758115766,51.0074038749316));
#21889=CARTESIAN_POINT('Ctrl Pts',(-4.20281855634457,5.30681296262605,51.0159996324792));
#21890=CARTESIAN_POINT('Ctrl Pts',(-4.34511433100738,5.19093896239823,51.0245953900268));
#21891=CARTESIAN_POINT('Ctrl Pts',(-4.48239025425366,5.06956276305677,51.0331911475744));
#21892=CARTESIAN_POINT('Ctrl Pts',(-4.61979426060219,4.94807331559589,51.041794925256));
#21893=CARTESIAN_POINT('Ctrl Pts',(-4.75216883799272,4.82107162412226,51.0503987029375));
#21894=CARTESIAN_POINT('Ctrl Pts',(-4.87909141508808,4.68900372821496,51.0590024806191));
#21895=CARTESIAN_POINT('Ctrl Pts',(-5.01100216045051,4.55174544851197,51.0679443942871));
#21896=CARTESIAN_POINT('Ctrl Pts',(-5.1370234511554,4.40901497961087,51.0768863079551));
#21897=CARTESIAN_POINT('Ctrl Pts',(-5.25672760455551,4.2613500080965,51.0858282216231));
#21898=CARTESIAN_POINT('Ctrl Pts',(-5.37221876109697,4.11888211657855,51.0944554239538));
#21899=CARTESIAN_POINT('Ctrl Pts',(-5.48182972798825,3.97182141005477,51.1030826262846));
#21900=CARTESIAN_POINT('Ctrl Pts',(-5.58522098140526,3.82067999037744,51.1117098286153));
#21901=CARTESIAN_POINT('Ctrl Pts',(-5.68871069916511,3.66939463163297,51.1203452470357));
#21902=CARTESIAN_POINT('Ctrl Pts',(-5.78596871565353,3.5140210591272,51.1289806654561));
#21903=CARTESIAN_POINT('Ctrl Pts',(-5.8767006022561,3.35509746973807,51.1376160838765));
#21904=CARTESIAN_POINT('Ctrl Pts',(-5.96756653229802,3.1959390933814,51.1462642598976));
#21905=CARTESIAN_POINT('Ctrl Pts',(-6.05188692151583,3.03322048828594,51.1549124359188));
#21906=CARTESIAN_POINT('Ctrl Pts',(-6.12941409520859,2.86750272004374,51.16356061194));
#21907=CARTESIAN_POINT('Ctrl Pts',(-6.13761617622538,2.84997040851603,51.1644755561717));
#21908=CARTESIAN_POINT('Ctrl Pts',(-6.14574226703425,2.8324045443392,51.1653905004034));
#21909=CARTESIAN_POINT('Ctrl Pts',(-6.15379210651178,2.81480580321864,51.1663054446351));
#21910=CARTESIAN_POINT('Ctrl Pts',(-6.23137319601528,2.64519627077582,51.175123306225));
#21911=CARTESIAN_POINT('Ctrl Pts',(-6.30201094808761,2.47221860160181,51.1839411678148));
#21912=CARTESIAN_POINT('Ctrl Pts',(-6.36542467166714,2.29644458877878,51.1927590294046));
#21913=CARTESIAN_POINT('Ctrl Pts',(-6.43138349855206,2.11361590394177,51.2019307949668));
#21914=CARTESIAN_POINT('Ctrl Pts',(-6.48952626910946,1.92776199853278,51.211102560529));
#21915=CARTESIAN_POINT('Ctrl Pts',(-6.539590179954,1.73955433322712,51.2202743260912));
#21916=CARTESIAN_POINT('Ctrl Pts',(-6.587510676453,1.5594045084487,51.2290534157008));
#21917=CARTESIAN_POINT('Ctrl Pts',(-6.62802949287413,1.37709857063926,51.2378325053105));
#21918=CARTESIAN_POINT('Ctrl Pts',(-6.66096483337967,1.1932461977645,51.2466115949201));
#21919=CARTESIAN_POINT('Ctrl Pts',(-6.69384701086094,1.00969059267806,51.2553765136438));
#21920=CARTESIAN_POINT('Ctrl Pts',(-6.71917007219714,0.824593800378376,
51.2641414323675));
#21921=CARTESIAN_POINT('Ctrl Pts',(-6.73680234476203,0.638579022211728,
51.2729063510912));
#21922=CARTESIAN_POINT('Ctrl Pts',(-6.75439619629057,0.452969573563714,
51.2816521709007));
#21923=CARTESIAN_POINT('Ctrl Pts',(-6.76433266229265,0.266446403454901,
51.2903979907102));
#21924=CARTESIAN_POINT('Ctrl Pts',(-6.76653133397799,0.0796411093222789,
51.2991438105197));
#21925=CARTESIAN_POINT('Ctrl Pts',(-6.76683941292852,0.0534658602596612,
51.3003692790635));
#21926=CARTESIAN_POINT('Ctrl Pts',(-6.76699565200429,0.0272850882396232,
51.3015947476073));
#21927=CARTESIAN_POINT('Ctrl Pts',(-6.76699991050681,0.00110054571902172,
51.3028202161511));
#21928=CARTESIAN_POINT('Ctrl Pts',(-6.76699991050694,0.0011005448889491,
51.3028202161899));
#21929=CARTESIAN_POINT('Ctrl Pts',(-6.7670293195252,-0.179728811491938,
51.3112832507402));
#21930=CARTESIAN_POINT('Ctrl Pts',(-6.75980613686487,-0.360470594821842,
51.3197462852904));
#21931=CARTESIAN_POINT('Ctrl Pts',(-6.74537751872907,-0.540528565225264,
51.3282093198407));
#21932=CARTESIAN_POINT('Ctrl Pts',(-6.73093802421214,-0.720722264434683,
51.3366787338785));
#21933=CARTESIAN_POINT('Ctrl Pts',(-6.70928228373777,-0.900230799662108,
51.3451481479163));
#21934=CARTESIAN_POINT('Ctrl Pts',(-6.68050916102434,-1.07846481141938,
51.3536175619541));
#21935=CARTESIAN_POINT('Ctrl Pts',(-6.65171094590499,-1.25685425712857,
51.3620943619812));
#21936=CARTESIAN_POINT('Ctrl Pts',(-6.61578301640392,-1.43396664259712,
51.3705711620082));
#21937=CARTESIAN_POINT('Ctrl Pts',(-6.57287508846235,-1.60922405881562,
51.3790479620353));
#21938=CARTESIAN_POINT('Ctrl Pts',(-6.52855870350362,-1.79023431721328,
51.3878030138692));
#21939=CARTESIAN_POINT('Ctrl Pts',(-6.4767964103259,-1.96926538920702,51.3965580657032));
#21940=CARTESIAN_POINT('Ctrl Pts',(-6.41780797571549,-2.14570030219569,
51.4053131175372));
#21941=CARTESIAN_POINT('Ctrl Pts',(-6.36053538499355,-2.31700311142258,
51.4138135041595));
#21942=CARTESIAN_POINT('Ctrl Pts',(-6.29645132653337,-2.48585841071289,
51.4223138907819));
#21943=CARTESIAN_POINT('Ctrl Pts',(-6.22580501065645,-2.65172415030015,
51.4308142774042));
#21944=CARTESIAN_POINT('Ctrl Pts',(-6.15198392877506,-2.82504370973367,
51.439696661844));
#21945=CARTESIAN_POINT('Ctrl Pts',(-6.07099737519763,-2.99509844173543,
51.4485790462838));
#21946=CARTESIAN_POINT('Ctrl Pts',(-5.98318190989025,-3.16130087672182,
51.4574614307236));
#21947=CARTESIAN_POINT('Ctrl Pts',(-5.89536644458283,-3.32750331170826,
51.4663438151633));
#21948=CARTESIAN_POINT('Ctrl Pts',(-5.80072232668789,-3.48985314242165,
51.4752261996031));
#21949=CARTESIAN_POINT('Ctrl Pts',(-5.69963587399677,-3.64779932340708,
51.4841085840429));
#21950=CARTESIAN_POINT('Ctrl Pts',(-5.60682224202642,-3.79281933670102,
51.4922640424497));
#21951=CARTESIAN_POINT('Ctrl Pts',(-5.50831883497746,-3.93453128983594,
51.5004195008565));
#21952=CARTESIAN_POINT('Ctrl Pts',(-5.40438862416666,-4.07245289708525,
51.5085749592633));
#21953=CARTESIAN_POINT('Ctrl Pts',(-5.30058491008398,-4.21020663560882,
51.5167204914052));
#21954=CARTESIAN_POINT('Ctrl Pts',(-5.19136775760629,-4.34417892263188,
51.5248660235471));
#21955=CARTESIAN_POINT('Ctrl Pts',(-5.0770451485939,-4.47391345011716,51.5330115556889));
#21956=CARTESIAN_POINT('Ctrl Pts',(-4.96283764547294,-4.60351735419761,
51.5411488864895));
#21957=CARTESIAN_POINT('Ctrl Pts',(-4.84353515935554,-4.7288917209991,51.54928621729));
#21958=CARTESIAN_POINT('Ctrl Pts',(-4.71948794390356,-4.84961055625593,
51.5574235480906));
#21959=CARTESIAN_POINT('Ctrl Pts',(-4.59553955667126,-4.9702332150083,51.5655543958926));
#21960=CARTESIAN_POINT('Ctrl Pts',(-4.46685422751048,-5.08620747368003,
51.5736852436946));
#21961=CARTESIAN_POINT('Ctrl Pts',(-4.33382132026465,-5.19714169173976,
51.5818160914966));
#21962=CARTESIAN_POINT('Ctrl Pts',(-4.20086645426036,-5.30801083233643,
51.5899421694904));
#21963=CARTESIAN_POINT('Ctrl Pts',(-4.06356936929772,-5.41384558692698,
51.5980682474842));
#21964=CARTESIAN_POINT('Ctrl Pts',(-3.92235498716737,-5.5142923711609,51.6061943254779));
#21965=CARTESIAN_POINT('Ctrl Pts',(-3.7806398846293,-5.61509532134616,51.6143492170601));
#21966=CARTESIAN_POINT('Ctrl Pts',(-3.63497992465894,-5.71047176661043,
51.6225041086423));
#21967=CARTESIAN_POINT('Ctrl Pts',(-3.48583713478017,-5.80010590160107,
51.6306590002245));
#21968=CARTESIAN_POINT('Ctrl Pts',(-3.33727594963583,-5.88939049480482,
51.6387820905808));
#21969=CARTESIAN_POINT('Ctrl Pts',(-3.18525937398488,-5.97297730829069,
51.6469051809371));
#21970=CARTESIAN_POINT('Ctrl Pts',(-3.03027176795098,-6.05059848381623,
51.6550282712934));
#21971=CARTESIAN_POINT('Ctrl Pts',(-2.87527199158271,-6.12822575451082,
51.6631519995118));
#21972=CARTESIAN_POINT('Ctrl Pts',(-2.71730104721002,-6.19988629028897,
51.6712757277303));
#21973=CARTESIAN_POINT('Ctrl Pts',(-2.55686628275255,-6.26535903297833,
51.6793994559487));
#21974=CARTESIAN_POINT('Ctrl Pts',(-2.39638839770137,-6.33084937299796,
51.687525367609));
#21975=CARTESIAN_POINT('Ctrl Pts',(-2.23344571254812,-6.39014847019056,
51.6956512792693));
#21976=CARTESIAN_POINT('Ctrl Pts',(-2.06856381296008,-6.44308410248633,
51.7037771909296));
#21977=CARTESIAN_POINT('Ctrl Pts',(-1.90262747648431,-6.49635826365341,
51.7119550686397));
#21978=CARTESIAN_POINT('Ctrl Pts',(-1.73472739414795,-6.54318717256633,
51.7201329463498));
#21979=CARTESIAN_POINT('Ctrl Pts',(-1.56541213514596,-6.5834469578738,51.7283108240599));
#21980=CARTESIAN_POINT('Ctrl Pts',(-1.39690498115332,-6.62351459195772,
51.7364496705333));
#21981=CARTESIAN_POINT('Ctrl Pts',(-1.22699650039423,-6.65707566049365,
51.7445885170068));
#21982=CARTESIAN_POINT('Ctrl Pts',(-1.05623464916449,-6.6840599463129,51.7527273634802));
#21983=CARTESIAN_POINT('Ctrl Pts',(-0.884244421238745,-6.71123834380065,
51.7609247568086));
#21984=CARTESIAN_POINT('Ctrl Pts',(-0.711388874229226,-6.73174493705477,
51.769122150137));
#21985=CARTESIAN_POINT('Ctrl Pts',(-0.538229598620791,-6.74556134796568,
51.7773195434654));
#21986=CARTESIAN_POINT('Ctrl Pts',(-0.365070323012357,-6.75937775887658,
51.7855169367938));
#21987=CARTESIAN_POINT('Ctrl Pts',(-0.19160769323252,-6.76650403322454,
51.7937143301222));
#21988=CARTESIAN_POINT('Ctrl Pts',(-0.0183993852529096,-6.76697498610881,
51.8019117234507));
#21989=CARTESIAN_POINT('Ctrl Pts',(0.155417795802133,-6.7674475945172,51.8101379327876));
#21990=CARTESIAN_POINT('Ctrl Pts',(0.329496174290599,-6.76121953317085,
51.8183641421246));
#21991=CARTESIAN_POINT('Ctrl Pts',(0.50327859407008,-6.74825900931128,51.8265903514616));
#21992=CARTESIAN_POINT('Ctrl Pts',(0.676865776745864,-6.73531304604503,
51.8348073190048));
#21993=CARTESIAN_POINT('Ctrl Pts',(0.850157308409486,-6.71564970794485,
51.843024286548));
#21994=CARTESIAN_POINT('Ctrl Pts',(1.02259445868563,-6.68928916799576,51.8512412540912));
#21995=CARTESIAN_POINT('Ctrl Pts',(1.19487249272749,-6.66295295221258,51.8594506394346));
#21996=CARTESIAN_POINT('Ctrl Pts',(1.36629736317955,-6.62993189581132,51.8676600247779));
#21997=CARTESIAN_POINT('Ctrl Pts',(1.53631380092767,-6.59029808924294,51.8758694101213));
#21998=CARTESIAN_POINT('Ctrl Pts',(1.70620746886125,-6.55069290246655,51.8840728674219));
#21999=CARTESIAN_POINT('Ctrl Pts',(1.87469438199783,-6.50448455780097,51.8922763247225));
#22000=CARTESIAN_POINT('Ctrl Pts',(2.04122773926517,-6.45179651852524,51.9004797820231));
#22001=CARTESIAN_POINT('Ctrl Pts',(2.207674248052,-6.39913595648427,51.9086789611549));
#22002=CARTESIAN_POINT('Ctrl Pts',(2.37216888947289,-6.34000253974969,51.9168781402868));
#22003=CARTESIAN_POINT('Ctrl Pts',(2.53417825948068,-6.27457006887129,51.9250773194186));
#22004=CARTESIAN_POINT('Ctrl Pts',(2.69615710343171,-6.20914992688054,51.9332749536484));
#22005=CARTESIAN_POINT('Ctrl Pts',(2.85565127420781,-6.13743322328416,51.9414725878783));
#22006=CARTESIAN_POINT('Ctrl Pts',(3.01214536417536,-6.05964267140208,51.9496702221081));
#22007=CARTESIAN_POINT('Ctrl Pts',(3.16862815822796,-5.9818577345273,51.9578672646236));
#22008=CARTESIAN_POINT('Ctrl Pts',(3.32211098116247,-5.89799998136302,51.9660643071392));
#22009=CARTESIAN_POINT('Ctrl Pts',(3.47210119730316,-5.80833902898978,51.9742613496548));
#22010=CARTESIAN_POINT('Ctrl Pts',(3.62210784745626,-5.71866825271441,51.9824592902976));
#22011=CARTESIAN_POINT('Ctrl Pts',(3.76862082048467,-5.6231931945263,51.9906572309405));
#22012=CARTESIAN_POINT('Ctrl Pts',(3.91117470277814,-5.52222794208536,51.9988551715833));
#22013=CARTESIAN_POINT('Ctrl Pts',(4.05377011333156,-5.42123327682745,52.0070555004193));
#22014=CARTESIAN_POINT('Ctrl Pts',(4.19240384319343,-5.31474543879705,52.0152558292553));
#22015=CARTESIAN_POINT('Ctrl Pts',(4.3266418856865,-5.20312012094889,52.0234561580913));
#22016=CARTESIAN_POINT('Ctrl Pts',(4.46101980770262,-5.09137848662344,52.0316650318827));
#22017=CARTESIAN_POINT('Ctrl Pts',(4.59099261521088,-4.97448890685478,52.0398739056741));
#22018=CARTESIAN_POINT('Ctrl Pts',(4.71616091591607,-4.85284609432297,52.0480827794655));
#22019=CARTESIAN_POINT('Ctrl Pts',(4.84139639306712,-4.73113799743591,52.0562960588689));
#22020=CARTESIAN_POINT('Ctrl Pts',(4.96182197592798,-4.60467184176375,52.0645093382723));
#22021=CARTESIAN_POINT('Ctrl Pts',(5.07707730261945,-4.47387696111844,52.0727226176757));
#22022=CARTESIAN_POINT('Ctrl Pts',(5.19250120834156,-4.3428907724024,52.0809479102911));
#22023=CARTESIAN_POINT('Ctrl Pts',(5.30273951858665,-4.20756348381302,52.0891732029066));
#22024=CARTESIAN_POINT('Ctrl Pts',(5.40747332910717,-4.06835608016243,52.097398495522));
#22025=CARTESIAN_POINT('Ctrl Pts',(5.50219247963385,-3.94245970577029,52.1048372846341));
#22026=CARTESIAN_POINT('Ctrl Pts',(5.5924099379874,-3.81339031464735,52.1122760737462));
#22027=CARTESIAN_POINT('Ctrl Pts',(5.67792195915921,-3.68150665158949,52.1197148628583));
#22028=CARTESIAN_POINT('Ctrl Pts',(5.77248561260963,-3.53566281772527,52.1279410638772));
#22029=CARTESIAN_POINT('Ctrl Pts',(5.86155858299504,-3.38596933453658,52.136167264896));
#22030=CARTESIAN_POINT('Ctrl Pts',(5.94481231055862,-3.23287729309831,52.1443934659149));
#22031=CARTESIAN_POINT('Ctrl Pts',(6.02797252010593,-3.07995721830275,52.1526104265306));
#22032=CARTESIAN_POINT('Ctrl Pts',(6.10532633338411,-2.92364649926657,52.1608273871464));
#22033=CARTESIAN_POINT('Ctrl Pts',(6.17658801737508,-2.76442570231478,52.1690443477622));
#22034=CARTESIAN_POINT('Ctrl Pts',(6.24778395666923,-2.60535179949229,52.1772537275638));
#22035=CARTESIAN_POINT('Ctrl Pts',(6.31289881449309,-2.44337349088994,52.1854631073653));
#22036=CARTESIAN_POINT('Ctrl Pts',(6.3716923719208,-2.27899655936693,52.1936724871669));
#22037=CARTESIAN_POINT('Ctrl Pts',(6.43044348405991,-2.11473829775612,52.2018759403073));
#22038=CARTESIAN_POINT('Ctrl Pts',(6.4828822653894,-1.9480851987053,52.2100793934477));
#22039=CARTESIAN_POINT('Ctrl Pts',(6.52881626566073,-1.77956375812836,52.2182828465881));
#22040=CARTESIAN_POINT('Ctrl Pts',(6.57472631868904,-1.61113017456074,52.2264820229382));
#22041=CARTESIAN_POINT('Ctrl Pts',(6.61413825245348,-1.44083053512187,52.2346811992884));
#22042=CARTESIAN_POINT('Ctrl Pts',(6.64690918518168,-1.26920734474215,52.2428803756385));
#22043=CARTESIAN_POINT('Ctrl Pts',(6.67967395156445,-1.09761644785506,52.2510780091899));
#22044=CARTESIAN_POINT('Ctrl Pts',(6.70580013268361,-0.924702846842289,
52.2592756427412));
#22045=CARTESIAN_POINT('Ctrl Pts',(6.72519570953941,-0.751020418093132,
52.2674732762926));
#22046=CARTESIAN_POINT('Ctrl Pts',(6.74458988943764,-0.577350498741494,
52.2756703194132));
#22047=CARTESIAN_POINT('Ctrl Pts',(6.75725438983026,-0.402912218299536,
52.2838673625338));
#22048=CARTESIAN_POINT('Ctrl Pts',(6.76314895297657,-0.228265722025817,
52.2920644056544));
#22049=CARTESIAN_POINT('Ctrl Pts',(6.76904416289669,-0.0536000628765411,
52.3002623481856));
#22050=CARTESIAN_POINT('Ctrl Pts',(6.76816794355004,0.1212734990702,52.3084602907168));
#22051=CARTESIAN_POINT('Ctrl Pts',(6.76053216405729,0.295793608360497,52.316658233248));
#22052=CARTESIAN_POINT('Ctrl Pts',(6.75289415894258,0.470364585513826,52.3248585652564));
#22053=CARTESIAN_POINT('Ctrl Pts',(6.73849268490011,0.644581546556523,52.3330588972648));
#22054=CARTESIAN_POINT('Ctrl Pts',(6.71739159661993,0.817886995654062,52.3412592292732));
#22055=CARTESIAN_POINT('Ctrl Pts',(6.69626851530248,0.991373075871156,52.3494681082439));
#22056=CARTESIAN_POINT('Ctrl Pts',(6.6684319125601,1.16394538958286,52.3576769872147));
#22057=CARTESIAN_POINT('Ctrl Pts',(6.63399719299451,1.33505439714681,52.3658858661855));
#22058=CARTESIAN_POINT('Ctrl Pts',(6.59954398807276,1.50625525999478,52.3740991518728));
#22059=CARTESIAN_POINT('Ctrl Pts',(6.55848568943385,1.67599090241361,52.3823124375602));
#22060=CARTESIAN_POINT('Ctrl Pts',(6.51098794669323,1.84372583591367,52.3905257232476));
#22061=CARTESIAN_POINT('Ctrl Pts',(6.46342072060891,2.01170614494867,52.3987510239597));
#22062=CARTESIAN_POINT('Ctrl Pts',(6.40939533595326,2.17767955502114,52.4069763246718));
#22063=CARTESIAN_POINT('Ctrl Pts',(6.34912650578597,2.34112827788783,52.4152016253839));
#22064=CARTESIAN_POINT('Ctrl Pts',(6.29462061899694,2.48894793125848,52.4226404176779));
#22065=CARTESIAN_POINT('Ctrl Pts',(6.23500890614251,2.63470272676859,52.430079209972));
#22066=CARTESIAN_POINT('Ctrl Pts',(6.17048252953134,2.77802706119803,52.437518002266));
#22067=CARTESIAN_POINT('Ctrl Pts',(6.09974706525856,2.93514286205176,52.4456725966223));
#22068=CARTESIAN_POINT('Ctrl Pts',(6.02289617693403,3.08980105830553,52.4538271909787));
#22069=CARTESIAN_POINT('Ctrl Pts',(5.9401224555034,3.24148642039794,52.461981785335));
#22070=CARTESIAN_POINT('Ctrl Pts',(5.85747523226454,3.39293997070648,52.4701239175062));
#22071=CARTESIAN_POINT('Ctrl Pts',(5.76892338489564,3.54142942142937,52.4782660496774));
#22072=CARTESIAN_POINT('Ctrl Pts',(5.67470749145207,3.68645953273026,52.4864081818485));
#22073=CARTESIAN_POINT('Ctrl Pts',(5.58057537657762,3.83136068049049,52.4945430738805));
#22074=CARTESIAN_POINT('Ctrl Pts',(5.48078943761993,3.97280830693704,52.5026779659125));
#22075=CARTESIAN_POINT('Ctrl Pts',(5.37563639108518,4.11033117775693,52.5108128579445));
#22076=CARTESIAN_POINT('Ctrl Pts',(5.27055683700799,4.2477579325433,52.5189420644236));
#22077=CARTESIAN_POINT('Ctrl Pts',(5.16011786372585,4.38126510315289,52.5270712709028));
#22078=CARTESIAN_POINT('Ctrl Pts',(5.04464975887452,4.51040993816386,52.5352004773819));
#22079=CARTESIAN_POINT('Ctrl Pts',(4.92924038507035,4.63948908567258,52.5433255490671));
#22080=CARTESIAN_POINT('Ctrl Pts',(4.80880721628425,4.76421004385035,52.5514506207524));
#22081=CARTESIAN_POINT('Ctrl Pts',(4.68372110033272,4.88416273831023,52.5595756924376));
#22082=CARTESIAN_POINT('Ctrl Pts',(4.55865929744746,5.00409211749017,52.5676991848477));
#22083=CARTESIAN_POINT('Ctrl Pts',(4.42894660773446,5.11925482125234,52.5758226772577));
#22084=CARTESIAN_POINT('Ctrl Pts',(4.29499117035121,5.22927718204009,52.5839461696677));
#22085=CARTESIAN_POINT('Ctrl Pts',(4.16105365691941,5.3392848212496,52.5920685751111));
#22086=CARTESIAN_POINT('Ctrl Pts',(4.0228748111491,5.44415325782776,52.6001909805546));
#22087=CARTESIAN_POINT('Ctrl Pts',(3.8808961193363,5.54354889136196,52.608313385998));
#22088=CARTESIAN_POINT('Ctrl Pts',(3.73886862973991,5.64297868697044,52.6164385830954));
#22089=CARTESIAN_POINT('Ctrl Pts',(3.59303898458832,5.73693171154433,52.6245637801929));
#22090=CARTESIAN_POINT('Ctrl Pts',(3.4438782889268,5.82511728045527,52.6326889772903));
#22091=CARTESIAN_POINT('Ctrl Pts',(3.33081901237669,5.89195926305005,52.638847629887));
#22092=CARTESIAN_POINT('Ctrl Pts',(3.21584661904426,5.95548860693522,52.6450062824837));
#22093=CARTESIAN_POINT('Ctrl Pts',(3.09917575053253,6.01559628526642,52.6511649350805));
#22094=CARTESIAN_POINT('Origin',(0.,0.,-3.69717978381041));
#22095=CARTESIAN_POINT('',(3.09917575053258,6.01559628526639,55.0458595242204));
#22096=CARTESIAN_POINT('',(3.09917575053251,6.01559628526643,54.6513758699904));
#22097=CARTESIAN_POINT('',(3.09917575053259,6.01559628526639,-3.69717978381041));
#22098=CARTESIAN_POINT('',(-6.76699752191952,-0.00579122915657409,53.6971797837779));
#22099=CARTESIAN_POINT('Ctrl Pts',(-6.76699752191893,-0.00579122983738126,
53.69717978381));
#22100=CARTESIAN_POINT('Ctrl Pts',(-6.76677989625174,-0.260084772302621,
53.7091640693841));
#22101=CARTESIAN_POINT('Ctrl Pts',(-6.75222508869606,-0.513791481686647,
53.7211483549582));
#22102=CARTESIAN_POINT('Ctrl Pts',(-6.72355008369308,-0.765613004115478,
53.7331326405323));
#22103=CARTESIAN_POINT('Ctrl Pts',(-6.70444183559884,-0.933420058570815,
53.7411186444391));
#22104=CARTESIAN_POINT('Ctrl Pts',(-6.6790643925138,-1.10039086166875,53.7491046483459));
#22105=CARTESIAN_POINT('Ctrl Pts',(-6.64749262677839,-1.26614800751213,
53.7570906522527));
#22106=CARTESIAN_POINT('Ctrl Pts',(-6.61497661658581,-1.43686259753244,
53.7653155005748));
#22107=CARTESIAN_POINT('Ctrl Pts',(-6.57583454917597,-1.60656341094717,
53.7735403488968));
#22108=CARTESIAN_POINT('Ctrl Pts',(-6.53014070694439,-1.77469753690816,
53.7817651972189));
#22109=CARTESIAN_POINT('Ctrl Pts',(-6.4844983261104,-1.94264230656458,53.7899807825381));
#22110=CARTESIAN_POINT('Ctrl Pts',(-6.43231895666366,-2.10902355915417,
53.7981963678573));
#22111=CARTESIAN_POINT('Ctrl Pts',(-6.37372820420558,-2.27329667639628,
53.8064119531765));
#22112=CARTESIAN_POINT('Ctrl Pts',(-6.31519166587682,-2.43741779142559,
53.8146199365997));
#22113=CARTESIAN_POINT('Ctrl Pts',(-6.25025567892752,-2.59943432009761,
53.822827920023));
#22114=CARTESIAN_POINT('Ctrl Pts',(-6.17909617111013,-2.7588148738493,53.8310359034462));
#22115=CARTESIAN_POINT('Ctrl Pts',(-6.10798821456512,-2.91807996488083,
53.8392379406227));
#22116=CARTESIAN_POINT('Ctrl Pts',(-6.03066586312489,-3.07471255832712,
53.8474399777993));
#22117=CARTESIAN_POINT('Ctrl Pts',(-5.94735388331155,-3.22819931024387,
53.8556420149758));
#22118=CARTESIAN_POINT('Ctrl Pts',(-5.86408552880434,-3.38160569068759,
53.8638397572552));
#22119=CARTESIAN_POINT('Ctrl Pts',(-5.77483396487451,-3.53186919668161,
53.8720374995346));
#22120=CARTESIAN_POINT('Ctrl Pts',(-5.67987084575693,-3.67849917432647,
53.880235241814));
#22121=CARTESIAN_POINT('Ctrl Pts',(-5.58492578230503,-3.82510127270745,
53.8884314254284));
#22122=CARTESIAN_POINT('Ctrl Pts',(-5.48427151635331,-3.96807091461804,
53.8966276090427));
#22123=CARTESIAN_POINT('Ctrl Pts',(-5.37822431914769,-4.10694438395851,
53.9048237926571));
#22124=CARTESIAN_POINT('Ctrl Pts',(-5.27218492849548,-4.24580763027392,
53.913019372918));
#22125=CARTESIAN_POINT('Ctrl Pts',(-5.16075361427734,-4.3805750188078,53.9212149531789));
#22126=CARTESIAN_POINT('Ctrl Pts',(-5.04428838637792,-4.51081408118899,
53.9294105334398));
#22127=CARTESIAN_POINT('Ctrl Pts',(-4.92781054247369,-4.64106725161484,
53.9376070014805));
#22128=CARTESIAN_POINT('Ctrl Pts',(-4.80629793773614,-4.76679085107235,
53.9458034695212));
#22129=CARTESIAN_POINT('Ctrl Pts',(-4.68014708707251,-4.8875875688694,53.9539999375619));
#22130=CARTESIAN_POINT('Ctrl Pts',(-4.55395961946476,-5.00841934950307,
53.9621987847353));
#22131=CARTESIAN_POINT('Ctrl Pts',(-4.42313148335591,-5.12432115180538,
53.9703976319087));
#22132=CARTESIAN_POINT('Ctrl Pts',(-4.28809409074618,-5.23493439012446,
53.9785964790821));
#22133=CARTESIAN_POINT('Ctrl Pts',(-4.1529155709298,-5.34566323003388,53.9868038948481));
#22134=CARTESIAN_POINT('Ctrl Pts',(-4.01351928378293,-5.45109223592226,
53.9950113106141));
#22135=CARTESIAN_POINT('Ctrl Pts',(-3.87036839545008,-5.55090420413658,
54.0032187263801));
#22136=CARTESIAN_POINT('Ctrl Pts',(-3.72714078327598,-5.65076966805529,
54.0114305410322));
#22137=CARTESIAN_POINT('Ctrl Pts',(-3.58015486006431,-5.74501189923058,
54.0196423556844));
#22138=CARTESIAN_POINT('Ctrl Pts',(-3.42990038334897,-5.83335858320938,
54.0278541703365));
#22139=CARTESIAN_POINT('Ctrl Pts',(-3.27942463407448,-5.92183537111111,
54.0360780781341));
#22140=CARTESIAN_POINT('Ctrl Pts',(-3.12567102790622,-6.00439909114341,
54.0443019859317));
#22141=CARTESIAN_POINT('Ctrl Pts',(-2.96915255132073,-6.08082413221971,
54.0525258937293));
#22142=CARTESIAN_POINT('Ctrl Pts',(-2.82453236958644,-6.15143945873337,
54.0601246326527));
#22143=CARTESIAN_POINT('Ctrl Pts',(-2.67755213333043,-6.21681438246504,
54.0677233715761));
#22144=CARTESIAN_POINT('Ctrl Pts',(-2.52862869857054,-6.27680857639975,
54.0753221104995));
#22145=CARTESIAN_POINT('Ctrl Pts',(-2.36888215716391,-6.34116288706281,
54.0834730926737));
#22146=CARTESIAN_POINT('Ctrl Pts',(-2.20642631344928,-6.39951591725883,
54.091624074848));
#22147=CARTESIAN_POINT('Ctrl Pts',(-2.04175619711414,-6.45162930053688,
54.0997750570223));
#22148=CARTESIAN_POINT('Ctrl Pts',(-1.87727736038111,-6.50368214929027,
54.1079165710753));
#22149=CARTESIAN_POINT('Ctrl Pts',(-1.71058971603811,-6.54950966947025,
54.1160580851284));
#22150=CARTESIAN_POINT('Ctrl Pts',(-1.54220965914812,-6.5889208803286,54.1241995991814));
#22151=CARTESIAN_POINT('Ctrl Pts',(-1.37398975796036,-6.62829460497709,
54.1323333693845));
#22152=CARTESIAN_POINT('Ctrl Pts',(-1.20408100262226,-6.66126408753093,
54.1404671395875));
#22153=CARTESIAN_POINT('Ctrl Pts',(-1.0330163950658,-6.68768765176165,54.1486009097906));
#22154=CARTESIAN_POINT('Ctrl Pts',(-0.862078518229963,-6.71409164048003,
54.1567286542086));
#22155=CARTESIAN_POINT('Ctrl Pts',(-0.689986854089072,-6.73395931129053,
54.1648563986266));
#22156=CARTESIAN_POINT('Ctrl Pts',(-0.51728608276181,-6.74719972348388,
54.1729841430445));
#22157=CARTESIAN_POINT('Ctrl Pts',(-0.344676945247087,-6.76043311040781,
54.1811075749386));
#22158=CARTESIAN_POINT('Ctrl Pts',(-0.171459708007611,-6.76704621375931,
54.1892310068326));
#22159=CARTESIAN_POINT('Ctrl Pts',(0.00181431908837062,-6.76699975677894,
54.1973544387267));
#22160=CARTESIAN_POINT('Ctrl Pts',(0.176187528458872,-6.76695300509376,
54.2055294024775));
#22161=CARTESIAN_POINT('Ctrl Pts',(0.350617878930557,-6.76016185860829,
54.2137043662283));
#22162=CARTESIAN_POINT('Ctrl Pts',(0.524541422292644,-6.74663955583068,
54.2218793299792));
#22163=CARTESIAN_POINT('Ctrl Pts',(0.697329413745348,-6.73320554056402,
54.2300009191522));
#22164=CARTESIAN_POINT('Ctrl Pts',(0.869616829378833,-6.71312805834558,
54.2381225083252));
#22165=CARTESIAN_POINT('Ctrl Pts',(1.04085417149711,-6.68647228317572,54.2462440974982));
#22166=CARTESIAN_POINT('Ctrl Pts',(1.21211412045663,-6.65981298889682,54.2543667588876));
#22167=CARTESIAN_POINT('Ctrl Pts',(1.38232335810515,-6.62657372812762,54.2624894202769));
#22168=CARTESIAN_POINT('Ctrl Pts',(1.55094109439532,-6.58687108737645,54.2706120816663));
#22169=CARTESIAN_POINT('Ctrl Pts',(1.71961320148922,-6.54715564450533,54.2787373622085));
#22170=CARTESIAN_POINT('Ctrl Pts',(1.88669242926656,-6.500972755372,54.2868626427508));
#22171=CARTESIAN_POINT('Ctrl Pts',(2.05165174144156,-6.44848929066645,54.294987923293));
#22172=CARTESIAN_POINT('Ctrl Pts',(2.21840825109433,-6.39543402950303,54.3032017270808));
#22173=CARTESIAN_POINT('Ctrl Pts',(2.3829980164088,-6.33594021797138,54.3114155308686));
#22174=CARTESIAN_POINT('Ctrl Pts',(2.54489678858769,-6.27023040529103,54.3196293346564));
#22175=CARTESIAN_POINT('Ctrl Pts',(2.7053278537605,-6.20511629047262,54.3277686755115));
#22176=CARTESIAN_POINT('Ctrl Pts',(2.86311620993667,-6.13389862319921,54.3359080163667));
#22177=CARTESIAN_POINT('Ctrl Pts',(3.01777638448957,-6.05684032257885,54.3440473572218));
#22178=CARTESIAN_POINT('Ctrl Pts',(3.17455892687851,-5.97872456770946,54.3522983924759));
#22179=CARTESIAN_POINT('Ctrl Pts',(3.32812646607889,-5.89460690617624,54.36054942773));
#22180=CARTESIAN_POINT('Ctrl Pts',(3.47800386231351,-5.80480646824098,54.3688004629841));
#22181=CARTESIAN_POINT('Ctrl Pts',(3.62788125854819,-5.71500603030568,54.3770514982382));
#22182=CARTESIAN_POINT('Ctrl Pts',(3.77406822709501,-5.61952308203906,54.3853025334923));
#22183=CARTESIAN_POINT('Ctrl Pts',(3.91612491505882,-5.51871856952821,54.3935535687464));
#22184=CARTESIAN_POINT('Ctrl Pts',(4.05784995134361,-5.41814939958594,54.4017853407773));
#22185=CARTESIAN_POINT('Ctrl Pts',(4.19590651381752,-5.31196967080089,54.4100171128081));
#22186=CARTESIAN_POINT('Ctrl Pts',(4.32982117865205,-5.20047474379947,54.418248884839));
#22187=CARTESIAN_POINT('Ctrl Pts',(4.4635759359942,-5.08911295288297,54.4264708273114));
#22188=CARTESIAN_POINT('Ctrl Pts',(4.59319837135361,-4.97244882885405,54.4346927697838));
#22189=CARTESIAN_POINT('Ctrl Pts',(4.71824369305165,-4.85082111121182,54.4429147122562));
#22190=CARTESIAN_POINT('Ctrl Pts',(4.84316475206892,-4.72931426003662,54.4511284842461));
#22191=CARTESIAN_POINT('Ctrl Pts',(4.96351750059756,-4.60285388646279,54.459342256236));
#22192=CARTESIAN_POINT('Ctrl Pts',(5.07888986678513,-4.47181917356542,54.4675560282259));
#22193=CARTESIAN_POINT('Ctrl Pts',(5.1941706901766,-4.34088843083354,54.4757632829563));
#22194=CARTESIAN_POINT('Ctrl Pts',(5.30447876646133,-4.2053908457353,54.4839705376866));
#22195=CARTESIAN_POINT('Ctrl Pts',(5.40943852255572,-4.06574272067111,54.492177792417));
#22196=CARTESIAN_POINT('Ctrl Pts',(5.51433601428634,-3.92617743785032,54.500380178429));
#22197=CARTESIAN_POINT('Ctrl Pts',(5.61389129159109,-3.78246680569833,54.5085825644409));
#22198=CARTESIAN_POINT('Ctrl Pts',(5.70776871342452,-3.63506056538984,54.5167849504529));
#22199=CARTESIAN_POINT('Ctrl Pts',(5.80161811512457,-3.48769832226867,54.5249848882516));
#22200=CARTESIAN_POINT('Ctrl Pts',(5.88979284162434,-3.33664296798299,54.5331848260503));
#22201=CARTESIAN_POINT('Ctrl Pts',(5.97200015707509,-3.18237381900605,54.541384763849));
#22202=CARTESIAN_POINT('Ctrl Pts',(6.05419597782134,-3.02812624083786,54.5495835550848));
#22203=CARTESIAN_POINT('Ctrl Pts',(6.13042588011323,-2.87066607878234,54.5577823463206));
#22204=CARTESIAN_POINT('Ctrl Pts',(6.20044273888851,-2.710497895547,54.5659811375563));
#22205=CARTESIAN_POINT('Ctrl Pts',(6.27046250892149,-2.55032305261763,54.5741802696928));
#22206=CARTESIAN_POINT('Ctrl Pts',(6.33426857712661,-2.38744029259166,54.5823794018292));
#22207=CARTESIAN_POINT('Ctrl Pts',(6.39166166953295,-2.22237487886794,54.5905785339656));
#22208=CARTESIAN_POINT('Ctrl Pts',(6.4490675596751,-2.05727265821384,54.5987794943765));
#22209=CARTESIAN_POINT('Ctrl Pts',(6.50005750820112,-1.88998715298163,54.6069804547875));
#22210=CARTESIAN_POINT('Ctrl Pts',(6.54448186788967,-1.72105958085806,54.6151814151984));
#22211=CARTESIAN_POINT('Ctrl Pts',(6.58894786389753,-1.55197368293349,54.6233900618834));
#22212=CARTESIAN_POINT('Ctrl Pts',(6.62683588539739,-1.3812429903637,54.6315987085685));
#22213=CARTESIAN_POINT('Ctrl Pts',(6.65804706090852,-1.20942066078247,54.6398073552535));
#22214=CARTESIAN_POINT('Ctrl Pts',(6.68927313751141,-1.03751629839533,54.6480199209771));
#22215=CARTESIAN_POINT('Ctrl Pts',(6.7138159620467,-0.864519614543845,54.6562324867006));
#22216=CARTESIAN_POINT('Ctrl Pts',(6.73162850336684,-0.690989647288,54.6644450524241));
#22217=CARTESIAN_POINT('Ctrl Pts',(6.74946548606402,-0.517221571876593,
54.6726688869729));
#22218=CARTESIAN_POINT('Ctrl Pts',(6.76055370632946,-0.342919108470499,
54.6808927215216));
#22219=CARTESIAN_POINT('Ctrl Pts',(6.76489825762268,-0.16864330408773,54.6891165560704));
#22220=CARTESIAN_POINT('Ctrl Pts',(6.76889008301258,-0.00851662268189041,
54.6966727130446));
#22221=CARTESIAN_POINT('Ctrl Pts',(6.76718940853875,0.151587348590576,54.7042288700189));
#22222=CARTESIAN_POINT('Ctrl Pts',(6.75983876983123,0.311237539327512,54.7117850269931));
#22223=CARTESIAN_POINT('Ctrl Pts',(6.75142820477987,0.493908510937084,54.7204307450454));
#22224=CARTESIAN_POINT('Ctrl Pts',(6.73560133324951,0.676401735153858,54.7290764630978));
#22225=CARTESIAN_POINT('Ctrl Pts',(6.71237252634239,0.858104928085077,54.7377221811502));
#22226=CARTESIAN_POINT('Ctrl Pts',(6.68917354048944,1.03957485114661,54.7463567998625));
#22227=CARTESIAN_POINT('Ctrl Pts',(6.65859160637791,1.22025646429683,54.7549914185748));
#22228=CARTESIAN_POINT('Ctrl Pts',(6.62069299883697,1.39954035852889,54.7636260372871));
#22229=CARTESIAN_POINT('Ctrl Pts',(6.58145595970188,1.58515586344356,54.7725655971896));
#22230=CARTESIAN_POINT('Ctrl Pts',(6.53437600806887,1.76927280158388,54.781505157092));
#22231=CARTESIAN_POINT('Ctrl Pts',(6.4795853778515,1.95122072845004,54.7904447169945));
#22232=CARTESIAN_POINT('Ctrl Pts',(6.42681061886781,2.1264743794821,54.799055370265));
#22233=CARTESIAN_POINT('Ctrl Pts',(6.3668825032131,2.29971543155046,54.8076660235354));
#22234=CARTESIAN_POINT('Ctrl Pts',(6.29997117461289,2.47035467069948,54.8162766768059));
#22235=CARTESIAN_POINT('Ctrl Pts',(6.23312318206175,2.6408323883924,54.824879179517));
#22236=CARTESIAN_POINT('Ctrl Pts',(6.15930526625744,2.80871292030108,54.8334816822281));
#22237=CARTESIAN_POINT('Ctrl Pts',(6.0787371052689,2.97342297781985,54.8420841849391));
#22238=CARTESIAN_POINT('Ctrl Pts',(5.99825962212379,3.13794765748433,54.8506770057066));
#22239=CARTESIAN_POINT('Ctrl Pts',(5.91104718384051,3.29930870803239,54.859269826474));
#22240=CARTESIAN_POINT('Ctrl Pts',(5.81736730544237,3.45695337451494,54.8678626472414));
#22241=CARTESIAN_POINT('Ctrl Pts',(5.80632670625338,3.47553251452534,54.8688753501998));
#22242=CARTESIAN_POINT('Ctrl Pts',(5.79519633069773,3.49406005925568,54.8698880531582));
#22243=CARTESIAN_POINT('Ctrl Pts',(5.78397666006704,3.51253512378164,54.8709007561166));
#22244=CARTESIAN_POINT('Ctrl Pts',(5.68875035480715,3.6693411648995,54.8794960138767));
#22245=CARTESIAN_POINT('Ctrl Pts',(5.58719985117846,3.8221801252544,54.8880912716368));
#22246=CARTESIAN_POINT('Ctrl Pts',(5.47968778795488,3.97055547077964,54.8966865293968));
#22247=CARTESIAN_POINT('Ctrl Pts',(5.37207504424347,4.11906976352366,54.9052898362513));
#22248=CARTESIAN_POINT('Ctrl Pts',(5.25848977672164,4.26311185076452,54.9138931431057));
#22249=CARTESIAN_POINT('Ctrl Pts',(5.13933507636798,4.40221807420007,54.9224964499602));
#22250=CARTESIAN_POINT('Ctrl Pts',(5.015240180819,4.5470916898964,54.9314564529002));
#22251=CARTESIAN_POINT('Ctrl Pts',(4.88510444856113,4.68661115451239,54.9404164558401));
#22252=CARTESIAN_POINT('Ctrl Pts',(4.74942480987268,4.82029594271616,54.9493764587801));
#22253=CARTESIAN_POINT('Ctrl Pts',(4.6187901463701,4.94900993024758,54.9580033019849));
#22254=CARTESIAN_POINT('Ctrl Pts',(4.48301667055892,5.07231515410789,54.9666301451896));
#22255=CARTESIAN_POINT('Ctrl Pts',(4.34258132168731,5.18982431923591,54.9752569883944));
#22256=CARTESIAN_POINT('Ctrl Pts',(4.20201175212178,5.30744579342153,54.9838920766805));
#22257=CARTESIAN_POINT('Ctrl Pts',(4.05677165544218,5.41925996304238,54.9925271649667));
#22258=CARTESIAN_POINT('Ctrl Pts',(3.90736828990719,5.52492190415645,55.0011622532529));
#22259=CARTESIAN_POINT('Ctrl Pts',(3.75774303039178,5.63074077445756,55.009810166378));
#22260=CARTESIAN_POINT('Ctrl Pts',(3.60394239921484,5.73038898730998,55.0184580795032));
#22261=CARTESIAN_POINT('Ctrl Pts',(3.44650092837927,5.82356594799792,55.0271059926284));
#22262=CARTESIAN_POINT('Ctrl Pts',(3.42883839211303,5.83401898453647,55.0280761568322));
#22263=CARTESIAN_POINT('Ctrl Pts',(3.41113005765446,5.84439062630108,55.029046321036));
#22264=CARTESIAN_POINT('Ctrl Pts',(3.39337669691533,5.85468048597291,55.0300164852398));
#22265=CARTESIAN_POINT('Ctrl Pts',(3.29673766573511,5.91069253260895,55.0352974982333));
#22266=CARTESIAN_POINT('Ctrl Pts',(3.19862976534322,5.96435855979782,55.0405785112269));
#22267=CARTESIAN_POINT('Ctrl Pts',(3.09917575053258,6.01559628526639,55.0458595242204));
#22268=CARTESIAN_POINT('Ctrl Pts',(3.09917575053258,6.01559628526639,53.0455807084606));
#22269=CARTESIAN_POINT('Ctrl Pts',(2.94389790458265,6.09559389679854,53.0537979533555));
#22270=CARTESIAN_POINT('Ctrl Pts',(2.785645637837,6.16951112027455,53.0620151982504));
#22271=CARTESIAN_POINT('Ctrl Pts',(2.62494151830489,6.23714446084739,53.0702324431454));
#22272=CARTESIAN_POINT('Ctrl Pts',(2.46067861284263,6.30627553888669,53.078631658581));
#22273=CARTESIAN_POINT('Ctrl Pts',(2.29385438133757,6.3688410547015,53.0870308740166));
#22274=CARTESIAN_POINT('Ctrl Pts',(2.12504217396318,6.42467779416819,53.0954300894522));
#22275=CARTESIAN_POINT('Ctrl Pts',(1.95622996658878,6.48051453363488,53.1038293048877));
#22276=CARTESIAN_POINT('Ctrl Pts',(1.78543017853457,6.5296224489739,53.1122285203233));
#22277=CARTESIAN_POINT('Ctrl Pts',(1.61322576824907,6.57189406645126,53.1206277357589));
#22278=CARTESIAN_POINT('Ctrl Pts',(1.44605108355753,6.61293101963649,53.1287816279257));
#22279=CARTESIAN_POINT('Ctrl Pts',(1.27703569613876,6.64765218906878,53.1369355200924));
#22280=CARTESIAN_POINT('Ctrl Pts',(1.10670232505557,6.6758893762342,53.1450894122591));
#22281=CARTESIAN_POINT('Ctrl Pts',(0.936576808273544,6.70409210614225,53.1532333543993));
#22282=CARTESIAN_POINT('Ctrl Pts',(0.765136865949179,6.72582654422594,53.1613772965395));
#22283=CARTESIAN_POINT('Ctrl Pts',(0.592919935417015,6.74097433240812,53.1695212386797));
#22284=CARTESIAN_POINT('Ctrl Pts',(0.420876909425892,6.75610682436395,53.1776569570726));
#22285=CARTESIAN_POINT('Ctrl Pts',(0.248058818721434,6.76466587584156,53.1857926754655));
#22286=CARTESIAN_POINT('Ctrl Pts',(0.0750128443173994,6.76658422493856,
53.1939283938584));
#22287=CARTESIAN_POINT('Ctrl Pts',(-0.0978947886393597,6.76850104041312,
53.2020576081586));
#22288=CARTESIAN_POINT('Ctrl Pts',(-0.271029578634426,6.76378772005493,
53.2101868224589));
#22289=CARTESIAN_POINT('Ctrl Pts',(-0.443839678090963,6.75242884747052,
53.2183160367591));
#22290=CARTESIAN_POINT('Ctrl Pts',(-0.616547960138858,6.74107666738254,
53.2264404614345));
#22291=CARTESIAN_POINT('Ctrl Pts',(-0.788931568674309,6.72308675649276,
53.2345648861099));
#22292=CARTESIAN_POINT('Ctrl Pts',(-0.960439117220119,6.69849577906215,
53.2426893107854));
#22293=CARTESIAN_POINT('Ctrl Pts',(-1.13298782637896,6.67375551865623,53.2508630559196));
#22294=CARTESIAN_POINT('Ctrl Pts',(-1.30464942893307,6.6423337798946,53.2590368010538));
#22295=CARTESIAN_POINT('Ctrl Pts',(-1.47486751946542,6.60432091891558,53.2672105461879));
#22296=CARTESIAN_POINT('Ctrl Pts',(-1.64399558315513,6.56655148117496,53.2753319490501));
#22297=CARTESIAN_POINT('Ctrl Pts',(-1.81169821212646,6.5222751928793,53.2834533519123));
#22298=CARTESIAN_POINT('Ctrl Pts',(-1.97744006838208,6.47163192525325,53.2915747547744));
#22299=CARTESIAN_POINT('Ctrl Pts',(-2.14319473892537,6.42098474215639,53.2996967855407));
#22300=CARTESIAN_POINT('Ctrl Pts',(-2.30698798475606,6.36396970609436,53.3078188163069));
#22301=CARTESIAN_POINT('Ctrl Pts',(-2.4683000816797,6.30077643681951,53.3159408470732));
#22302=CARTESIAN_POINT('Ctrl Pts',(-2.62965536795347,6.23756624831614,53.3240650524143));
#22303=CARTESIAN_POINT('Ctrl Pts',(-2.78852784195636,6.16817466633816,53.3321892577554));
#22304=CARTESIAN_POINT('Ctrl Pts',(-2.94441823979469,6.09283925843809,53.3403134630965));
#22305=CARTESIAN_POINT('Ctrl Pts',(-3.10199604332251,6.01668839687522,53.348525607339));
#22306=CARTESIAN_POINT('Ctrl Pts',(-3.25652648989856,5.93446444821664,53.3567377515815));
#22307=CARTESIAN_POINT('Ctrl Pts',(-3.40752067337968,5.84645977156177,53.3649498958239));
#22308=CARTESIAN_POINT('Ctrl Pts',(-3.55713644638242,5.75925848061124,53.3730870722404));
#22309=CARTESIAN_POINT('Ctrl Pts',(-3.70327997723185,5.6663818151341,53.3812242486569));
#22310=CARTESIAN_POINT('Ctrl Pts',(-3.84550626848677,5.56815683498848,53.3893614250733));
#22311=CARTESIAN_POINT('Ctrl Pts',(-3.98969805648939,5.46857443437359,53.3976110532288));
#22312=CARTESIAN_POINT('Ctrl Pts',(-4.12986322942873,5.36349504988159,53.4058606813842));
#22313=CARTESIAN_POINT('Ctrl Pts',(-4.26557448679539,5.25330022915122,53.4141103095397));
#22314=CARTESIAN_POINT('Ctrl Pts',(-4.4012857441621,5.14310540842081,53.4223599376951));
#22315=CARTESIAN_POINT('Ctrl Pts',(-4.53254283863639,5.02779545292852,53.4306095658506));
#22316=CARTESIAN_POINT('Ctrl Pts',(-4.6589590763726,4.90778863895802,53.4388591940061));
#22317=CARTESIAN_POINT('Ctrl Pts',(-4.783286477857,4.78976475525007,53.4469725095907));
#22318=CARTESIAN_POINT('Ctrl Pts',(-4.90332457913685,4.66682505072133,53.4550858251754));
#22319=CARTESIAN_POINT('Ctrl Pts',(-5.01865373847193,4.53931753166946,53.4631991407601));
#22320=CARTESIAN_POINT('Ctrl Pts',(-5.13385069024837,4.41195618083645,53.4713031556471));
#22321=CARTESIAN_POINT('Ctrl Pts',(-5.24434919911163,4.28003770958282,53.479407170534));
#22322=CARTESIAN_POINT('Ctrl Pts',(-5.34976387157572,4.14394926590363,53.487511185421));
#22323=CARTESIAN_POINT('Ctrl Pts',(-5.45508038457376,4.00798754432729,53.4956076540551));
#22324=CARTESIAN_POINT('Ctrl Pts',(-5.55532226046852,3.86786387087928,53.5037041226892));
#22325=CARTESIAN_POINT('Ctrl Pts',(-5.65014210968964,3.72400095868837,53.5118005913233));
#22326=CARTESIAN_POINT('Ctrl Pts',(-5.74488807005004,3.5802501524201,53.5198907507422));
#22327=CARTESIAN_POINT('Ctrl Pts',(-5.83422021707111,3.43276621887143,53.527980910161));
#22328=CARTESIAN_POINT('Ctrl Pts',(-5.91783259522884,3.28200340871961,53.5360710695798));
#22329=CARTESIAN_POINT('Ctrl Pts',(-6.00140935231352,3.13130482749169,53.5441577823778));
#22330=CARTESIAN_POINT('Ctrl Pts',(-6.07927101126975,2.97733047237376,53.5522444951759));
#22331=CARTESIAN_POINT('Ctrl Pts',(-6.15115588124769,2.82056205827704,53.5603312079739));
#22332=CARTESIAN_POINT('Ctrl Pts',(-6.22302411160969,2.66382993229214,53.5684160488927));
#22333=CARTESIAN_POINT('Ctrl Pts',(-6.28891815330792,2.50430537076334,53.5765008898115));
#22334=CARTESIAN_POINT('Ctrl Pts',(-6.34862312441312,2.3424929934083,53.5845857307303));
#22335=CARTESIAN_POINT('Ctrl Pts',(-6.40832589041272,2.18068659232917,53.5926702730487));
#22336=CARTESIAN_POINT('Ctrl Pts',(-6.46183991417272,2.01659289092625,53.6007548153671));
#22337=CARTESIAN_POINT('Ctrl Pts',(-6.50899918430194,1.85073461597192,53.6088393576855));
#22338=CARTESIAN_POINT('Ctrl Pts',(-6.55618318282665,1.68478937171109,53.6169281392078));
#22339=CARTESIAN_POINT('Ctrl Pts',(-6.59700566875786,1.51707806119666,53.6250169207301));
#22340=CARTESIAN_POINT('Ctrl Pts',(-6.6313509400887,1.34813712558655,53.6331057022524));
#22341=CARTESIAN_POINT('Ctrl Pts',(-6.66570576845019,1.17914917990377,53.6411967345862));
#22342=CARTESIAN_POINT('Ctrl Pts',(-6.69357972811641,1.00893129170854,53.64928776692));
#22343=CARTESIAN_POINT('Ctrl Pts',(-6.71490866735369,0.838027797330332,
53.6573787992538));
#22344=CARTESIAN_POINT('Ctrl Pts',(-6.73625802014904,0.666960734179693,
53.6654775753744));
#22345=CARTESIAN_POINT('Ctrl Pts',(-6.75104980613574,0.495207122242946,
53.673576351495));
#22346=CARTESIAN_POINT('Ctrl Pts',(-6.7592718950147,0.323314783553781,53.6816751276156));
#22347=CARTESIAN_POINT('Ctrl Pts',(-6.76451880553983,0.213622011517981,
53.6868433463364));
#22348=CARTESIAN_POINT('Ctrl Pts',(-6.76709137289696,0.103872766967097,
53.6920115650572));
#22349=CARTESIAN_POINT('Ctrl Pts',(-6.76699752191952,-0.00579122915667694,
53.697179783778));
#22350=CARTESIAN_POINT('',(-6.76699862526772,-0.00431342378654712,53.3028202162263));
#22351=CARTESIAN_POINT('Ctrl Pts',(3.09917575053253,6.01559628526642,52.6511649350805));
#22352=CARTESIAN_POINT('Ctrl Pts',(2.94515939621147,6.09494398877942,52.6592949270191));
#22353=CARTESIAN_POINT('Ctrl Pts',(2.78818271189624,6.16832714753178,52.6674249189578));
#22354=CARTESIAN_POINT('Ctrl Pts',(2.6287573478755,6.23553717060452,52.6755549108964));
#22355=CARTESIAN_POINT('Ctrl Pts',(2.46914177694221,6.30282738048479,52.6836946025505));
#22356=CARTESIAN_POINT('Ctrl Pts',(2.30707202997899,6.36392960719194,52.6918342942046));
#22357=CARTESIAN_POINT('Ctrl Pts',(2.14307717840784,6.41868438290804,52.6999739858587));
#22358=CARTESIAN_POINT('Ctrl Pts',(1.97896652703362,6.47347782198572,52.7081194250999));
#22359=CARTESIAN_POINT('Ctrl Pts',(1.81292841243395,6.52191477893482,52.7162648643411));
#22360=CARTESIAN_POINT('Ctrl Pts',(1.64550328180379,6.5638866496591,52.7244103035823));
#22361=CARTESIAN_POINT('Ctrl Pts',(1.47784304389534,6.60591745951787,52.7325671810827));
#22362=CARTESIAN_POINT('Ctrl Pts',(1.30879225749729,6.64146498483198,52.7407240585831));
#22363=CARTESIAN_POINT('Ctrl Pts',(1.13889846745706,6.67047219324269,52.7488809360836));
#22364=CARTESIAN_POINT('Ctrl Pts',(1.09418564949929,6.67810633942793,52.7510276712803));
#22365=CARTESIAN_POINT('Ctrl Pts',(1.04941445079136,6.6852877556321,52.753174406477));
#22366=CARTESIAN_POINT('Ctrl Pts',(1.0045948586897,6.69201600191558,52.7553211416737));
#22367=CARTESIAN_POINT('Ctrl Pts',(0.832705028385672,6.71781983139463,52.7635541918057));
#22368=CARTESIAN_POINT('Ctrl Pts',(0.659569085890686,6.73703443976784,52.7717872419377));
#22369=CARTESIAN_POINT('Ctrl Pts',(0.485733193020823,6.7495445968745,52.7800202920697));
#22370=CARTESIAN_POINT('Ctrl Pts',(0.312104311977997,6.76203985630706,52.7882435379046));
#22371=CARTESIAN_POINT('Ctrl Pts',(0.137777494084929,6.76784653707539,52.7964667837394));
#22372=CARTESIAN_POINT('Ctrl Pts',(-0.0366916789560165,6.76690052540271,
52.8046900295743));
#22373=CARTESIAN_POINT('Ctrl Pts',(-0.21098800641131,6.76595545093823,52.8129051286877));
#22374=CARTESIAN_POINT('Ctrl Pts',(-0.385426052436014,6.75827100888565,
52.8211202278012));
#22375=CARTESIAN_POINT('Ctrl Pts',(-0.559445794775028,6.74383491810917,
52.8293353269147));
#22376=CARTESIAN_POINT('Ctrl Pts',(-0.733327954622235,6.72941024071209,
52.8375439310536));
#22377=CARTESIAN_POINT('Ctrl Pts',(-0.906792114155987,6.70824457619736,
52.8457525351925));
#22378=CARTESIAN_POINT('Ctrl Pts',(-1.07927883681853,6.6803776983338,52.8539611393313));
#22379=CARTESIAN_POINT('Ctrl Pts',(-1.2516636911726,6.65252727826866,52.8621648955804));
#22380=CARTESIAN_POINT('Ctrl Pts',(-1.42307190598866,6.61798358599597,52.8703686518295));
#22381=CARTESIAN_POINT('Ctrl Pts',(-1.59294965437233,6.57683817640628,52.8785724080786));
#22382=CARTESIAN_POINT('Ctrl Pts',(-1.76277714020926,6.53570494070689,52.8867737370429));
#22383=CARTESIAN_POINT('Ctrl Pts',(-1.93107471304449,6.48797395901418,52.8949750660072));
#22384=CARTESIAN_POINT('Ctrl Pts',(-2.0972989744039,6.433787843251,52.9031763949714));
#22385=CARTESIAN_POINT('Ctrl Pts',(-2.26350031185091,6.37960920027044,52.9113765928942));
#22386=CARTESIAN_POINT('Ctrl Pts',(-2.42762856652253,6.31897730647894,52.9195767908169));
#22387=CARTESIAN_POINT('Ctrl Pts',(-2.589155718125,6.25208458574423,52.9277769887396));
#22388=CARTESIAN_POINT('Ctrl Pts',(-2.75068986559701,6.18518896783253,52.9359775418194));
#22389=CARTESIAN_POINT('Ctrl Pts',(-2.90962235449856,6.11203211979522,52.9441780948992));
#22390=CARTESIAN_POINT('Ctrl Pts',(-3.06544530637694,6.03285455432266,52.9523786479791));
#22391=CARTESIAN_POINT('Ctrl Pts',(-3.22130324524423,5.95365921108004,52.9605810423323));
#22392=CARTESIAN_POINT('Ctrl Pts',(-3.37404993715094,5.86844062019941,52.9687834366855));
#22393=CARTESIAN_POINT('Ctrl Pts',(-3.5232022135851,5.77748519359323,52.9769858310388));
#22394=CARTESIAN_POINT('Ctrl Pts',(-3.67249397361664,5.68644470767448,52.9851958960726));
#22395=CARTESIAN_POINT('Ctrl Pts',(-3.81818429606853,5.5896568540881,52.9934059611064));
#22396=CARTESIAN_POINT('Ctrl Pts',(-3.95981833588254,5.48745184460041,53.0016160261403));
#22397=CARTESIAN_POINT('Ctrl Pts',(-4.1015201592352,5.38519792160845,53.0098300203656));
#22398=CARTESIAN_POINT('Ctrl Pts',(-4.23916154734745,5.27752189422133,53.0180440145909));
#22399=CARTESIAN_POINT('Ctrl Pts',(-4.37232094003325,5.1647941485936,53.0262580088162));
#22400=CARTESIAN_POINT('Ctrl Pts',(-4.50566187332155,5.05191271750331,53.0344832014514));
#22401=CARTESIAN_POINT('Ctrl Pts',(-4.63450833501256,4.93396604605028,53.0427083940865));
#22402=CARTESIAN_POINT('Ctrl Pts',(-4.7584749478192,4.81136209102756,53.0509335867217));
#22403=CARTESIAN_POINT('Ctrl Pts',(-4.86995785720111,4.70110461687214,53.0583304848416));
#22404=CARTESIAN_POINT('Ctrl Pts',(-4.97749464124063,4.58708124221604,53.0657273829615));
#22405=CARTESIAN_POINT('Ctrl Pts',(-5.08083346162143,4.46961075880976,53.0731242810814));
#22406=CARTESIAN_POINT('Ctrl Pts',(-5.2016224685459,4.33230376245259,53.0817702475723));
#22407=CARTESIAN_POINT('Ctrl Pts',(-5.31694983733856,4.1899752222184,53.0904162140632));
#22408=CARTESIAN_POINT('Ctrl Pts',(-5.42640085573318,4.0430759024409,53.0990621805541));
#22409=CARTESIAN_POINT('Ctrl Pts',(-5.53571187139551,3.89636448686419,53.1076970876785));
#22410=CARTESIAN_POINT('Ctrl Pts',(-5.63916134397898,3.74509419367296,53.1163319948028));
#22411=CARTESIAN_POINT('Ctrl Pts',(-5.73637392148778,3.58974974515981,53.1249669019272));
#22412=CARTESIAN_POINT('Ctrl Pts',(-5.83681387810786,3.4292479863373,53.1338884809987));
#22413=CARTESIAN_POINT('Ctrl Pts',(-5.93059546957259,3.26439712748198,53.1428100600702));
#22414=CARTESIAN_POINT('Ctrl Pts',(-6.01735067509065,3.0957680554244,53.1517316391417));
#22415=CARTESIAN_POINT('Ctrl Pts',(-6.10108632156991,2.93300820395935,53.1603426981174));
#22416=CARTESIAN_POINT('Ctrl Pts',(-6.17827625866201,2.76672900032398,53.1689537570931));
#22417=CARTESIAN_POINT('Ctrl Pts',(-6.24863382533625,2.59747267875211,53.1775648160689));
#22418=CARTESIAN_POINT('Ctrl Pts',(-6.31892504157508,2.42837597370996,53.1861677544182));
#22419=CARTESIAN_POINT('Ctrl Pts',(-6.38239661685956,2.25630802893954,53.1947706927676));
#22420=CARTESIAN_POINT('Ctrl Pts',(-6.43880859873856,2.0818340060654,53.2033736311169));
#22421=CARTESIAN_POINT('Ctrl Pts',(-6.49515741224976,1.90755535372928,53.2119669361657));
#22422=CARTESIAN_POINT('Ctrl Pts',(-6.54446230921303,1.73087628779443,53.2205602412146));
#22423=CARTESIAN_POINT('Ctrl Pts',(-6.58653202175268,1.55238040648114,53.2291535462634));
#22424=CARTESIAN_POINT('Ctrl Pts',(-6.59121927634099,1.53249304362142,53.230110981104));
#22425=CARTESIAN_POINT('Ctrl Pts',(-6.59581676624511,1.51258314576003,53.2310684159446));
#22426=CARTESIAN_POINT('Ctrl Pts',(-6.60032426476746,1.4926515333198,53.2320258507851));
#22427=CARTESIAN_POINT('Ctrl Pts',(-6.63752498744106,1.32815444404714,53.2399276321848));
#22428=CARTESIAN_POINT('Ctrl Pts',(-6.66857070888122,1.16227112455706,53.2478294135844));
#22429=CARTESIAN_POINT('Ctrl Pts',(-6.69337176356371,0.995521689732583,
53.255731194984));
#22430=CARTESIAN_POINT('Ctrl Pts',(-6.71818808436948,0.828669613409205,
53.2636378402723));
#22431=CARTESIAN_POINT('Ctrl Pts',(-6.73675200528878,0.660950739777101,
53.2715444855606));
#22432=CARTESIAN_POINT('Ctrl Pts',(-6.74902561190871,0.492891762763725,
53.2794511308489));
#22433=CARTESIAN_POINT('Ctrl Pts',(-6.76111767498075,0.327318609509081,
53.2872408259626));
#22434=CARTESIAN_POINT('Ctrl Pts',(-6.76710426439709,0.16141570621137,53.2950305210762));
#22435=CARTESIAN_POINT('Ctrl Pts',(-6.76699862526822,-0.00431342301278818,
53.3028202161899));
#22436=CARTESIAN_POINT('Ctrl Pts',(-6.76699862526772,-0.00431342378654577,
53.3028202162263));
#22437=CARTESIAN_POINT('Ctrl Pts',(-6.7668657739302,-0.212733663223811,
53.3126165032661));
#22438=CARTESIAN_POINT('Ctrl Pts',(-6.75710010762463,-0.420817753426841,
53.3224127903059));
#22439=CARTESIAN_POINT('Ctrl Pts',(-6.73781830924752,-0.627768613080422,
53.3322090773457));
#22440=CARTESIAN_POINT('Ctrl Pts',(-6.71837254760011,-0.836479284711892,
53.3420886673653));
#22441=CARTESIAN_POINT('Ctrl Pts',(-6.68924817378419,-1.04403733784282,
53.3519682573849));
#22442=CARTESIAN_POINT('Ctrl Pts',(-6.65061516021554,-1.2496427452321,53.3618478474045));
#22443=CARTESIAN_POINT('Ctrl Pts',(-6.61271103871109,-1.45136897944904,
53.3715410384327));
#22444=CARTESIAN_POINT('Ctrl Pts',(-6.5656539155427,-1.65121560294499,53.3812342294609));
#22445=CARTESIAN_POINT('Ctrl Pts',(-6.50965016194429,-1.84844360722711,
53.3909274204891));
#22446=CARTESIAN_POINT('Ctrl Pts',(-6.46212335079957,-2.01581842605051,
53.3991534130305));
#22447=CARTESIAN_POINT('Ctrl Pts',(-6.40807475476983,-2.18157874669713,
53.4073794055718));
#22448=CARTESIAN_POINT('Ctrl Pts',(-6.34763095885382,-2.34518020847024,
53.4156053981132));
#22449=CARTESIAN_POINT('Ctrl Pts',(-6.28725053044514,-2.50861015525707,
53.4238227667646));
#22450=CARTESIAN_POINT('Ctrl Pts',(-6.22048837652145,-2.66988541688268,
53.432040135416));
#22451=CARTESIAN_POINT('Ctrl Pts',(-6.14752138460948,-2.82847482325177,
53.4402575040674));
#22452=CARTESIAN_POINT('Ctrl Pts',(-6.0746162887784,-2.98692970217952,53.4484679021298));
#22453=CARTESIAN_POINT('Ctrl Pts',(-5.99551698666296,-3.14270293981774,
53.4566783001921));
#22454=CARTESIAN_POINT('Ctrl Pts',(-5.9104491970952,-3.29528136713038,53.4648886982545));
#22455=CARTESIAN_POINT('Ctrl Pts',(-5.82543655151031,-3.44776088765088,
53.4730937740433));
#22456=CARTESIAN_POINT('Ctrl Pts',(-5.7344632990645,-3.59704941129093,53.4812988498321));
#22457=CARTESIAN_POINT('Ctrl Pts',(-5.63780205186725,-3.74265641275839,
53.4895039256209));
#22458=CARTESIAN_POINT('Ctrl Pts',(-5.54118413182602,-3.88819814776742,
53.4977053235904));
#22459=CARTESIAN_POINT('Ctrl Pts',(-5.43888349427051,-4.03006135039806,
53.5059067215598));
#22460=CARTESIAN_POINT('Ctrl Pts',(-5.33121725879015,-4.16778256865422,
53.5141081195293));
#22461=CARTESIAN_POINT('Ctrl Pts',(-5.22355945662589,-4.30549299943778,
53.522308875097));
#22462=CARTESIAN_POINT('Ctrl Pts',(-5.11053710730422,-4.43906180466784,
53.5305096306648));
#22463=CARTESIAN_POINT('Ctrl Pts',(-4.99250921412986,-4.5680565612554,53.5387103862325));
#22464=CARTESIAN_POINT('Ctrl Pts',(-4.87448192048102,-4.69705066261098,
53.5469111001442));
#22465=CARTESIAN_POINT('Ctrl Pts',(-4.75144937475753,-4.82147049648515,
53.555111814056));
#22466=CARTESIAN_POINT('Ctrl Pts',(-4.62380914846253,-4.94091873628723,
53.5633125279678));
#22467=CARTESIAN_POINT('Ctrl Pts',(-4.496146438932,-5.06038801634432,53.5715146863974));
#22468=CARTESIAN_POINT('Ctrl Pts',(-4.36387469348221,-5.1748837127253,53.579716844827));
#22469=CARTESIAN_POINT('Ctrl Pts',(-4.22742646181163,-5.28404717143733,
53.5879190032566));
#22470=CARTESIAN_POINT('Ctrl Pts',(-4.09092946733719,-5.39324964213406,
53.5961240929096));
#22471=CARTESIAN_POINT('Ctrl Pts',(-3.95025329303532,-5.49711585537118,
53.6043291825625));
#22472=CARTESIAN_POINT('Ctrl Pts',(-3.80586153818101,-5.59532902984217,
53.6125342722155));
#22473=CARTESIAN_POINT('Ctrl Pts',(-3.6613048328186,-5.69365440125299,53.6207487352133));
#22474=CARTESIAN_POINT('Ctrl Pts',(-3.51302436353896,-5.78631363033407,
53.628963198211));
#22475=CARTESIAN_POINT('Ctrl Pts',(-3.36151144712169,-5.87303412137797,
53.6371776612088));
#22476=CARTESIAN_POINT('Ctrl Pts',(-3.20990876409008,-5.95980599157196,
53.6453969910163));
#22477=CARTESIAN_POINT('Ctrl Pts',(-3.05507013350502,-6.04063194441922,
53.6536163208237));
#22478=CARTESIAN_POINT('Ctrl Pts',(-2.89750906385215,-6.11528660202403,
53.6618356506312));
#22479=CARTESIAN_POINT('Ctrl Pts',(-2.73970386287458,-6.19005693249459,
53.6700677157919));
#22480=CARTESIAN_POINT('Ctrl Pts',(-2.5791681224417,-6.25863671833393,53.6782997809526));
#22481=CARTESIAN_POINT('Ctrl Pts',(-2.4164340604615,-6.32084926504671,53.6865318461133));
#22482=CARTESIAN_POINT('Ctrl Pts',(-2.27015700060778,-6.37677036913779,
53.6939314173744));
#22483=CARTESIAN_POINT('Ctrl Pts',(-2.12210415199189,-6.4275475489319,53.7013309886355));
#22484=CARTESIAN_POINT('Ctrl Pts',(-1.97266978345942,-6.47308758827085,
53.7087305598966));
#22485=CARTESIAN_POINT('Ctrl Pts',(-1.80797027127025,-6.5232796715102,53.7168860183034));
#22486=CARTESIAN_POINT('Ctrl Pts',(-1.64108525912738,-6.56726366386642,
53.7250414767102));
#22487=CARTESIAN_POINT('Ctrl Pts',(-1.47252769844495,-6.60484300928587,
53.7331969351169));
#22488=CARTESIAN_POINT('Ctrl Pts',(-1.30417529447042,-6.64237661570222,
53.7413424672588));
#22489=CARTESIAN_POINT('Ctrl Pts',(-1.13415474695746,-6.67352101341617,
53.7494879994007));
#22490=CARTESIAN_POINT('Ctrl Pts',(-0.962996420609403,-6.6981286113282,
53.7576335315426));
#22491=CARTESIAN_POINT('Ctrl Pts',(-0.792010425280498,-6.72271143304315,
53.7657708623432));
#22492=CARTESIAN_POINT('Ctrl Pts',(-0.619889290828873,-6.7407705061041,
53.7739081931437));
#22493=CARTESIAN_POINT('Ctrl Pts',(-0.447175898437896,-6.75220872869436,
53.7820455239443));
#22494=CARTESIAN_POINT('Ctrl Pts',(-0.274600106533052,-6.7636378384708,
53.7901763717463));
#22495=CARTESIAN_POINT('Ctrl Pts',(-0.101433359209004,-6.76845657656059,
53.7983072195483));
#22496=CARTESIAN_POINT('Ctrl Pts',(0.0717739725180646,-6.76661935510407,
53.8064380673503));
#22497=CARTESIAN_POINT('Ctrl Pts',(0.244879695437417,-6.76478321141879,
53.8145641453441));
#22498=CARTESIAN_POINT('Ctrl Pts',(0.418025590781101,-6.75629888797378,
53.8226902233378));
#22499=CARTESIAN_POINT('Ctrl Pts',(0.590658902779662,-6.74117282530029,
53.8308163013316));
#22500=CARTESIAN_POINT('Ctrl Pts',(0.763904340972275,-6.72599312837124,
53.8389711929138));
#22501=CARTESIAN_POINT('Ctrl Pts',(0.936633182670272,-6.7041244865418,53.8471260844961));
#22502=CARTESIAN_POINT('Ctrl Pts',(1.10828892944676,-6.67562616155711,53.8552809760782));
#22503=CARTESIAN_POINT('Ctrl Pts',(1.27927527882838,-6.64723897007574,53.8634040664345));
#22504=CARTESIAN_POINT('Ctrl Pts',(1.44919652710337,-6.61227378673521,53.8715271567908));
#22505=CARTESIAN_POINT('Ctrl Pts',(1.61751027262617,-6.57084085318986,53.8796502471471));
#22506=CARTESIAN_POINT('Ctrl Pts',(1.78583723491278,-6.52940466614138,53.8877739753655));
#22507=CARTESIAN_POINT('Ctrl Pts',(1.95255608777658,-6.48149980465698,53.895897703584));
#22508=CARTESIAN_POINT('Ctrl Pts',(2.11713728372672,-6.42728704212394,53.9040214318024));
#22509=CARTESIAN_POINT('Ctrl Pts',(2.28176271472091,-6.37305970864356,53.9121473434627));
#22510=CARTESIAN_POINT('Ctrl Pts',(2.44424899745888,-6.31252121266928,53.920273255123));
#22511=CARTESIAN_POINT('Ctrl Pts',(2.60408437468839,-6.2458813284839,53.9283991667834));
#22512=CARTESIAN_POINT('Ctrl Pts',(2.76494191577037,-6.17881527531186,53.9365770444934));
#22513=CARTESIAN_POINT('Ctrl Pts',(2.92311418135037,-6.10556966957484,53.9447549222035));
#22514=CARTESIAN_POINT('Ctrl Pts',(3.07810327724429,-6.02640599483788,53.9529327999136));
#22515=CARTESIAN_POINT('Ctrl Pts',(3.23235264379837,-5.947620151151,53.961071646387));
#22516=CARTESIAN_POINT('Ctrl Pts',(3.38344887013187,-5.86297283847708,53.9692104928605));
#22517=CARTESIAN_POINT('Ctrl Pts',(3.53092932571211,-5.77276598320305,53.9773493393339));
#22518=CARTESIAN_POINT('Ctrl Pts',(3.67947068308868,-5.68191022421886,53.9855467326623));
#22519=CARTESIAN_POINT('Ctrl Pts',(3.82434373903263,-5.58541484526097,53.9937441259907));
#22520=CARTESIAN_POINT('Ctrl Pts',(3.9651091049225,-5.48363007377966,54.0019415193191));
#22521=CARTESIAN_POINT('Ctrl Pts',(4.10587447081243,-5.38184530229831,54.0101389126475));
#22522=CARTESIAN_POINT('Ctrl Pts',(4.24253189133332,-5.27477141597334,54.0183363059759));
#22523=CARTESIAN_POINT('Ctrl Pts',(4.3746794556649,-5.16279659295071,54.0265336993043));
#22524=CARTESIAN_POINT('Ctrl Pts',(4.50729155368351,-5.05042814876937,54.0347599086413));
#22525=CARTESIAN_POINT('Ctrl Pts',(4.63575678636189,-4.93278991264607,54.0429861179783));
#22526=CARTESIAN_POINT('Ctrl Pts',(4.7596304403996,-4.81021902524423,54.0512123273153));
#22527=CARTESIAN_POINT('Ctrl Pts',(4.88336492769362,-4.68778584098357,54.0594292948585));
#22528=CARTESIAN_POINT('Ctrl Pts',(5.00251785559057,-4.56043129027937,54.0676462624017));
#22529=CARTESIAN_POINT('Ctrl Pts',(5.11667701461948,-4.42853308986901,54.0758632299448));
#22530=CARTESIAN_POINT('Ctrl Pts',(5.23073083338146,-4.29675659841091,54.0840726152882));
#22531=CARTESIAN_POINT('Ctrl Pts',(5.33979982704329,-4.16044507653162,54.0922820006316));
#22532=CARTESIAN_POINT('Ctrl Pts',(5.44350809155414,-4.02001351455249,54.100491385975));
#22533=CARTESIAN_POINT('Ctrl Pts',(5.54714146775072,-3.87968335898484,54.1086948432756));
#22534=CARTESIAN_POINT('Ctrl Pts',(5.64542161299945,-3.73523937653856,54.1168983005762));
#22535=CARTESIAN_POINT('Ctrl Pts',(5.73801238649264,-3.58713016943309,54.1251017578768));
#22536=CARTESIAN_POINT('Ctrl Pts',(5.83055487315543,-3.43909820246606,54.1333009370086));
#22537=CARTESIAN_POINT('Ctrl Pts',(5.91741370930256,-3.28740512215544,54.1415001161405));
#22538=CARTESIAN_POINT('Ctrl Pts',(5.99829559759164,-3.13252915771151,54.1496992952724));
#22539=CARTESIAN_POINT('Ctrl Pts',(6.07916224598982,-2.97768237523713,54.1578969295022));
#22540=CARTESIAN_POINT('Ctrl Pts',(6.15405401841697,-2.81965421790738,54.166094563732));
#22541=CARTESIAN_POINT('Ctrl Pts',(6.22272303809128,-2.65894847471853,54.1742921979618));
#22542=CARTESIAN_POINT('Ctrl Pts',(6.29138710116054,-2.49825433144625,54.1824892404774));
#22543=CARTESIAN_POINT('Ctrl Pts',(6.3538291642663,-2.33488331670718,54.190686282993));
#22544=CARTESIAN_POINT('Ctrl Pts',(6.4098491032884,-2.16936015291905,54.1988833255086));
#22545=CARTESIAN_POINT('Ctrl Pts',(6.46587518026003,-2.0038188532164,54.2070812661514));
#22546=CARTESIAN_POINT('Ctrl Pts',(6.51547761625543,-1.83612527449301,54.2152792067943));
#22547=CARTESIAN_POINT('Ctrl Pts',(6.55850584910796,-1.66682033441422,54.2234771474371));
#22548=CARTESIAN_POINT('Ctrl Pts',(6.60154661678304,-1.49746607305868,54.2316774762731));
#22549=CARTESIAN_POINT('Ctrl Pts',(6.63800927819798,-1.32649986287014,54.2398778051091));
#22550=CARTESIAN_POINT('Ctrl Pts',(6.66779416029866,-1.15447392170076,54.2480781339451));
#22551=CARTESIAN_POINT('Ctrl Pts',(6.69761007901933,-0.982268725037,54.2562870077365));
#22552=CARTESIAN_POINT('Ctrl Pts',(6.72073425528281,-0.809001945121539,
54.2644958815279));
#22553=CARTESIAN_POINT('Ctrl Pts',(6.73711866972606,-0.635233051744458,
54.2727047553193));
#22554=CARTESIAN_POINT('Ctrl Pts',(6.7535118775038,-0.461370898519205,54.2809180347227));
#22555=CARTESIAN_POINT('Ctrl Pts',(6.76315809274141,-0.287006452402152,
54.2891313141262));
#22556=CARTESIAN_POINT('Ctrl Pts',(6.76606145846543,-0.112700223019793,
54.2973445935296));
#22557=CARTESIAN_POINT('Ctrl Pts',(6.76896907081815,0.0618609566189891,
54.3055698861451));
#22558=CARTESIAN_POINT('Ctrl Pts',(6.76511413205971,0.236363390784799,54.3137951787605));
#22559=CARTESIAN_POINT('Ctrl Pts',(6.75455286888362,0.410249364967281,54.3220204713759));
#22560=CARTESIAN_POINT('Ctrl Pts',(6.74500147500663,0.567508340660824,54.329459260488));
#22561=CARTESIAN_POINT('Ctrl Pts',(6.72996565522437,0.724262994944808,54.3368980496));
#22562=CARTESIAN_POINT('Ctrl Pts',(6.70952298555752,0.880108121923286,54.3443368387121));
#22563=CARTESIAN_POINT('Ctrl Pts',(6.68691590961242,1.05245364619639,54.3525632236772));
#22564=CARTESIAN_POINT('Ctrl Pts',(6.65763248579208,1.22416845318491,54.3607896086424));
#22565=CARTESIAN_POINT('Ctrl Pts',(6.62171517814278,1.39469605991898,54.3690159936076));
#22566=CARTESIAN_POINT('Ctrl Pts',(6.58583838831994,1.56503129677822,54.3772330984997));
#22567=CARTESIAN_POINT('Ctrl Pts',(6.54334269003506,1.73418165247868,54.3854502033918));
#22568=CARTESIAN_POINT('Ctrl Pts',(6.49432226520474,1.90159599170432,54.393667308284));
#22569=CARTESIAN_POINT('Ctrl Pts',(6.44534730067471,2.06885507511243,54.4018767928412));
#22570=CARTESIAN_POINT('Ctrl Pts',(6.38985976052621,2.2343810063116,54.4100862773984));
#22571=CARTESIAN_POINT('Ctrl Pts',(6.32800482632947,2.39763298232881,54.4182957619556));
#22572=CARTESIAN_POINT('Ctrl Pts',(6.26619484386969,2.56076631849977,54.4264992804472));
#22573=CARTESIAN_POINT('Ctrl Pts',(6.19802681108652,2.72162865713693,54.4347027989389));
#22574=CARTESIAN_POINT('Ctrl Pts',(6.12369570284242,2.87969441764041,54.4429063174306));
#22575=CARTESIAN_POINT('Ctrl Pts',(6.04940370234929,3.03767701516481,54.4511055198133));
#22576=CARTESIAN_POINT('Ctrl Pts',(5.96895523867511,3.1928656420963,54.4593047221961));
#22577=CARTESIAN_POINT('Ctrl Pts',(5.88259339742212,3.34475468765733,54.4675039245789));
#22578=CARTESIAN_POINT('Ctrl Pts',(5.79625018319389,3.49661097290464,54.4757013585099));
#22579=CARTESIAN_POINT('Ctrl Pts',(5.70399630503805,3.64516878067554,54.483898792441));
#22580=CARTESIAN_POINT('Ctrl Pts',(5.6061209149474,3.7899468712621,54.492096226372));
#22581=CARTESIAN_POINT('Ctrl Pts',(5.50825324360556,3.93471354421126,54.5002930138287));
#22582=CARTESIAN_POINT('Ctrl Pts',(5.40476514373408,4.07570079626699,54.5084898012854));
#22583=CARTESIAN_POINT('Ctrl Pts',(5.29598922111453,4.21245619203793,54.516686588742));
#22584=CARTESIAN_POINT('Ctrl Pts',(5.18720210735474,4.34922565754762,54.5248842195048));
#22585=CARTESIAN_POINT('Ctrl Pts',(5.07312631060924,4.48176211890996,54.5330818502675));
#22586=CARTESIAN_POINT('Ctrl Pts',(4.95413488642051,4.60964603057016,54.5412794810303));
#22587=CARTESIAN_POINT('Ctrl Pts',(4.83510959399437,4.73756634151469,54.5494794450646));
#22588=CARTESIAN_POINT('Ctrl Pts',(4.7111661317907,4.86083120287225,54.5576794090989));
#22589=CARTESIAN_POINT('Ctrl Pts',(4.582714608375,4.97905772392592,54.5658793731332));
#22590=CARTESIAN_POINT('Ctrl Pts',(4.45414192612709,5.09739575932248,54.5740870715878));
#22591=CARTESIAN_POINT('Ctrl Pts',(4.32105295405945,5.2106857196889,54.5822947700423));
#22592=CARTESIAN_POINT('Ctrl Pts',(4.18389174031732,5.31858429521471,54.5905024684969));
#22593=CARTESIAN_POINT('Ctrl Pts',(4.04665726739587,5.4265405004514,54.5987145507655));
#22594=CARTESIAN_POINT('Ctrl Pts',(3.9053465066936,5.52909937007814,54.6069266330341));
#22595=CARTESIAN_POINT('Ctrl Pts',(3.76043261936165,5.6259608526225,54.6151387153027));
#22596=CARTESIAN_POINT('Ctrl Pts',(3.61533942837926,5.72294218301393,54.6233609584769));
#22597=CARTESIAN_POINT('Ctrl Pts',(3.46663451090963,5.81421185833465,54.6315832016511));
#22598=CARTESIAN_POINT('Ctrl Pts',(3.31481654211206,5.89951525908191,54.6398054448253));
#22599=CARTESIAN_POINT('Ctrl Pts',(3.24360327303733,5.93952853339006,54.6436622532137));
#22600=CARTESIAN_POINT('Ctrl Pts',(3.17170535883719,5.97822974792016,54.647519061602));
#22601=CARTESIAN_POINT('Ctrl Pts',(3.09917575053251,6.01559628526643,54.6513758699904));
#22602=CARTESIAN_POINT('Origin',(0.,0.,-3.69717978381041));
#22603=CARTESIAN_POINT('',(3.09917575053258,6.01559628526639,57.0458946091258));
#22604=CARTESIAN_POINT('',(3.09917575053263,6.01559628526637,56.6515777772535));
#22605=CARTESIAN_POINT('',(3.09917575053259,6.01559628526639,-3.69717978381041));
#22606=CARTESIAN_POINT('',(-6.76699940565952,0.00283616003333658,55.6971797838559));
#22607=CARTESIAN_POINT('Ctrl Pts',(-6.76699940565952,0.00283616003323741,
55.6971797838558));
#22608=CARTESIAN_POINT('Ctrl Pts',(-6.76707134889961,-0.168818421231435,
55.7052944011409));
#22609=CARTESIAN_POINT('Ctrl Pts',(-6.76060770170997,-0.340730811922388,
55.7134090184261));
#22610=CARTESIAN_POINT('Ctrl Pts',(-6.74757589657687,-0.512355852835504,
55.7215236357112));
#22611=CARTESIAN_POINT('Ctrl Pts',(-6.7345577476259,-0.683801045846384,
55.7296297495932));
#22612=CARTESIAN_POINT('Ctrl Pts',(-6.71498516853079,-0.854959123553571,
55.7377358634753));
#22613=CARTESIAN_POINT('Ctrl Pts',(-6.68887757730892,-1.02528325636085,
55.7458419773573));
#22614=CARTESIAN_POINT('Ctrl Pts',(-6.66279174601455,-1.19546542889505,
55.7539413350262));
#22615=CARTESIAN_POINT('Ctrl Pts',(-6.63018180148919,-1.36481467740047,
55.7620406926952));
#22616=CARTESIAN_POINT('Ctrl Pts',(-6.59111909538432,-1.53278767951083,
55.7701400503641));
#22617=CARTESIAN_POINT('Ctrl Pts',(-6.5520805758803,-1.70065667715348,55.7782343931237));
#22618=CARTESIAN_POINT('Ctrl Pts',(-6.50659733355476,-1.86715076671615,
55.7863287358832));
#22619=CARTESIAN_POINT('Ctrl Pts',(-6.45479207658211,-2.03173528002365,
55.7944230786428));
#22620=CARTESIAN_POINT('Ctrl Pts',(-6.40300243503939,-2.19627018334781,
55.8025149815603));
#22621=CARTESIAN_POINT('Ctrl Pts',(-6.34489467906279,-2.35889630336945,
55.8106068844779));
#22622=CARTESIAN_POINT('Ctrl Pts',(-6.28064183324126,-2.51909252758604,
55.8186987873954));
#22623=CARTESIAN_POINT('Ctrl Pts',(-6.21639767769422,-2.67926708507111,
55.8267895958734));
#22624=CARTESIAN_POINT('Ctrl Pts',(-6.14601022330997,-2.83701205795902,
55.8348804043514));
#22625=CARTESIAN_POINT('Ctrl Pts',(-6.06970120868306,-2.9918249008442,55.8429712128293));
#22626=CARTESIAN_POINT('Ctrl Pts',(-5.99338771118787,-3.14664683840301,
55.851062496612));
#22627=CARTESIAN_POINT('Ctrl Pts',(-5.91115212404481,-3.2985359716822,55.8591537803946));
#22628=CARTESIAN_POINT('Ctrl Pts',(-5.82326280444565,-3.44701309982422,
55.8672450641772));
#22629=CARTESIAN_POINT('Ctrl Pts',(-5.7353512698158,-3.59552775725847,55.8753383931243));
#22630=CARTESIAN_POINT('Ctrl Pts',(-5.64178334607896,-3.74062837509862,
55.8834317220714));
#22631=CARTESIAN_POINT('Ctrl Pts',(-5.54287143362222,-3.88186363366036,
55.8915250510186));
#22632=CARTESIAN_POINT('Ctrl Pts',(-5.44386021068177,-4.02324069659627,
55.8996265059072));
#22633=CARTESIAN_POINT('Ctrl Pts',(-5.3394944940311,-4.16074434571123,55.9077279607958));
#22634=CARTESIAN_POINT('Ctrl Pts',(-5.2301283013377,-4.2939546983575,55.9158294156844));
#22635=CARTESIAN_POINT('Ctrl Pts',(-5.12070475684185,-4.42723490672098,
55.9239351189886));
#22636=CARTESIAN_POINT('Ctrl Pts',(-5.00627575655876,-4.55621705729177,
55.9320408222929));
#22637=CARTESIAN_POINT('Ctrl Pts',(-4.88723282960504,-4.68051752151733,
55.9401465255971));
#22638=CARTESIAN_POINT('Ctrl Pts',(-4.76801861168757,-4.80499684178127,
55.9482638922043));
#22639=CARTESIAN_POINT('Ctrl Pts',(-4.64417746908534,-4.92478076149952,
55.9563812588116));
#22640=CARTESIAN_POINT('Ctrl Pts',(-4.51613550604893,-5.03952468899639,
55.9644986254188));
#22641=CARTESIAN_POINT('Ctrl Pts',(-4.40986072031907,-5.1347621097556,55.9712360369394));
#22642=CARTESIAN_POINT('Ctrl Pts',(-4.30069266936053,-5.22652816319539,
55.9779734484599));
#22643=CARTESIAN_POINT('Ctrl Pts',(-4.18888991287168,-5.31464865234212,
55.9847108599805));
#22644=CARTESIAN_POINT('Ctrl Pts',(-4.05240415550037,-5.42222374332229,
55.9929357083025));
#22645=CARTESIAN_POINT('Ctrl Pts',(-3.91158021645315,-5.52468878958651,
56.0011605566246));
#22646=CARTESIAN_POINT('Ctrl Pts',(-3.76683671702674,-5.62167503038545,
56.0093854049466));
#22647=CARTESIAN_POINT('Ctrl Pts',(-3.62225623087324,-5.71855204317344,
56.0176009902658));
#22648=CARTESIAN_POINT('Ctrl Pts',(-3.4737652696585,-5.80996233934751,56.025816575585));
#22649=CARTESIAN_POINT('Ctrl Pts',(-3.32181576814251,-5.89557707120514,
56.0340321609042));
#22650=CARTESIAN_POINT('Ctrl Pts',(-3.17000686577554,-5.98111258359629,
56.0422401443274));
#22651=CARTESIAN_POINT('Ctrl Pts',(-3.01474610696026,-6.06086303648539,
56.0504481277507));
#22652=CARTESIAN_POINT('Ctrl Pts',(-2.85651474687221,-6.13454256655715,
56.0586561111739));
#22653=CARTESIAN_POINT('Ctrl Pts',(-2.69839801697386,-6.20816871973508,
56.0668581483504));
#22654=CARTESIAN_POINT('Ctrl Pts',(-2.53731529618713,-6.27573255936942,
56.075060185527));
#22655=CARTESIAN_POINT('Ctrl Pts',(-2.37377288303919,-6.33699386931594,
56.0832622227036));
#22656=CARTESIAN_POINT('Ctrl Pts',(-2.21031610689051,-6.39822310052121,
56.0914599649829));
#22657=CARTESIAN_POINT('Ctrl Pts',(-2.04440253943738,-6.45315625109748,
56.0996577072623));
#22658=CARTESIAN_POINT('Ctrl Pts',(-1.87655900350602,-6.5016009802479,56.1078554495417));
#22659=CARTESIAN_POINT('Ctrl Pts',(-1.70874738024495,-6.55003649843492,
56.116051633156));
#22660=CARTESIAN_POINT('Ctrl Pts',(-1.53900686205038,-6.59198594712425,
56.1242478167704));
#22661=CARTESIAN_POINT('Ctrl Pts',(-1.36788029639942,-6.6273065792011,56.1324440003847));
#22662=CARTESIAN_POINT('Ctrl Pts',(-1.1967663280512,-6.66262461118665,56.1406395806456));
#22663=CARTESIAN_POINT('Ctrl Pts',(-1.02426686668324,-6.6913147249621,56.1488351609065));
#22664=CARTESIAN_POINT('Ctrl Pts',(-0.850935785196513,-6.71328513393197,
56.1570307411674));
#22665=CARTESIAN_POINT('Ctrl Pts',(-0.677585927756354,-6.73525792282916,
56.1652272092081));
#22666=CARTESIAN_POINT('Ctrl Pts',(-0.503404626776022,-6.75050951157719,
56.1734236772488));
#22667=CARTESIAN_POINT('Ctrl Pts',(-0.328951775392259,-6.75899990601171,
56.1816201452895));
#22668=CARTESIAN_POINT('Ctrl Pts',(-0.154448286773356,-6.76749276489491,
56.1898189924629));
#22669=CARTESIAN_POINT('Ctrl Pts',(0.0203265509343518,-6.76922050292508,
56.1980178396363));
#22670=CARTESIAN_POINT('Ctrl Pts',(0.194811887535325,-6.76419524618228,
56.2062166868096));
#22671=CARTESIAN_POINT('Ctrl Pts',(0.369479578280686,-6.75916473755751,
56.2144241025756));
#22672=CARTESIAN_POINT('Ctrl Pts',(0.543856804288456,-6.7473671444689,56.2226315183416));
#22673=CARTESIAN_POINT('Ctrl Pts',(0.717385873467032,-6.72886665855031,
56.2308389341075));
#22674=CARTESIAN_POINT('Ctrl Pts',(0.891007948123133,-6.71035625702198,
56.2390507487596));
#22675=CARTESIAN_POINT('Ctrl Pts',(1.06378060499883,-6.68513585267878,56.2472625634118));
#22676=CARTESIAN_POINT('Ctrl Pts',(1.23515550778358,-6.6533209656225,56.2554743780639));
#22677=CARTESIAN_POINT('Ctrl Pts',(1.40678278616593,-6.62145922630837,56.2636982858615));
#22678=CARTESIAN_POINT('Ctrl Pts',(1.57700784678693,-6.58298367547638,56.2719221936591));
#22679=CARTESIAN_POINT('Ctrl Pts',(1.745295437402,-6.53806032674705,56.2801461014567));
#22680=CARTESIAN_POINT('Ctrl Pts',(1.90079006314705,-6.49655198217838,56.2877448403802));
#22681=CARTESIAN_POINT('Ctrl Pts',(2.05463055554878,-6.44953950084289,56.2953435793037));
#22682=CARTESIAN_POINT('Ctrl Pts',(2.20641016366796,-6.39719025742261,56.3029423182272));
#22683=CARTESIAN_POINT('Ctrl Pts',(2.36922045267152,-6.34103649898305,56.3110933004015));
#22684=CARTESIAN_POINT('Ctrl Pts',(2.53014140601998,-6.27857511840655,56.3192442825758));
#22685=CARTESIAN_POINT('Ctrl Pts',(2.68864296595399,-6.20995072457311,56.3273952647501));
#22686=CARTESIAN_POINT('Ctrl Pts',(2.84696041163582,-6.1414060443334,56.3355367788031));
#22687=CARTESIAN_POINT('Ctrl Pts',(3.00286372596184,-6.06671274500468,56.3436782928561));
#22688=CARTESIAN_POINT('Ctrl Pts',(3.15583778969361,-5.98606522225926,56.3518198069092));
#22689=CARTESIAN_POINT('Ctrl Pts',(3.30866635122605,-5.90549440788939,56.3599535771122));
#22690=CARTESIAN_POINT('Ctrl Pts',(3.45857088775684,-5.81898081446106,56.3680873473153));
#22691=CARTESIAN_POINT('Ctrl Pts',(3.60505606954399,-5.72676695312845,56.3762211175183));
#22692=CARTESIAN_POINT('Ctrl Pts',(3.75143272991933,-5.63462140709091,56.3843488619363));
#22693=CARTESIAN_POINT('Ctrl Pts',(3.89439477132242,-5.53678419572485,56.3924766063543));
#22694=CARTESIAN_POINT('Ctrl Pts',(4.03347131311705,-5.43354379445513,56.4006043507722));
#22695=CARTESIAN_POINT('Ctrl Pts',(4.17247406187973,-5.330358171814,56.4087277826663));
#22696=CARTESIAN_POINT('Ctrl Pts',(4.3075951238005,-5.22177528624459,56.4168512145604));
#22697=CARTESIAN_POINT('Ctrl Pts',(4.43839248785028,-5.10812696825306,56.4249746464545));
#22698=CARTESIAN_POINT('Ctrl Pts',(4.57001957893041,-4.99375771003405,56.4331496102053));
#22699=CARTESIAN_POINT('Ctrl Pts',(4.69726761262311,-4.87425873615773,56.4413245739561));
#22700=CARTESIAN_POINT('Ctrl Pts',(4.81971946900952,-4.75000981473203,56.449499537707));
#22701=CARTESIAN_POINT('Ctrl Pts',(4.94137183363872,-4.62657211815382,56.45762112688));
#22702=CARTESIAN_POINT('Ctrl Pts',(5.05829022241523,-4.49844659671581,56.465742716053));
#22703=CARTESIAN_POINT('Ctrl Pts',(5.17010247939526,-4.3660427566105,56.473864305226));
#22704=CARTESIAN_POINT('Ctrl Pts',(5.2819294978866,-4.23362143648254,56.4819869666154));
#22705=CARTESIAN_POINT('Ctrl Pts',(5.38864880570886,-4.09692095230147,56.4901096280048));
#22706=CARTESIAN_POINT('Ctrl Pts',(5.48992853191956,-3.95638391898657,56.4982322893941));
#22707=CARTESIAN_POINT('Ctrl Pts',(5.59124091578664,-3.81580156949327,56.5063575699364));
#22708=CARTESIAN_POINT('Ctrl Pts',(5.68711001143615,-3.67138050419232,56.5144828504786));
#22709=CARTESIAN_POINT('Ctrl Pts',(5.77724730308799,-3.52359228614244,56.5226081310208));
#22710=CARTESIAN_POINT('Ctrl Pts',(5.8683666218291,-3.37419394612263,56.5308219348086));
#22711=CARTESIAN_POINT('Ctrl Pts',(5.95362831122039,-3.22135498257339,56.5390357385963));
#22712=CARTESIAN_POINT('Ctrl Pts',(6.03278246772727,-3.06558717003488,56.5472495423841));
#22713=CARTESIAN_POINT('Ctrl Pts',(6.11121904553692,-2.91123148376901,56.5553888832393));
#22714=CARTESIAN_POINT('Ctrl Pts',(6.18365827760207,-2.7540001919264,56.5635282240944));
#22715=CARTESIAN_POINT('Ctrl Pts',(6.24990600766964,-2.59441012472874,56.5716675649496));
#22716=CARTESIAN_POINT('Ctrl Pts',(6.31706284088456,-2.43263003785449,56.5799186002037));
#22717=CARTESIAN_POINT('Ctrl Pts',(6.377856874295,-2.26842633637579,56.5881696354577));
#22718=CARTESIAN_POINT('Ctrl Pts',(6.4321386101332,-2.10235151676254,56.5964206707118));
#22719=CARTESIAN_POINT('Ctrl Pts',(6.48642034597141,-1.9362766971493,56.6046717059658));
#22720=CARTESIAN_POINT('Ctrl Pts',(6.53418974372113,-1.76833114698214,56.6129227412199));
#22721=CARTESIAN_POINT('Ctrl Pts',(6.57535136644329,-1.59907579801969,56.621173776474));
#22722=CARTESIAN_POINT('Ctrl Pts',(6.61641689146346,-1.43021559990437,56.6294055485048));
#22723=CARTESIAN_POINT('Ctrl Pts',(6.65103383186121,-1.25952460223781,56.6376373205357));
#22724=CARTESIAN_POINT('Ctrl Pts',(6.67903840006713,-1.08753622947872,56.6458690925665));
#22725=CARTESIAN_POINT('Ctrl Pts',(6.70700952802003,-0.915753228023974,
56.6540910350389));
#22726=CARTESIAN_POINT('Ctrl Pts',(6.72838394919001,-0.742676286453013,
56.6623129775113));
#22727=CARTESIAN_POINT('Ctrl Pts',(6.74304793715289,-0.568852808077908,
56.6705349199837));
#22728=CARTESIAN_POINT('Ctrl Pts',(6.75769735290761,-0.395202065244957,
56.6787486919736));
#22729=CARTESIAN_POINT('Ctrl Pts',(6.76564958570011,-0.220806617608481,
56.6869624639635));
#22730=CARTESIAN_POINT('Ctrl Pts',(6.76684213195596,-0.0462229508549047,
56.6951762359534));
#22731=CARTESIAN_POINT('Ctrl Pts',(6.76803373197987,0.12822219159306,56.7033834906838));
#22732=CARTESIAN_POINT('Ctrl Pts',(6.76247632597551,0.302854899009995,56.7115907454141));
#22733=CARTESIAN_POINT('Ctrl Pts',(6.75015930678691,0.477114591055564,56.7197980001445));
#22734=CARTESIAN_POINT('Ctrl Pts',(6.7378495943166,0.651270908537818,56.7280003861565));
#22735=CARTESIAN_POINT('Ctrl Pts',(6.71878828214661,0.82505429500201,56.7362027721684));
#22736=CARTESIAN_POINT('Ctrl Pts',(6.69301683849192,0.997905105540422,56.7444051581804));
#22737=CARTESIAN_POINT('Ctrl Pts',(6.66725308698803,1.17070432430472,56.7526050959791));
#22738=CARTESIAN_POINT('Ctrl Pts',(6.63478324245407,1.34257116708588,56.7608050337778));
#22739=CARTESIAN_POINT('Ctrl Pts',(6.59570056008811,1.51295179092179,56.7690049715765));
#22740=CARTESIAN_POINT('Ctrl Pts',(6.55662334248996,1.68330859114856,56.7772037628122));
#22741=CARTESIAN_POINT('Ctrl Pts',(6.51093520792635,1.85217923690409,56.785402554048));
#22742=CARTESIAN_POINT('Ctrl Pts',(6.45878040288734,2.01902072977927,56.7936013452837));
#22743=CARTESIAN_POINT('Ctrl Pts',(6.40662342928366,2.185869159821,56.8018004774201));
#22744=CARTESIAN_POINT('Ctrl Pts',(6.34799935640286,2.35068792675093,56.8099996095566));
#22745=CARTESIAN_POINT('Ctrl Pts',(6.28310213308798,2.51294977768862,56.818198741693));
#22746=CARTESIAN_POINT('Ctrl Pts',(6.21819043873685,2.67524781040739,56.8263997021039));
#22747=CARTESIAN_POINT('Ctrl Pts',(6.14700294099896,2.83498745882719,56.8346006625148));
#22748=CARTESIAN_POINT('Ctrl Pts',(6.06978151960589,2.99166196356654,56.8428016229257));
#22749=CARTESIAN_POINT('Ctrl Pts',(5.99248772315154,3.14848331003294,56.8510102696108));
#22750=CARTESIAN_POINT('Ctrl Pts',(5.9091488628883,3.30223345126376,56.8592189162958));
#22751=CARTESIAN_POINT('Ctrl Pts',(5.82005298481939,3.45242990571784,56.8674275629809));
#22752=CARTESIAN_POINT('Ctrl Pts',(5.73091456987614,3.60269806817737,56.8756401287044));
#22753=CARTESIAN_POINT('Ctrl Pts',(5.63601385153254,3.74940886027348,56.8838526944278));
#22754=CARTESIAN_POINT('Ctrl Pts',(5.53568187272827,3.89210935148895,56.8920652601513));
#22755=CARTESIAN_POINT('Ctrl Pts',(5.43521222397096,4.03500564837034,56.9002890947001));
#22756=CARTESIAN_POINT('Ctrl Pts',(5.3292966380478,4.17388036182298,56.9085129292489));
#22757=CARTESIAN_POINT('Ctrl Pts',(5.21830683100648,4.30831322183881,56.9167367637976));
#22758=CARTESIAN_POINT('Ctrl Pts',(5.11632807649764,4.43183173218608,56.9242929207721));
#22759=CARTESIAN_POINT('Ctrl Pts',(5.01006618032121,4.55160060682997,56.9318490777466));
#22760=CARTESIAN_POINT('Ctrl Pts',(4.89983590488299,4.66732226284189,56.939405234721));
#22761=CARTESIAN_POINT('Ctrl Pts',(4.77037908012015,4.80322828397848,56.9482793492547));
#22762=CARTESIAN_POINT('Ctrl Pts',(4.63514552804324,4.9338696802297,56.9571534637885));
#22763=CARTESIAN_POINT('Ctrl Pts',(4.494581686238,5.0587572056518,56.9660275783222));
#22764=CARTESIAN_POINT('Ctrl Pts',(4.35783563105977,5.18025272130586,56.9746606673165));
#22765=CARTESIAN_POINT('Ctrl Pts',(4.21604527949635,5.29630258905356,56.9832937563108));
#22766=CARTESIAN_POINT('Ctrl Pts',(4.0696609981487,5.40649131693998,56.9919268453051));
#22767=CARTESIAN_POINT('Ctrl Pts',(3.91714640520632,5.52129455145204,57.0009214726086));
#22768=CARTESIAN_POINT('Ctrl Pts',(3.75964502175002,5.62973490596909,57.009916099912));
#22769=CARTESIAN_POINT('Ctrl Pts',(3.59770745665002,5.73138639915028,57.0189107272154));
#22770=CARTESIAN_POINT('Ctrl Pts',(3.43576989154996,5.83303789233151,57.0279053545189));
#22771=CARTESIAN_POINT('Ctrl Pts',(3.26939643015181,5.92790027351654,57.0368999818223));
#22772=CARTESIAN_POINT('Ctrl Pts',(3.09917575053259,6.01559628526639,57.0458946091257));
#22773=CARTESIAN_POINT('Ctrl Pts',(3.09917575053258,6.01559628526639,55.0458595242204));
#22774=CARTESIAN_POINT('Ctrl Pts',(2.94439360812047,6.09533851523518,55.0540784634639));
#22775=CARTESIAN_POINT('Ctrl Pts',(2.78634971423239,6.16919687680001,55.0622974027074));
#22776=CARTESIAN_POINT('Ctrl Pts',(2.62553110980132,6.23689629474993,55.0705163419508));
#22777=CARTESIAN_POINT('Ctrl Pts',(2.46486086366275,6.30453325866921,55.0787276990629));
#22778=CARTESIAN_POINT('Ctrl Pts',(2.30142133292268,6.36602245613136,55.0869390561749));
#22779=CARTESIAN_POINT('Ctrl Pts',(2.13572376068943,6.42113486994524,55.0951504132869));
#22780=CARTESIAN_POINT('Ctrl Pts',(1.97014586454737,6.47620747847909,55.1033558396958));
#22781=CARTESIAN_POINT('Ctrl Pts',(1.80231351396567,6.52491236430631,55.1115612661046));
#22782=CARTESIAN_POINT('Ctrl Pts',(1.63275760578661,6.5670687220971,55.1197666925134));
#22783=CARTESIAN_POINT('Ctrl Pts',(1.46329021233422,6.60920307264244,55.1279678353731));
#22784=CARTESIAN_POINT('Ctrl Pts',(1.29210140067427,6.64479561916022,55.1361689782327));
#22785=CARTESIAN_POINT('Ctrl Pts',(1.11973698256718,6.67371546365826,55.1443701210923));
#22786=CARTESIAN_POINT('Ctrl Pts',(0.941198440117324,6.7036712221684,55.1528650303588));
#22787=CARTESIAN_POINT('Ctrl Pts',(0.761398889731606,6.72646726241169,55.1613599396252));
#22788=CARTESIAN_POINT('Ctrl Pts',(0.580956816055468,6.74201588383465,55.1698548488916));
#22789=CARTESIAN_POINT('Ctrl Pts',(0.40679692454045,6.75702317212979,55.1780540035906));
#22790=CARTESIAN_POINT('Ctrl Pts',(0.232038878029628,6.76527918081022,55.1862531582896));
#22791=CARTESIAN_POINT('Ctrl Pts',(0.0572440019946399,6.76675787391833,
55.1944523129886));
#22792=CARTESIAN_POINT('Ctrl Pts',(-0.117571233752477,6.76823673926126,
55.2026524227065));
#22793=CARTESIAN_POINT('Ctrl Pts',(-0.292422949038723,6.76293671292917,
55.2108525324245));
#22794=CARTESIAN_POINT('Ctrl Pts',(-0.466749923568456,6.75088390574515,
55.2190526421425));
#22795=CARTESIAN_POINT('Ctrl Pts',(-0.641128828132783,6.73882750816615,
55.2272551945804));
#22796=CARTESIAN_POINT('Ctrl Pts',(-0.814982323011746,6.72001434722957,
55.2354577470184));
#22797=CARTESIAN_POINT('Ctrl Pts',(-0.98775435508373,6.69452241269033,55.2436602994563));
#22798=CARTESIAN_POINT('Ctrl Pts',(-1.16060919733535,6.6690182597865,55.2518667834035));
#22799=CARTESIAN_POINT('Ctrl Pts',(-1.33238119003697,6.6368290086569,55.2600732673507));
#22800=CARTESIAN_POINT('Ctrl Pts',(-1.50252445657173,6.5980837564708,55.2682797512978));
#22801=CARTESIAN_POINT('Ctrl Pts',(-1.67286916646132,6.55929263133455,55.2764959514195));
#22802=CARTESIAN_POINT('Ctrl Pts',(-1.84158094989867,6.51393008400835,55.2847121515411));
#22803=CARTESIAN_POINT('Ctrl Pts',(-2.00812818465421,6.46217534534598,55.2929283516627));
#22804=CARTESIAN_POINT('Ctrl Pts',(-2.17479235022103,6.41038427030379,55.3011503202797));
#22805=CARTESIAN_POINT('Ctrl Pts',(-2.33928860165323,6.35219217846584,55.3093722888966));
#22806=CARTESIAN_POINT('Ctrl Pts',(-2.5011054099358,6.28782639140028,55.3175942575136));
#22807=CARTESIAN_POINT('Ctrl Pts',(-2.66314387204506,6.22337243720819,55.325827488439));
#22808=CARTESIAN_POINT('Ctrl Pts',(-2.82249523650154,6.15272804690666,55.3340607193644));
#22809=CARTESIAN_POINT('Ctrl Pts',(-2.97867190289986,6.07616677642039,55.3422939502898));
#22810=CARTESIAN_POINT('Ctrl Pts',(-3.01631912457594,6.05771127222588,55.3442786146888));
#22811=CARTESIAN_POINT('Ctrl Pts',(-3.05378200236287,6.03891215075457,55.3462632790878));
#22812=CARTESIAN_POINT('Ctrl Pts',(-3.09105396253018,6.01977361706622,55.3482479434869));
#22813=CARTESIAN_POINT('Ctrl Pts',(-3.2441839043967,5.94114393035398,55.3564018356536));
#22814=CARTESIAN_POINT('Ctrl Pts',(-3.39456247297689,5.85653868877348,55.3645557278203));
#22815=CARTESIAN_POINT('Ctrl Pts',(-3.54168471217314,5.76617363591828,55.3727096199871));
#22816=CARTESIAN_POINT('Ctrl Pts',(-3.68862742113394,5.67591885367413,55.3808535621273));
#22817=CARTESIAN_POINT('Ctrl Pts',(-3.83232140220006,5.57991843998532,55.3889975042675));
#22818=CARTESIAN_POINT('Ctrl Pts',(-3.9722832661189,5.47843542023741,55.3971414464077));
#22819=CARTESIAN_POINT('Ctrl Pts',(-4.11210379664129,5.37705487797486,55.4052771648006));
#22820=CARTESIAN_POINT('Ctrl Pts',(-4.24819941893756,5.27020296442739,55.4134128831935));
#22821=CARTESIAN_POINT('Ctrl Pts',(-4.38011288995688,5.15818767313032,55.4215486015864));
#22822=CARTESIAN_POINT('Ctrl Pts',(-4.51192090287179,5.04626193235598,55.4296778158867));
#22823=CARTESIAN_POINT('Ctrl Pts',(-4.63955314418621,4.9291812683987,55.4378070301869));
#22824=CARTESIAN_POINT('Ctrl Pts',(-4.76258284177514,4.80729587972584,55.4459362444871));
#22825=CARTESIAN_POINT('Ctrl Pts',(-4.88554005190463,4.68548230430085,55.4540606691626));
#22826=CARTESIAN_POINT('Ctrl Pts',(-5.00389985955734,4.55886989843988,55.462185093838));
#22827=CARTESIAN_POINT('Ctrl Pts',(-5.11726998927648,4.42784788095191,55.4703095185134));
#22828=CARTESIAN_POINT('Ctrl Pts',(-5.23132834825853,4.29603047594216,55.4784832636476));
#22829=CARTESIAN_POINT('Ctrl Pts',(-5.34033596388518,4.15974998873474,55.4866570087817));
#22830=CARTESIAN_POINT('Ctrl Pts',(-5.4439319762056,4.01943946819033,55.4948307539159));
#22831=CARTESIAN_POINT('Ctrl Pts',(-5.54686458997772,3.88002745516137,55.5029521567781));
#22832=CARTESIAN_POINT('Ctrl Pts',(-5.64445450512135,3.7366371837638,55.5110735596402));
#22833=CARTESIAN_POINT('Ctrl Pts',(-5.73638923462593,3.58972527484593,55.5191949625024));
#22834=CARTESIAN_POINT('Ctrl Pts',(-5.82833107203969,3.44280200747288,55.5273169932686));
#22835=CARTESIAN_POINT('Ctrl Pts',(-5.91461665870489,3.29235687046016,55.5354390240349));
#22836=CARTESIAN_POINT('Ctrl Pts',(-5.99497791594782,3.13887380875657,55.5435610548012));
#22837=CARTESIAN_POINT('Ctrl Pts',(-6.07536068893902,2.98534965383178,55.5516852601423));
#22838=CARTESIAN_POINT('Ctrl Pts',(-6.14981580447394,2.82878627875354,55.5598094654834));
#22839=CARTESIAN_POINT('Ctrl Pts',(-6.2181220707769,2.66969041518249,55.5679336708245));
#22840=CARTESIAN_POINT('Ctrl Pts',(-6.28716770514826,2.50887244897422,55.5761458150669));
#22841=CARTESIAN_POINT('Ctrl Pts',(-6.3499304463994,2.34546720131573,55.5843579593094));
#22842=CARTESIAN_POINT('Ctrl Pts',(-6.40623284922578,2.18001598193695,55.5925701035518));
#22843=CARTESIAN_POINT('Ctrl Pts',(-6.46202127316779,2.01607514983982,55.6007072799682));
#22844=CARTESIAN_POINT('Ctrl Pts',(-6.51146677541545,1.85012591390681,55.6088444563847));
#22845=CARTESIAN_POINT('Ctrl Pts',(-6.55444781601728,1.68270699383651,55.6169816328011));
#22846=CARTESIAN_POINT('Ctrl Pts',(-6.59802283326526,1.51297442739444,55.6252312609565));
#22847=CARTESIAN_POINT('Ctrl Pts',(-6.63495332642006,1.34173164236327,55.6334808891119));
#22848=CARTESIAN_POINT('Ctrl Pts',(-6.66516684415941,1.16954689496323,55.6417305172673));
#22849=CARTESIAN_POINT('Ctrl Pts',(-6.69538036189876,0.9973621475632,55.6499801454227));
#22850=CARTESIAN_POINT('Ctrl Pts',(-6.71887691516152,0.824235827583319,
55.6582297735781));
#22851=CARTESIAN_POINT('Ctrl Pts',(-6.73563879448179,0.650737297434142,
55.6664794017335));
#22852=CARTESIAN_POINT('Ctrl Pts',(-6.7564314932459,0.435516640819393,55.6767128624256));
#22853=CARTESIAN_POINT('Ctrl Pts',(-6.76690867697218,0.219312224909553,
55.6869463231178));
#22854=CARTESIAN_POINT('Ctrl Pts',(-6.76699940565911,0.00283616100313801,
55.69717978381));
#22855=CARTESIAN_POINT('',(-6.76699999332355,-0.000300597867382727,55.3028202161605));
#22856=CARTESIAN_POINT('Ctrl Pts',(3.09917575053251,6.01559628526643,54.6513758699904));
#22857=CARTESIAN_POINT('Ctrl Pts',(3.03170056831351,6.05035883224919,54.6549639060335));
#22858=CARTESIAN_POINT('Ctrl Pts',(2.96367868074345,6.08396626315161,54.6585519420766));
#22859=CARTESIAN_POINT('Ctrl Pts',(2.8951533392384,6.11640222208258,54.6621399781197));
#22860=CARTESIAN_POINT('Ctrl Pts',(2.73945348228504,6.19010158723388,54.6702925343329));
#22861=CARTESIAN_POINT('Ctrl Pts',(2.58069410409827,6.25796707530155,54.6784450905462));
#22862=CARTESIAN_POINT('Ctrl Pts',(2.41935558589252,6.31973160419101,54.6865976467594));
#22863=CARTESIAN_POINT('Ctrl Pts',(2.25820398224972,6.38142457738471,54.6947407580398));
#22864=CARTESIAN_POINT('Ctrl Pts',(2.09447952438987,6.43703053178444,54.7028838693201));
#22865=CARTESIAN_POINT('Ctrl Pts',(1.92868669728718,6.48632843939524,54.7110269806005));
#22866=CARTESIAN_POINT('Ctrl Pts',(1.76305108929455,6.5355795984627,54.7191623698778));
#22867=CARTESIAN_POINT('Ctrl Pts',(1.5953513649588,6.57853451633816,54.7272977591551));
#22868=CARTESIAN_POINT('Ctrl Pts',(1.42611147686499,6.61502041233086,54.7354331484325));
#22869=CARTESIAN_POINT('Ctrl Pts',(1.25699651529884,6.65147937580579,54.7435625324711));
#22870=CARTESIAN_POINT('Ctrl Pts',(1.08634400956924,6.68147874892201,54.7516919165097));
#22871=CARTESIAN_POINT('Ctrl Pts',(0.914692545464687,6.7048957148692,54.7598213005483));
#22872=CARTESIAN_POINT('Ctrl Pts',(0.743131733005261,6.72830031397467,54.7679463913404));
#22873=CARTESIAN_POINT('Ctrl Pts',(0.570573374236173,6.74512937973692,54.7760714821325));
#22874=CARTESIAN_POINT('Ctrl Pts',(0.397565704887895,6.75531128152486,54.7841965729247));
#22875=CARTESIAN_POINT('Ctrl Pts',(0.22389762775997,6.76553204983922,54.7923526789498));
#22876=CARTESIAN_POINT('Ctrl Pts',(0.049777168539924,6.76905473590006,54.8005087849749));
#22877=CARTESIAN_POINT('Ctrl Pts',(-0.124235975849758,6.76585947402876,
54.808664891));
#22878=CARTESIAN_POINT('Ctrl Pts',(-0.297548748803826,6.76267707250862,
54.8167881701735));
#22879=CARTESIAN_POINT('Ctrl Pts',(-0.470754701295699,6.75283072801071,
54.8249114493468));
#22880=CARTESIAN_POINT('Ctrl Pts',(-0.643301263867664,6.7363530551706,54.8330347285203));
#22881=CARTESIAN_POINT('Ctrl Pts',(-0.815870802472411,6.71987318818912,
54.8411590893769));
#22882=CARTESIAN_POINT('Ctrl Pts',(-0.987780412063691,6.69676026883925,
54.8492834502336));
#22883=CARTESIAN_POINT('Ctrl Pts',(-1.15848317996609,6.66709874846141,54.8574078110903));
#22884=CARTESIAN_POINT('Ctrl Pts',(-1.32924115546454,6.63742763514459,54.8655347994757));
#22885=CARTESIAN_POINT('Ctrl Pts',(-1.49879115180774,6.60120376597276,54.8736617878611));
#22886=CARTESIAN_POINT('Ctrl Pts',(-1.66659701485307,6.5585626009121,54.8817887762466));
#22887=CARTESIAN_POINT('Ctrl Pts',(-1.83548772369796,6.5156457655741,54.8899683046866));
#22888=CARTESIAN_POINT('Ctrl Pts',(-2.00261130556678,6.46622846506356,54.8981478331267));
#22889=CARTESIAN_POINT('Ctrl Pts',(-2.16743807252027,6.41049929426637,54.9063273615668));
#22890=CARTESIAN_POINT('Ctrl Pts',(-2.33148861709045,6.35503257010073,54.9144683699705));
#22891=CARTESIAN_POINT('Ctrl Pts',(-2.49326361463911,6.29331348729231,54.9226093783741));
#22892=CARTESIAN_POINT('Ctrl Pts',(-2.65226262308908,6.22557563428191,54.9307503867778));
#22893=CARTESIAN_POINT('Ctrl Pts',(-2.81239011230343,6.15735701812156,54.9389491752361));
#22894=CARTESIAN_POINT('Ctrl Pts',(-2.96970172158162,6.08303404365845,54.9471479636944));
#22895=CARTESIAN_POINT('Ctrl Pts',(-3.12371347702433,6.00289122952071,54.9553467521526));
#22896=CARTESIAN_POINT('Ctrl Pts',(-3.27772523246704,5.92274841538296,54.9635455406109));
#22897=CARTESIAN_POINT('Ctrl Pts',(-3.42843684358858,5.83678600183742,54.9717443290691));
#22898=CARTESIAN_POINT('Ctrl Pts',(-3.5753961880223,5.74533124359907,54.9799431175274));
#22899=CARTESIAN_POINT('Ctrl Pts',(-3.72296965649872,5.6534943077859,54.9881761676594));
#22900=CARTESIAN_POINT('Ctrl Pts',(-3.86721823322404,5.55583365106446,54.9964092177914));
#22901=CARTESIAN_POINT('Ctrl Pts',(-4.00765146065182,5.45261577318037,55.0046422679234));
#22902=CARTESIAN_POINT('Ctrl Pts',(-4.14791745369263,5.34952081192255,55.0128655137583));
#22903=CARTESIAN_POINT('Ctrl Pts',(-4.28437685887732,5.24088201721773,55.0210887595931));
#22904=CARTESIAN_POINT('Ctrl Pts',(-4.41656519971276,5.12701090662837,55.029312005428));
#22905=CARTESIAN_POINT('Ctrl Pts',(-4.54862258233521,5.01325260747955,55.0375271045415));
#22906=CARTESIAN_POINT('Ctrl Pts',(-4.67641705782021,4.89427254786337,55.045742203655));
#22907=CARTESIAN_POINT('Ctrl Pts',(-4.79951438540531,4.77042457903775,55.0539573027685));
#22908=CARTESIAN_POINT('Ctrl Pts',(-4.9225143904864,4.64667452618382,55.0621659069074));
#22909=CARTESIAN_POINT('Ctrl Pts',(-5.04082439311391,4.51806448273646,55.0703745110463));
#22910=CARTESIAN_POINT('Ctrl Pts',(-5.15404435826846,4.38498754308391,55.0785831151852));
#22911=CARTESIAN_POINT('Ctrl Pts',(-5.26719745725208,4.25198919686126,55.0867868714341));
#22912=CARTESIAN_POINT('Ctrl Pts',(-5.37526627585814,4.11452948193927,55.0949906276831));
#22913=CARTESIAN_POINT('Ctrl Pts',(-5.47788863137583,3.97303726917373,55.1031943839321));
#22914=CARTESIAN_POINT('Ctrl Pts',(-5.58048062352503,3.83158692038776,55.1113957128964));
#22915=CARTESIAN_POINT('Ctrl Pts',(-5.67762914942449,3.68610673771275,55.1195970418606));
#22916=CARTESIAN_POINT('Ctrl Pts',(-5.76901307699329,3.53705769213345,55.1277983708249));
#22917=CARTESIAN_POINT('Ctrl Pts',(-5.86038440184607,3.38802920184045,55.1359985687476));
#22918=CARTESIAN_POINT('Ctrl Pts',(-5.94599252382731,3.23543313381405,55.1441987666703));
#22919=CARTESIAN_POINT('Ctrl Pts',(-6.02556032163339,3.07975840129666,55.152398964593));
#22920=CARTESIAN_POINT('Ctrl Pts',(-6.1051315655844,2.92407692638214,55.1605995176729));
#22921=CARTESIAN_POINT('Ctrl Pts',(-6.17866180104383,2.7653168403509,55.1688000707527));
#22922=CARTESIAN_POINT('Ctrl Pts',(-6.24592042595145,2.6039905976563,55.1770006238325));
#22923=CARTESIAN_POINT('Ctrl Pts',(-6.31319415246435,2.44262813231754,55.1852030181858));
#22924=CARTESIAN_POINT('Ctrl Pts',(-6.3741933259118,2.27869869335459,55.193405412539));
#22925=CARTESIAN_POINT('Ctrl Pts',(-6.42873592055473,2.11273364714281,55.2016078068922));
#22926=CARTESIAN_POINT('Ctrl Pts',(-6.4833295221116,1.9466133944381,55.209817871926));
#22927=CARTESIAN_POINT('Ctrl Pts',(-6.53145436936603,1.77845407196468,55.2180279369598));
#22928=CARTESIAN_POINT('Ctrl Pts',(-6.57297840188812,1.60880201650555,55.2262380019937));
#22929=CARTESIAN_POINT('Ctrl Pts',(-6.61452230707553,1.43906876858232,55.234451996219));
#22930=CARTESIAN_POINT('Ctrl Pts',(-6.64945902734759,1.26784171414278,55.2426659904443));
#22931=CARTESIAN_POINT('Ctrl Pts',(-6.67770789282387,1.09567618305674,55.2508799846696));
#22932=CARTESIAN_POINT('Ctrl Pts',(-6.70599527091237,0.923275933010371,
55.2591051773048));
#22933=CARTESIAN_POINT('Ctrl Pts',(-6.727576527936,0.749935004945466,55.26733036994));
#22934=CARTESIAN_POINT('Ctrl Pts',(-6.74242290182665,0.576213860405586,
55.2755555625752));
#22935=CARTESIAN_POINT('Ctrl Pts',(-6.75577421406819,0.419986807201015,
55.2829524606951));
#22936=CARTESIAN_POINT('Ctrl Pts',(-6.76367947340974,0.263452476255881,
55.290349358815));
#22937=CARTESIAN_POINT('Ctrl Pts',(-6.76615373703693,0.107016852790295,
55.2977462569349));
#22938=CARTESIAN_POINT('Ctrl Pts',(-6.76671948376637,0.0712474459374166,
55.2994375766768));
#22939=CARTESIAN_POINT('Ctrl Pts',(-6.76700158246802,0.0354739095168925,
55.3011288964187));
#22940=CARTESIAN_POINT('Ctrl Pts',(-6.76699999332355,-0.000300597867481069,
55.3028202161605));
#22941=CARTESIAN_POINT('Ctrl Pts',(-6.76699999332352,-0.000300598487863234,
55.3028202161898));
#22942=CARTESIAN_POINT('Ctrl Pts',(-6.7669919378939,-0.181642469414841,
55.3113935581795));
#22943=CARTESIAN_POINT('Ctrl Pts',(-6.75969016719996,-0.363162940377724,
55.3199669001692));
#22944=CARTESIAN_POINT('Ctrl Pts',(-6.74507751209151,-0.544259456396834,
55.3285402421589));
#22945=CARTESIAN_POINT('Ctrl Pts',(-6.73048339037461,-0.725126285708546,
55.3371027104845));
#22946=CARTESIAN_POINT('Ctrl Pts',(-6.70859689518945,-0.905569919651554,
55.34566517881));
#22947=CARTESIAN_POINT('Ctrl Pts',(-6.67945284379024,-1.08498788361092,
55.3542276471356));
#22948=CARTESIAN_POINT('Ctrl Pts',(-6.65035580230743,-1.26411644293771,
55.3627763040348));
#22949=CARTESIAN_POINT('Ctrl Pts',(-6.61402461003255,-1.44222232324766,
55.3713249609339));
#22950=CARTESIAN_POINT('Ctrl Pts',(-6.57054578095658,-1.61870847911341,
55.3798736178331));
#22951=CARTESIAN_POINT('Ctrl Pts',(-6.52710837203152,-1.79502650526263,
55.3884141308456));
#22952=CARTESIAN_POINT('Ctrl Pts',(-6.47653697394261,-1.96972757813517,
55.396954643858));
#22953=CARTESIAN_POINT('Ctrl Pts',(-6.4189693188722,-2.14222358389066,55.4054951568705));
#22954=CARTESIAN_POINT('Ctrl Pts',(-6.36146978187363,-2.31451548031953,
55.4140255641512));
#22955=CARTESIAN_POINT('Ctrl Pts',(-6.29699060257995,-2.48460721701655,
55.4225559714319));
#22956=CARTESIAN_POINT('Ctrl Pts',(-6.22571961560228,-2.65192463465782,
55.4310863787127));
#22957=CARTESIAN_POINT('Ctrl Pts',(-6.15453154832205,-2.81904738809932,
55.4396068613548));
#22958=CARTESIAN_POINT('Ctrl Pts',(-6.07656756443147,-2.98340197460336,
55.4481273439968));
#22959=CARTESIAN_POINT('Ctrl Pts',(-5.99206411720368,-3.14443263806367,
55.4566478266389));
#22960=CARTESIAN_POINT('Ctrl Pts',(-5.90681411731338,-3.30688594017953,
55.4652435841865));
#22961=CARTESIAN_POINT('Ctrl Pts',(-5.81500381503648,-3.46577502039305,
55.4738393417341));
#22962=CARTESIAN_POINT('Ctrl Pts',(-5.71696406270463,-3.62058157009945,
55.4824350992816));
#22963=CARTESIAN_POINT('Ctrl Pts',(-5.61883283595042,-3.77553255958026,
55.4910388769632));
#22964=CARTESIAN_POINT('Ctrl Pts',(-5.51446072094989,-3.92639315744197,
55.4996426546449));
#22965=CARTESIAN_POINT('Ctrl Pts',(-5.40422100295438,-4.07267533093748,
55.5082464323265));
#22966=CARTESIAN_POINT('Ctrl Pts',(-5.28964876764329,-4.22470652176681,
55.5171883459945));
#22967=CARTESIAN_POINT('Ctrl Pts',(-5.16873863590604,-4.37179184566761,
55.5261302596625));
#22968=CARTESIAN_POINT('Ctrl Pts',(-5.04195356579148,-4.51342367171558,
55.5350721733305));
#22969=CARTESIAN_POINT('Ctrl Pts',(-4.9196307059426,-4.65007075478422,55.5436993756612));
#22970=CARTESIAN_POINT('Ctrl Pts',(-4.79183963920985,-4.78164149138373,
55.5523265779919));
#22971=CARTESIAN_POINT('Ctrl Pts',(-4.65903206133329,-4.90771935337266,
55.5609537803227));
#22972=CARTESIAN_POINT('Ctrl Pts',(-4.52609800456668,-5.03391728522732,
55.5695891987431));
#22973=CARTESIAN_POINT('Ctrl Pts',(-4.38813812777909,-5.15461169769776,
55.5782246171636));
#22974=CARTESIAN_POINT('Ctrl Pts',(-4.24563705091085,-5.26942644240652,
55.586860035584));
#22975=CARTESIAN_POINT('Ctrl Pts',(-4.10292544899946,-5.38441080954632,
55.5955082116051));
#22976=CARTESIAN_POINT('Ctrl Pts',(-3.95565948263147,-5.49349796567173,
55.6041563876262));
#22977=CARTESIAN_POINT('Ctrl Pts',(-3.8043537739338,-5.59635429210443,55.6128045636474));
#22978=CARTESIAN_POINT('Ctrl Pts',(-3.78834620365939,-5.60723610144071,
55.6137195078791));
#22979=CARTESIAN_POINT('Ctrl Pts',(-3.77229344066174,-5.61804821207019,
55.6146344521109));
#22980=CARTESIAN_POINT('Ctrl Pts',(-3.75619611061305,-5.62879025889359,
55.6155493963426));
#22981=CARTESIAN_POINT('Ctrl Pts',(-3.61146978487512,-5.72536881962095,
55.6237753888839));
#22982=CARTESIAN_POINT('Ctrl Pts',(-3.4628263023278,-5.81648879399469,55.6320013814253));
#22983=CARTESIAN_POINT('Ctrl Pts',(-3.31071505867864,-5.90181792333841,
55.6402273739666));
#22984=CARTESIAN_POINT('Ctrl Pts',(-3.1587632840073,-5.98705759611923,55.6484447426181));
#22985=CARTESIAN_POINT('Ctrl Pts',(-3.00335129777346,-6.06651833953246,
55.6566621112695));
#22986=CARTESIAN_POINT('Ctrl Pts',(-2.84495823010512,-6.13991055870989,
55.6648794799209));
#22987=CARTESIAN_POINT('Ctrl Pts',(-2.68669952332861,-6.21324052109687,
55.6730898779833));
#22988=CARTESIAN_POINT('Ctrl Pts',(-2.52546509477776,-6.28051206195501,
55.6813002760457));
#22989=CARTESIAN_POINT('Ctrl Pts',(-2.36175956934444,-6.34148095767937,
55.6895106741081));
#22990=CARTESIAN_POINT('Ctrl Pts',(-2.19816016368635,-6.40241033118543,
55.6977157498968));
#22991=CARTESIAN_POINT('Ctrl Pts',(-2.03209318647946,-6.45704507317781,
55.7059208256856));
#22992=CARTESIAN_POINT('Ctrl Pts',(-1.86408427121,-6.50518860832086,55.7141259014744));
#22993=CARTESIAN_POINT('Ctrl Pts',(-1.69615066376803,-6.55331056374575,
55.7223272994439));
#22994=CARTESIAN_POINT('Ctrl Pts',(-1.52627719615885,-6.59494701060637,
55.7305286974133));
#22995=CARTESIAN_POINT('Ctrl Pts',(-1.35500582168781,-6.62995084621237,
55.7387300953828));
#22996=CARTESIAN_POINT('Ctrl Pts',(-1.1837478626166,-6.66495194002658,55.7469308509505));
#22997=CARTESIAN_POINT('Ctrl Pts',(-1.01109256379185,-6.69332137718182,
55.7551316065182));
#22998=CARTESIAN_POINT('Ctrl Pts',(-0.837593635799518,-6.71496283692383,
55.763332362086));
#22999=CARTESIAN_POINT('Ctrl Pts',(-0.66409558909929,-6.73660418673752,
55.7715330759977));
#23000=CARTESIAN_POINT('Ctrl Pts',(-0.489754277252908,-6.75151758179396,
55.7797337899095));
#23001=CARTESIAN_POINT('Ctrl Pts',(-0.315130006418644,-6.75965842917041,
55.7879345038213));
#23002=CARTESIAN_POINT('Ctrl Pts',(-0.140474976326381,-6.7678007105195,
55.7961366622509));
#23003=CARTESIAN_POINT('Ctrl Pts',(0.03446275406608,-6.76916805074496,55.8043388206805));
#23004=CARTESIAN_POINT('Ctrl Pts',(0.209121334914704,-6.76376797852229,
55.8125409791101));
#23005=CARTESIAN_POINT('Ctrl Pts',(0.383842333883037,-6.75836597646398,
55.8207460687631));
#23006=CARTESIAN_POINT('Ctrl Pts',(0.5582836266049,-6.7461917552627,55.828951158416));
#23007=CARTESIAN_POINT('Ctrl Pts',(0.731886885323504,-6.72730485314078,
55.8371562480689));
#23008=CARTESIAN_POINT('Ctrl Pts',(0.905688465239941,-6.7083963749662,55.8453707110667));
#23009=CARTESIAN_POINT('Ctrl Pts',(1.07864974189527,-6.68275993446701,55.8535851740645));
#23010=CARTESIAN_POINT('Ctrl Pts',(1.25021994594242,-6.65050667895069,55.8617996370623));
#23011=CARTESIAN_POINT('Ctrl Pts',(1.42189179991283,-6.61823431439988,55.8700189668697));
#23012=CARTESIAN_POINT('Ctrl Pts',(1.5921705896081,-6.57933739993316,55.8782382966772));
#23013=CARTESIAN_POINT('Ctrl Pts',(1.76051927672503,-6.53397741626642,55.8864576264847));
#23014=CARTESIAN_POINT('Ctrl Pts',(1.92912880992589,-6.4885471500551,55.8946896916454));
#23015=CARTESIAN_POINT('Ctrl Pts',(2.09580192228886,-6.43663390899524,55.9029217568061));
#23016=CARTESIAN_POINT('Ctrl Pts',(2.26001890768737,-6.37844836436696,55.9111538219667));
#23017=CARTESIAN_POINT('Ctrl Pts',(2.40762892559136,-6.32614701890327,55.918553393228));
#23018=CARTESIAN_POINT('Ctrl Pts',(2.55325456856072,-6.26877855995937,55.9259529644892));
#23019=CARTESIAN_POINT('Ctrl Pts',(2.69653527350191,-6.20652773447118,55.9333525357504));
#23020=CARTESIAN_POINT('Ctrl Pts',(2.85445250794638,-6.13791781098557,55.9415079941572));
#23021=CARTESIAN_POINT('Ctrl Pts',(3.01000707065127,-6.06316503924268,55.9496634525639));
#23022=CARTESIAN_POINT('Ctrl Pts',(3.16268103959137,-5.9824524771877,55.9578189109707));
#23023=CARTESIAN_POINT('Ctrl Pts',(3.31516918424258,-5.90183815293024,55.9659644431126));
#23024=CARTESIAN_POINT('Ctrl Pts',(3.46478339452723,-5.81527864642458,55.9741099752545));
#23025=CARTESIAN_POINT('Ctrl Pts',(3.61102424978326,-5.7230055798922,55.9822555073964));
#23026=CARTESIAN_POINT('Ctrl Pts',(3.75711786221345,-5.63082541863613,55.990392838197));
#23027=CARTESIAN_POINT('Ctrl Pts',(3.89984457457807,-5.53294334355425,55.9985301689975));
#23028=CARTESIAN_POINT('Ctrl Pts',(4.03872818351032,-5.42963752562908,56.0066674997981));
#23029=CARTESIAN_POINT('Ctrl Pts',(4.17750114409153,-5.32641401128526,56.0147983476001));
#23030=CARTESIAN_POINT('Ctrl Pts',(4.31243680575048,-5.21777557504684,56.0229291954021));
#23031=CARTESIAN_POINT('Ctrl Pts',(4.44308667312931,-5.10404445661093,56.0310600432041));
#23032=CARTESIAN_POINT('Ctrl Pts',(4.57365989723239,-4.99038005638641,56.0391861211979));
#23033=CARTESIAN_POINT('Ctrl Pts',(4.69995205900485,-4.87162916294331,56.0473121991917));
#23034=CARTESIAN_POINT('Ctrl Pts',(4.82154659059871,-4.74815516539698,56.0554382771855));
#23035=CARTESIAN_POINT('Ctrl Pts',(4.9435722741931,-4.62424335160712,56.0635931687677));
#23036=CARTESIAN_POINT('Ctrl Pts',(5.06086665791248,-4.49557510456205,56.0717480603499));
#23037=CARTESIAN_POINT('Ctrl Pts',(5.17304458199475,-4.36255644693508,56.0799029519321));
#23038=CARTESIAN_POINT('Ctrl Pts',(5.28478505139497,-4.23005651556423,56.0880260422884));
#23039=CARTESIAN_POINT('Ctrl Pts',(5.39144866997132,-4.09324033547733,56.0961491326447));
#23040=CARTESIAN_POINT('Ctrl Pts',(5.49269407084485,-3.95254359167686,56.104272223001));
#23041=CARTESIAN_POINT('Ctrl Pts',(5.59394742196961,-3.81183579972556,56.1123959512194));
#23042=CARTESIAN_POINT('Ctrl Pts',(5.68978149420295,-3.6672471340104,56.1205196794378));
#23043=CARTESIAN_POINT('Ctrl Pts',(5.77989747702832,-3.51924340662048,56.1286434076563));
#23044=CARTESIAN_POINT('Ctrl Pts',(5.87003768063073,-3.3711998997689,56.1367693193166));
#23045=CARTESIAN_POINT('Ctrl Pts',(5.95445654445746,-3.21973981590843,56.1448952309769));
#23046=CARTESIAN_POINT('Ctrl Pts',(6.03290057877024,-3.06535472770669,56.1530211426372));
#23047=CARTESIAN_POINT('Ctrl Pts',(6.11184627083669,-2.9099823308176,56.1611990203473));
#23048=CARTESIAN_POINT('Ctrl Pts',(6.18474027868607,-2.75164772317277,56.1693768980574));
#23049=CARTESIAN_POINT('Ctrl Pts',(6.2513732005971,-2.59087284652419,56.1775547757674));
#23050=CARTESIAN_POINT('Ctrl Pts',(6.31768809802375,-2.43086531349166,56.1856936222409));
#23051=CARTESIAN_POINT('Ctrl Pts',(6.37780147487082,-2.26844111862139,56.1938324687143));
#23052=CARTESIAN_POINT('Ctrl Pts',(6.43155700025837,-2.10413011775119,56.2019713151877));
#23053=CARTESIAN_POINT('Ctrl Pts',(6.48569921643279,-1.93863714442772,56.2101687085161));
#23054=CARTESIAN_POINT('Ctrl Pts',(6.53339166227497,-1.77123048055735,56.2183661018445));
#23055=CARTESIAN_POINT('Ctrl Pts',(6.57452702349717,-1.602461674208,56.2265634951729));
#23056=CARTESIAN_POINT('Ctrl Pts',(6.61566238471935,-1.43369286785871,56.2347608885013));
#23057=CARTESIAN_POINT('Ctrl Pts',(6.65024064706947,-1.26356229597695,56.2429582818297));
#23058=CARTESIAN_POINT('Ctrl Pts',(6.6782076362055,-1.09262608779333,56.251155675158));
#23059=CARTESIAN_POINT('Ctrl Pts',(6.70627293671529,-0.921088993566183,
56.259381884495));
#23060=CARTESIAN_POINT('Ctrl Pts',(6.72776404513952,-0.748230083283909,
56.267608093832));
#23061=CARTESIAN_POINT('Ctrl Pts',(6.7425611068047,-0.574594396948484,56.275834303169));
#23062=CARTESIAN_POINT('Ctrl Pts',(6.757341544605,-0.401153782868209,56.2840512707122));
#23063=CARTESIAN_POINT('Ctrl Pts',(6.76544288077921,-0.226938484562735,
56.2922682382554));
#23064=CARTESIAN_POINT('Ctrl Pts',(6.76679631720286,-0.0525033474156623,
56.3004852057985));
#23065=CARTESIAN_POINT('Ctrl Pts',(6.7681485047442,0.12177082985688,56.3086945911419));
#23066=CARTESIAN_POINT('Ctrl Pts',(6.76276519031299,0.296264085603788,56.3169039764853));
#23067=CARTESIAN_POINT('Ctrl Pts',(6.75062938420426,0.470416748339141,56.3251133618287));
#23068=CARTESIAN_POINT('Ctrl Pts',(6.73850234142858,0.644443654468779,56.3333168191293));
#23069=CARTESIAN_POINT('Ctrl Pts',(6.71963254398363,0.818130101146211,56.3415202764299));
#23070=CARTESIAN_POINT('Ctrl Pts',(6.69405506783194,0.990916620525424,56.3497237337305));
#23071=CARTESIAN_POINT('Ctrl Pts',(6.66849093053905,1.16361303034995,56.3579229128623));
#23072=CARTESIAN_POINT('Ctrl Pts',(6.63622613578524,1.33541009391742,56.3661220919942));
#23073=CARTESIAN_POINT('Ctrl Pts',(6.59734758540405,1.50575357790155,56.374321271126));
#23074=CARTESIAN_POINT('Ctrl Pts',(6.55847636057965,1.67606496550217,56.3825189053559));
#23075=CARTESIAN_POINT('Ctrl Pts',(6.51299393603396,1.84492296840324,56.3907165395857));
#23076=CARTESIAN_POINT('Ctrl Pts',(6.461038363333,2.01178335502092,56.3989141738155));
#23077=CARTESIAN_POINT('Ctrl Pts',(6.40908654084219,2.17863169747312,56.4071112163311));
#23078=CARTESIAN_POINT('Ctrl Pts',(6.35066260651705,2.34348236808057,56.4153082588467));
#23079=CARTESIAN_POINT('Ctrl Pts',(6.28595453639365,2.50580617095419,56.4235053013623));
#23080=CARTESIAN_POINT('Ctrl Pts',(6.22123937638624,2.66814775919728,56.4317032420051));
#23081=CARTESIAN_POINT('Ctrl Pts',(6.15023884166485,2.82796159486556,56.4399011826479));
#23082=CARTESIAN_POINT('Ctrl Pts',(6.07318913700969,2.98473829775871,56.4480991232908));
#23083=CARTESIAN_POINT('Ctrl Pts',(5.9961169865251,3.14156067224979,56.4562994521267));
#23084=CARTESIAN_POINT('Ctrl Pts',(5.91299231413938,3.29534382979463,56.4644997809627));
#23085=CARTESIAN_POINT('Ctrl Pts',(5.82409738891453,3.44560279260959,56.4727001097987));
#23086=CARTESIAN_POINT('Ctrl Pts',(5.73510983287103,3.59601832916258,56.4809089835901));
#23087=CARTESIAN_POINT('Ctrl Pts',(5.64034019428901,3.7429020251711,56.4891178573815));
#23088=CARTESIAN_POINT('Ctrl Pts',(5.54011476302192,3.88579688256432,56.4973267311729));
#23089=CARTESIAN_POINT('Ctrl Pts',(5.4398355418715,4.02876843005117,56.5055400105764));
#23090=CARTESIAN_POINT('Ctrl Pts',(5.33409490781192,4.16774658605689,56.5137532899798));
#23091=CARTESIAN_POINT('Ctrl Pts',(5.22325952987308,4.30230739064401,56.5219665693832));
#23092=CARTESIAN_POINT('Ctrl Pts',(5.11226203777377,4.43706501155704,56.5301918619987));
#23093=CARTESIAN_POINT('Ctrl Pts',(4.99615514830823,4.56739210122478,56.5384171546141));
#23094=CARTESIAN_POINT('Ctrl Pts',(4.87534336262341,4.69290060586455,56.5466424472295));
#23095=CARTESIAN_POINT('Ctrl Pts',(4.76608361491862,4.8064079716734,56.5540812363416));
#23096=CARTESIAN_POINT('Ctrl Pts',(4.6529763248279,4.91597456532653,56.5615200254537));
#23097=CARTESIAN_POINT('Ctrl Pts',(4.53634333548057,5.02134226503642,56.5689588145658));
#23098=CARTESIAN_POINT('Ctrl Pts',(4.4073677887153,5.13786038531722,56.5771848053285));
#23099=CARTESIAN_POINT('Ctrl Pts',(4.2737198578081,5.24956897061698,56.5854107960912));
#23100=CARTESIAN_POINT('Ctrl Pts',(4.13579271193453,5.35607203498135,56.5936367868539));
#23101=CARTESIAN_POINT('Ctrl Pts',(3.99800205900093,5.46246970373067,56.6018546371621));
#23102=CARTESIAN_POINT('Ctrl Pts',(3.85594090032626,5.56367188666554,56.6100724874703));
#23103=CARTESIAN_POINT('Ctrl Pts',(3.71003847747409,5.65932005594857,56.6182903377784));
#23104=CARTESIAN_POINT('Ctrl Pts',(3.5642860834826,5.75486987192408,56.6264997378176));
#23105=CARTESIAN_POINT('Ctrl Pts',(3.41470059302471,5.84487685720998,56.6347091378568));
#23106=CARTESIAN_POINT('Ctrl Pts',(3.26174323667611,5.92902353326394,56.642918537896));
#23107=CARTESIAN_POINT('Ctrl Pts',(3.20796365254908,5.95860938223443,56.6458049510152));
#23108=CARTESIAN_POINT('Ctrl Pts',(3.15376751463628,5.98747114796232,56.6486913641344));
#23109=CARTESIAN_POINT('Ctrl Pts',(3.09917575053263,6.01559628526637,56.6515777772535));
#23110=CARTESIAN_POINT('Origin',(0.,0.,-3.69717978381041));
#23111=CARTESIAN_POINT('',(3.09917575053261,6.01559628526638,59.0457515827422));
#23112=CARTESIAN_POINT('',(3.09917575053263,6.01559628526637,58.651392015122));
#23113=CARTESIAN_POINT('',(3.09917575053259,6.01559628526639,-3.69717978381041));
#23114=CARTESIAN_POINT('',(-6.76699881114908,0.0028363625950735,57.69717978381));
#23115=CARTESIAN_POINT('Ctrl Pts',(-6.767,2.48324459799684E-12,57.69717978381));
#23116=CARTESIAN_POINT('Ctrl Pts',(-6.76700000000007,-0.186007249413249,
57.7059292956159));
#23117=CARTESIAN_POINT('Ctrl Pts',(-6.75932637295451,-0.37201435552516,
57.7146788074219));
#23118=CARTESIAN_POINT('Ctrl Pts',(-6.74400518266947,-0.557389537152733,
57.7234283192279));
#23119=CARTESIAN_POINT('Ctrl Pts',(-6.72868405709669,-0.742763935809343,
57.7321777940784));
#23120=CARTESIAN_POINT('Ctrl Pts',(-6.70571545653017,-0.927506129693245,
57.740927268929));
#23121=CARTESIAN_POINT('Ctrl Pts',(-6.67517739415676,-1.11098863924823,
57.7496767437795));
#23122=CARTESIAN_POINT('Ctrl Pts',(-6.64463945823093,-1.29447038906542,
57.7584261824015));
#23123=CARTESIAN_POINT('Ctrl Pts',(-6.60653217027143,-1.47669218228286,
57.7671756210235));
#23124=CARTESIAN_POINT('Ctrl Pts',(-6.56098496116687,-1.65703510504219,
57.7759250596455));
#23125=CARTESIAN_POINT('Ctrl Pts',(-6.51543793687486,-1.83737729604131,
57.7846744627658));
#23126=CARTESIAN_POINT('Ctrl Pts',(-6.46245112202601,-2.01584035397176,
57.793423865886));
#23127=CARTESIAN_POINT('Ctrl Pts',(-6.40220448416196,-2.19181813638278,
57.8021732690062));
#23128=CARTESIAN_POINT('Ctrl Pts',(-6.34195808575139,-2.36779521936072,
57.8109226373515));
#23129=CARTESIAN_POINT('Ctrl Pts',(-6.27445201489185,-2.54128677544949,
57.8196720056968));
#23130=CARTESIAN_POINT('Ctrl Pts',(-6.19991555136133,-2.71170355237957,
57.828421374042));
#23131=CARTESIAN_POINT('Ctrl Pts',(-6.12537937788982,-2.88211966613192,
57.8371707083391));
#23132=CARTESIAN_POINT('Ctrl Pts',(-6.04381298133555,-3.04946076210568,
57.8459200426362));
#23133=CARTESIAN_POINT('Ctrl Pts',(-5.95549339426238,-3.21315848206981,
57.8546693769332));
#23134=CARTESIAN_POINT('Ctrl Pts',(-5.86717414355101,-3.37685557859738,
57.8634186779088));
#23135=CARTESIAN_POINT('Ctrl Pts',(-5.77210188986189,-3.5369090746739,57.8721679788843));
#23136=CARTESIAN_POINT('Ctrl Pts',(-5.67059953467031,-3.69277536784962,
57.8809172798599));
#23137=CARTESIAN_POINT('Ctrl Pts',(-5.56909755761735,-3.84864108035837,
57.8896665482406));
#23138=CARTESIAN_POINT('Ctrl Pts',(-5.46116568338046,-4.00031938104311,
57.8984158166214));
#23139=CARTESIAN_POINT('Ctrl Pts',(-5.34717048686099,-4.14729511663238,
57.9071650850021));
#23140=CARTESIAN_POINT('Ctrl Pts',(-5.23317570555503,-4.29427031688057,
57.9159143215147));
#23141=CARTESIAN_POINT('Ctrl Pts',(-5.11311782178793,-4.43654275987144,
57.9246635580274));
#23142=CARTESIAN_POINT('Ctrl Pts',(-4.98740459172003,-4.57362924147661,
57.93341279454));
#23143=CARTESIAN_POINT('Ctrl Pts',(-4.86169180910817,-4.7107152351445,57.9421619999111));
#23144=CARTESIAN_POINT('Ctrl Pts',(-4.73032391415416,-4.84261509316539,
57.9509112052822));
#23145=CARTESIAN_POINT('Ctrl Pts',(-4.59374707237275,-4.9688808433154,57.9596604106533));
#23146=CARTESIAN_POINT('Ctrl Pts',(-4.45717070537378,-5.09514615452746,
57.9684095856096));
#23147=CARTESIAN_POINT('Ctrl Pts',(-4.31538563819479,-5.21577720253658,
57.9771587605658));
#23148=CARTESIAN_POINT('Ctrl Pts',(-4.16887341290611,-5.33036429028679,
57.985907935522));
#23149=CARTESIAN_POINT('Ctrl Pts',(-4.02236168477283,-5.44495098921219,
57.99465708079));
#23150=CARTESIAN_POINT('Ctrl Pts',(-3.87112305634363,-5.55349359238812,
58.0034062260579));
#23151=CARTESIAN_POINT('Ctrl Pts',(-3.71567117316636,-5.65562346102536,
58.0121553713258));
#23152=CARTESIAN_POINT('Ctrl Pts',(-3.56021980457208,-5.75775299158826,
58.020904487632));
#23153=CARTESIAN_POINT('Ctrl Pts',(-3.400555448623,-5.85346967275404,58.0296536039381));
#23154=CARTESIAN_POINT('Ctrl Pts',(-3.2372203632332,-5.94244842803607,58.0384027202443));
#23155=CARTESIAN_POINT('Ctrl Pts',(-3.07388580495989,-6.03142689616504,
58.0471518083152));
#23156=CARTESIAN_POINT('Ctrl Pts',(-2.90688079257676,-6.11366734484836,
58.0559008963862));
#23157=CARTESIAN_POINT('Ctrl Pts',(-2.73677251094612,-6.18889046787303,
58.0646499844571));
#23158=CARTESIAN_POINT('Ctrl Pts',(-2.56666476416658,-6.26411335438264,
58.0733990450193));
#23159=CARTESIAN_POINT('Ctrl Pts',(-2.39345402972123,-6.33231884350279,
58.0821481055815));
#23160=CARTESIAN_POINT('Ctrl Pts',(-2.21772856474086,-6.39327529621027,
58.0908971661437));
#23161=CARTESIAN_POINT('Ctrl Pts',(-2.04200363768338,-6.45423156232059,
58.0996461999237));
#23162=CARTESIAN_POINT('Ctrl Pts',(-1.86376426620184,-6.50793874252029,
58.1083952337037));
#23163=CARTESIAN_POINT('Ctrl Pts',(-1.68361578194802,-6.55421443796094,
58.1171442674837));
#23164=CARTESIAN_POINT('Ctrl Pts',(-1.50346783420026,-6.60048999558642,
58.1258932752079));
#23165=CARTESIAN_POINT('Ctrl Pts',(-1.3214110625745,-6.63933404145454,58.1346422829321));
#23166=CARTESIAN_POINT('Ctrl Pts',(-1.13806375959293,-6.67061465526987,
58.1433912906564));
#23167=CARTESIAN_POINT('Ctrl Pts',(-0.954716987421843,-6.70189517852442,
58.1521402730512));
#23168=CARTESIAN_POINT('Ctrl Pts',(-0.77007997381277,-6.72561226535794,
58.1608892554461));
#23169=CARTESIAN_POINT('Ctrl Pts',(-0.584779770555553,-6.74168536939755,
58.169638237841));
#23170=CARTESIAN_POINT('Ctrl Pts',(-0.391490647557006,-6.75845143942376,
58.178764418517));
#23171=CARTESIAN_POINT('Ctrl Pts',(-0.197480213107425,-6.76689975924017,
58.1878905991931));
#23172=CARTESIAN_POINT('Ctrl Pts',(-0.00346532630087703,-6.76699911271707,
58.1970167798691));
#23173=CARTESIAN_POINT('Ctrl Pts',(0.184486595292999,-6.76709536139782,
58.2058577673991));
#23174=CARTESIAN_POINT('Ctrl Pts',(0.3724423781822,-6.75935659726787,58.214698754929));
#23175=CARTESIAN_POINT('Ctrl Pts',(0.559750217719087,-6.74380965729041,
58.2235397424589));
#23176=CARTESIAN_POINT('Ctrl Pts',(0.745129914454696,-6.72842275717287,
58.2322897210567));
#23177=CARTESIAN_POINT('Ctrl Pts',(0.929874656311072,-6.70538772273516,
58.2410396996545));
#23178=CARTESIAN_POINT('Ctrl Pts',(1.11335688289461,-6.67478280180795,58.2497896782522));
#23179=CARTESIAN_POINT('Ctrl Pts',(1.29683723118535,-6.64417819418086,58.2585395672772));
#23180=CARTESIAN_POINT('Ctrl Pts',(1.47905480729908,-6.60600390230148,58.2672894563021));
#23181=CARTESIAN_POINT('Ctrl Pts',(1.65939064804477,-6.56038959797218,58.276039345327));
#23182=CARTESIAN_POINT('Ctrl Pts',(1.83972470263941,-6.51477574543348,58.284789147688));
#23183=CARTESIAN_POINT('Ctrl Pts',(2.01817678125532,-6.46172209820199,58.2935389500489));
#23184=CARTESIAN_POINT('Ctrl Pts',(2.19414072347371,-6.4014088672412,58.3022887524099));
#23185=CARTESIAN_POINT('Ctrl Pts',(2.37010298131792,-6.34109621361488,58.3110384710154));
#23186=CARTESIAN_POINT('Ctrl Pts',(2.54357687926612,-6.27352420826093,58.3197881896209));
#23187=CARTESIAN_POINT('Ctrl Pts',(2.71397317789675,-6.19892237325626,58.3285379082263));
#23188=CARTESIAN_POINT('Ctrl Pts',(2.88436790206907,-6.12432122757102,58.3372875459846));
#23189=CARTESIAN_POINT('Ctrl Pts',(3.05168482125965,-6.04269049717564,58.3460371837429));
#23190=CARTESIAN_POINT('Ctrl Pts',(3.21535561997101,-5.95430745235085,58.3547868215011));
#23191=CARTESIAN_POINT('Ctrl Pts',(3.37902496075002,-5.86592519481678,58.3635363813202));
#23192=CARTESIAN_POINT('Ctrl Pts',(3.53904799384605,-5.77079087940398,58.3722859411392));
#23193=CARTESIAN_POINT('Ctrl Pts',(3.69488118814723,-5.66922763747195,58.3810355009582));
#23194=CARTESIAN_POINT('Ctrl Pts',(3.85071304610573,-5.56766526649232,58.3897849857456));
#23195=CARTESIAN_POINT('Ctrl Pts',(4.00235489705709,-5.45967423580903,58.3985344705331));
#23196=CARTESIAN_POINT('Ctrl Pts',(4.14929168607398,-5.34562133936527,58.4072839553205));
#23197=CARTESIAN_POINT('Ctrl Pts',(4.29622726385506,-5.23156938308737,58.4160333679838));
#23198=CARTESIAN_POINT('Ctrl Pts',(4.43845763091822,-5.11145583677415,58.4247827806471));
#23199=CARTESIAN_POINT('Ctrl Pts',(4.57549970660723,-4.98568866204431,58.4335321933104));
#23200=CARTESIAN_POINT('Ctrl Pts',(4.71254069815065,-4.85992248226385,58.4422815367567));
#23201=CARTESIAN_POINT('Ctrl Pts',(4.84439326931092,-4.72850295734229,58.451030880203));
#23202=CARTESIAN_POINT('Ctrl Pts',(4.97060959434485,-4.59187644221912,58.4597802236494));
#23203=CARTESIAN_POINT('Ctrl Pts',(5.09682496280305,-4.45525096256904,58.4685295007857));
#23204=CARTESIAN_POINT('Ctrl Pts',(5.21740397615631,-4.31341878218577,58.477278777922));
#23205=CARTESIAN_POINT('Ctrl Pts',(5.3319371045173,-4.16686161438938,58.4860280550582));
#23206=CARTESIAN_POINT('Ctrl Pts',(5.44646940289187,-4.0203055086478,58.4947772687912));
#23207=CARTESIAN_POINT('Ctrl Pts',(5.55495572749476,-3.86902470980404,58.5035264825242));
#23208=CARTESIAN_POINT('Ctrl Pts',(5.65702762491275,-3.71353301466057,58.5122756962571));
#23209=CARTESIAN_POINT('Ctrl Pts',(5.75909881654979,-3.55804239467176,58.5210248494933));
#23210=CARTESIAN_POINT('Ctrl Pts',(5.85475551250613,-3.39834117619844,58.5297740027294));
#23211=CARTESIAN_POINT('Ctrl Pts',(5.94367283727932,-3.23497174692268,58.5385231559655));
#23212=CARTESIAN_POINT('Ctrl Pts',(6.03258957676171,-3.07160339301243,58.547272251611));
#23213=CARTESIAN_POINT('Ctrl Pts',(6.11476689685164,-2.90456712829758,58.5560213472566));
#23214=CARTESIAN_POINT('Ctrl Pts',(6.18992570525159,-2.73443024476135,58.5647704429021));
#23215=CARTESIAN_POINT('Ctrl Pts',(6.26508404388607,-2.56429442463251,58.5735194838632));
#23216=CARTESIAN_POINT('Ctrl Pts',(6.33322384283236,-2.39105828656204,58.5822685248242));
#23217=CARTESIAN_POINT('Ctrl Pts',(6.39411368719963,-2.21531017132282,58.5910175657852));
#23218=CARTESIAN_POINT('Ctrl Pts',(6.45500317120822,-2.03956309619727,58.5997665549676));
#23219=CARTESIAN_POINT('Ctrl Pts',(6.50864269270009,-1.86130434438857,58.60851554415));
#23220=CARTESIAN_POINT('Ctrl Pts',(6.55485008446273,-1.6811393072018,58.6172645333324));
#23221=CARTESIAN_POINT('Ctrl Pts',(6.60199664749351,-1.49731239212072,58.6261913468618));
#23222=CARTESIAN_POINT('Ctrl Pts',(6.64140563640862,-1.31150116499899,58.6351181603912));
#23223=CARTESIAN_POINT('Ctrl Pts',(6.67293772282135,-1.12436255155884,58.6440449739205));
#23224=CARTESIAN_POINT('Ctrl Pts',(6.7038449494984,-0.940932395053588,58.6527948880761));
#23225=CARTESIAN_POINT('Ctrl Pts',(6.72718449348905,-0.756227260508963,
58.6615448022316));
#23226=CARTESIAN_POINT('Ctrl Pts',(6.74287707373913,-0.570874564543943,
58.6702947163871));
#23227=CARTESIAN_POINT('Ctrl Pts',(6.75856934538658,-0.385525513634686,
58.6790444584711));
#23228=CARTESIAN_POINT('Ctrl Pts',(6.76661493004097,-0.199529212420397,
58.6877942005551));
#23229=CARTESIAN_POINT('Ctrl Pts',(6.76698649908906,-0.013517438602549,
58.6965439426391));
#23230=CARTESIAN_POINT('Ctrl Pts',(6.76735806132395,0.172490924443669,58.705293524285));
#23231=CARTESIAN_POINT('Ctrl Pts',(6.760055888963,0.358514472899315,58.7140431059309));
#23232=CARTESIAN_POINT('Ctrl Pts',(6.74510478454601,0.543921359660137,58.7227926875768));
#23233=CARTESIAN_POINT('Ctrl Pts',(6.7301539344071,0.72932509314843,58.7315421204158));
#23234=CARTESIAN_POINT('Ctrl Pts',(6.70755443556924,0.914111900254398,58.7402915532548));
#23235=CARTESIAN_POINT('Ctrl Pts',(6.6773830468235,1.09765415591349,58.7490409860939));
#23236=CARTESIAN_POINT('Ctrl Pts',(6.64721213111895,1.28119353391093,58.7577902817552));
#23237=CARTESIAN_POINT('Ctrl Pts',(6.60946960955533,1.46348811672481,58.7665395774165));
#23238=CARTESIAN_POINT('Ctrl Pts',(6.56428366991224,1.64391876348059,58.7752888730779));
#23239=CARTESIAN_POINT('Ctrl Pts',(6.51909837867765,1.82434682109545,58.7840380431887));
#23240=CARTESIAN_POINT('Ctrl Pts',(6.46646995271976,2.00291071820267,58.7927872132995));
#23241=CARTESIAN_POINT('Ctrl Pts',(6.40657713281612,2.17900400212519,58.8015363834103));
#23242=CARTESIAN_POINT('Ctrl Pts',(6.34668509279128,2.35509499309474,58.8102854395961));
#23243=CARTESIAN_POINT('Ctrl Pts',(6.27952894037599,2.5287151639794,58.8190344957819));
#23244=CARTESIAN_POINT('Ctrl Pts',(6.20533675061526,2.69927486771238,58.8277835519677));
#23245=CARTESIAN_POINT('Ctrl Pts',(6.12832117907998,2.87632521635751,58.8368655532499));
#23246=CARTESIAN_POINT('Ctrl Pts',(6.04372366626162,3.05007728919834,58.8459475545322));
#23247=CARTESIAN_POINT('Ctrl Pts',(5.95185378007951,3.21989527478042,58.8550295558145));
#23248=CARTESIAN_POINT('Ctrl Pts',(5.86334450817458,3.38350129286602,58.8637793361216));
#23249=CARTESIAN_POINT('Ctrl Pts',(5.76808562057345,3.54345567124816,58.8725291164287));
#23250=CARTESIAN_POINT('Ctrl Pts',(5.66640068804577,3.69921508465167,58.8812788967359));
#23251=CARTESIAN_POINT('Ctrl Pts',(5.56471941108017,3.85496889852148,58.8900283624894));
#23252=CARTESIAN_POINT('Ctrl Pts',(5.45661270815207,4.00652780919509,58.8987778282428));
#23253=CARTESIAN_POINT('Ctrl Pts',(5.34244776449207,4.15337704569109,58.9075272939963));
#23254=CARTESIAN_POINT('Ctrl Pts',(5.22828631819689,4.30022178356136,58.9162764917159));
#23255=CARTESIAN_POINT('Ctrl Pts',(5.10806717844163,4.44235690972572,58.9250256894355));
#23256=CARTESIAN_POINT('Ctrl Pts',(4.98219864544812,4.57929969070544,58.9337748871551));
#23257=CARTESIAN_POINT('Ctrl Pts',(4.85633329944126,4.71623900429896,58.9425238633454));
#23258=CARTESIAN_POINT('Ctrl Pts',(4.72481904033758,4.84798602483509,58.9512728395356));
#23259=CARTESIAN_POINT('Ctrl Pts',(4.58810250737318,4.97409332259016,58.9600218157258));
#23260=CARTESIAN_POINT('Ctrl Pts',(4.45137708685764,5.10020881822029,58.968771360662));
#23261=CARTESIAN_POINT('Ctrl Pts',(4.30944892636175,5.22068366307831,58.9775209055982));
#23262=CARTESIAN_POINT('Ctrl Pts',(4.16280009466787,5.33510865604752,58.9862704505343));
#23263=CARTESIAN_POINT('Ctrl Pts',(4.01615988348914,5.44952692272799,58.9950194811426));
#23264=CARTESIAN_POINT('Ctrl Pts',(3.86479978232355,5.5578958728854,59.0037685117509));
#23265=CARTESIAN_POINT('Ctrl Pts',(3.70923383581191,5.65984746713797,59.0125175423592));
#23266=CARTESIAN_POINT('Ctrl Pts',(3.55366577799669,5.76180044505304,59.0212666917072));
#23267=CARTESIAN_POINT('Ctrl Pts',(3.39389200026974,5.85733573570982,59.0300158410552));
#23268=CARTESIAN_POINT('Ctrl Pts',(3.2304551362618,5.94612887621853,59.0387649904032));
#23269=CARTESIAN_POINT('Ctrl Pts',(3.18695122151672,5.96976399206638,59.0410938545162));
#23270=CARTESIAN_POINT('Ctrl Pts',(3.14318791262713,5.99292165435308,59.0434227186292));
#23271=CARTESIAN_POINT('Ctrl Pts',(3.09917575053261,6.01559628526638,59.0457515827422));
#23272=CARTESIAN_POINT('Ctrl Pts',(3.09917575053259,6.01559628526639,57.0458946091257));
#23273=CARTESIAN_POINT('Ctrl Pts',(2.93318603311847,6.10111254710523,57.0546656682455));
#23274=CARTESIAN_POINT('Ctrl Pts',(2.76353838605607,6.17981426143319,57.0634367273652));
#23275=CARTESIAN_POINT('Ctrl Pts',(2.59080947744217,6.25139946344783,57.072207786485));
#23276=CARTESIAN_POINT('Ctrl Pts',(2.41808056882822,6.32298466546249,57.0809788456047));
#23277=CARTESIAN_POINT('Ctrl Pts',(2.2422706905842,6.38745318365418,57.0897499047244));
#23278=CARTESIAN_POINT('Ctrl Pts',(2.06398265584147,6.44455309516382,57.0985209638442));
#23279=CARTESIAN_POINT('Ctrl Pts',(1.88926810960206,6.50050853347528,57.1071162216042));
#23280=CARTESIAN_POINT('Ctrl Pts',(1.71237973373101,6.54932200570452,57.1157114793643));
#23281=CARTESIAN_POINT('Ctrl Pts',(1.53391690303733,6.59085638855653,57.1243067371243));
#23282=CARTESIAN_POINT('Ctrl Pts',(1.3552869494704,6.63242966659682,57.1329100439788));
#23283=CARTESIAN_POINT('Ctrl Pts',(1.17507989550135,6.66671017993159,57.1415133508332));
#23284=CARTESIAN_POINT('Ctrl Pts',(0.993904102582022,6.69361215151211,57.1501166576877));
#23285=CARTESIAN_POINT('Ctrl Pts',(0.805216698462053,6.72162948816315,57.1590766606277));
#23286=CARTESIAN_POINT('Ctrl Pts',(0.615478894157729,6.74164336922374,57.1680366635677));
#23287=CARTESIAN_POINT('Ctrl Pts',(0.425380962470535,6.75361681151423,57.1769966665077));
#23288=CARTESIAN_POINT('Ctrl Pts',(0.242351441030697,6.76514504537225,57.1856235097124));
#23289=CARTESIAN_POINT('Ctrl Pts',(0.0589883873994425,6.76922003344946,
57.1942503529171));
#23290=CARTESIAN_POINT('Ctrl Pts',(-0.124094149256997,6.76586207678816,
57.2028771961219));
#23291=CARTESIAN_POINT('Ctrl Pts',(-0.307351666537452,6.76250091076914,
57.2115122844079));
#23292=CARTESIAN_POINT('Ctrl Pts',(-0.49032782722238,6.7516926346868,57.220147372694));
#23293=CARTESIAN_POINT('Ctrl Pts',(-0.672413472376344,6.73350942096072,
57.2287824609801));
#23294=CARTESIAN_POINT('Ctrl Pts',(-0.854769551255752,6.71529920151311,
57.2374303741052));
#23295=CARTESIAN_POINT('Ctrl Pts',(-1.0362321690501,6.68969219430666,57.2460782872303));
#23296=CARTESIAN_POINT('Ctrl Pts',(-1.21620064023721,6.65681192483959,57.2547262003555));
#23297=CARTESIAN_POINT('Ctrl Pts',(-1.23639036301568,6.65312325914697,57.2556963645595));
#23298=CARTESIAN_POINT('Ctrl Pts',(-1.25656129563698,6.6493431084083,57.2566665287636));
#23299=CARTESIAN_POINT('Ctrl Pts',(-1.27671260132203,6.64547168631585,57.2576366929677));
#23300=CARTESIAN_POINT('Ctrl Pts',(-1.44754763156528,6.61265125668285,57.2658613724865));
#23301=CARTESIAN_POINT('Ctrl Pts',(-1.61734140890645,6.5731958646621,57.2740860520053));
#23302=CARTESIAN_POINT('Ctrl Pts',(-1.78554078892278,6.52718416249251,57.2823107315241));
#23303=CARTESIAN_POINT('Ctrl Pts',(-1.95356337236176,6.48122082382735,57.2905267659742));
#23304=CARTESIAN_POINT('Ctrl Pts',(-2.11999455290109,6.42871499207132,57.2987428004244));
#23305=CARTESIAN_POINT('Ctrl Pts',(-2.28428994028193,6.36979657985456,57.3069588348745));
#23306=CARTESIAN_POINT('Ctrl Pts',(-2.44844554327894,6.31092829609289,57.3151678790291));
#23307=CARTESIAN_POINT('Ctrl Pts',(-2.61046863671812,6.24565841824118,57.3233769231837));
#23308=CARTESIAN_POINT('Ctrl Pts',(-2.7698285067248,6.17416707283944,57.3315859673383));
#23309=CARTESIAN_POINT('Ctrl Pts',(-2.92908470258851,6.10272223728966,57.3397896709664));
#23310=CARTESIAN_POINT('Ctrl Pts',(-3.08568080036079,6.0250641425843,57.3479933745944));
#23311=CARTESIAN_POINT('Ctrl Pts',(-3.23910455825723,5.94142160267029,57.3561970782225));
#23312=CARTESIAN_POINT('Ctrl Pts',(-3.39245921996666,5.85781673215416,57.3643970872165));
#23313=CARTESIAN_POINT('Ctrl Pts',(-3.54264407412645,5.76823295714502,57.3725970962105));
#23314=CARTESIAN_POINT('Ctrl Pts',(-3.68916997333061,5.67294578749664,57.3807971052045));
#23315=CARTESIAN_POINT('Ctrl Pts',(-3.83568415601414,5.57766623721176,57.3889964585084));
#23316=CARTESIAN_POINT('Ctrl Pts',(-3.9785396615097,5.47668438860189,57.3971958118123));
#23317=CARTESIAN_POINT('Ctrl Pts',(-4.11727460720717,5.37032017749846,57.4053951651163));
#23318=CARTESIAN_POINT('Ctrl Pts',(-4.25600864839371,5.26395665985831,57.4135944649628));
#23319=CARTESIAN_POINT('Ctrl Pts',(-4.39062189811246,5.15221106689264,57.4217937648094));
#23320=CARTESIAN_POINT('Ctrl Pts',(-4.52068408089549,5.03544481061386,57.429993064656));
#23321=CARTESIAN_POINT('Ctrl Pts',(-4.65076901026754,4.91865813307208,57.438193798479));
#23322=CARTESIAN_POINT('Ctrl Pts',(-4.77630102015048,4.79684928233111,57.446394532302));
#23323=CARTESIAN_POINT('Ctrl Pts',(-4.89688531866907,4.67041788021194,57.454595266125));
#23324=CARTESIAN_POINT('Ctrl Pts',(-5.01751258160126,4.54394143034509,57.462798921885));
#23325=CARTESIAN_POINT('Ctrl Pts',(-5.13318837414066,4.41283940741912,57.471002577645));
#23326=CARTESIAN_POINT('Ctrl Pts',(-5.24355691907412,4.27754600634873,57.4792062334049));
#23327=CARTESIAN_POINT('Ctrl Pts',(-5.35405189827077,4.14209761799016,57.48741928698));
#23328=CARTESIAN_POINT('Ctrl Pts',(-5.45922725652506,4.00244853694774,57.4956323405549));
#23329=CARTESIAN_POINT('Ctrl Pts',(-5.55876882285838,3.85906441693031,57.50384539413));
#23330=CARTESIAN_POINT('Ctrl Pts',(-5.65836929016983,3.71559545331207,57.512063307553));
#23331=CARTESIAN_POINT('Ctrl Pts',(-5.75232912779609,3.56838734685494,57.5202812209761));
#23332=CARTESIAN_POINT('Ctrl Pts',(-5.84037927736495,3.41793196195098,57.5284991343992));
#23333=CARTESIAN_POINT('Ctrl Pts',(-5.92856675546629,3.2672419173978,57.5367298649952));
#23334=CARTESIAN_POINT('Ctrl Pts',(-6.0108259569123,3.11329478905805,57.5449605955912));
#23335=CARTESIAN_POINT('Ctrl Pts',(-6.08693469270373,2.95660532482097,57.5531913261871));
#23336=CARTESIAN_POINT('Ctrl Pts',(-6.15683146409667,2.81270479162234,57.5607502678629));
#23337=CARTESIAN_POINT('Ctrl Pts',(-6.22154127474536,2.66649174099346,57.5683092095387));
#23338=CARTESIAN_POINT('Ctrl Pts',(-6.28092899305939,2.51837645798755,57.5758681512144));
#23339=CARTESIAN_POINT('Ctrl Pts',(-6.35325564641545,2.33799096693271,57.5850739764228));
#23340=CARTESIAN_POINT('Ctrl Pts',(-6.4178787503003,2.15431021712131,57.5942798016312));
#23341=CARTESIAN_POINT('Ctrl Pts',(-6.47451834347859,1.96796880563672,57.6034856268395));
#23342=CARTESIAN_POINT('Ctrl Pts',(-6.53087849318174,1.7825467491239,57.6126460331519));
#23343=CARTESIAN_POINT('Ctrl Pts',(-6.57933360955935,1.59449040026369,57.6218064394644));
#23344=CARTESIAN_POINT('Ctrl Pts',(-6.61965344318901,1.40444910626052,57.6309668457768));
#23345=CARTESIAN_POINT('Ctrl Pts',(-6.65984329256155,1.21502047293069,57.6400977205039));
#23346=CARTESIAN_POINT('Ctrl Pts',(-6.69195011400064,1.02361985191255,57.6492285952309));
#23347=CARTESIAN_POINT('Ctrl Pts',(-6.71579294063093,0.830911655094422,
57.658359469958));
#23348=CARTESIAN_POINT('Ctrl Pts',(-6.73951276827878,0.63919759007472,57.6674432408614));
#23349=CARTESIAN_POINT('Ctrl Pts',(-6.75505355118757,0.446189597845692,
57.6765270117648));
#23350=CARTESIAN_POINT('Ctrl Pts',(-6.76228528965658,0.252560213205239,
57.6856107826683));
#23351=CARTESIAN_POINT('Ctrl Pts',(-6.76535537994889,0.170358720903004,
57.6894671163822));
#23352=CARTESIAN_POINT('Ctrl Pts',(-6.76692856984046,0.0880454475793552,
57.6933234500961));
#23353=CARTESIAN_POINT('Ctrl Pts',(-6.76699762229816,0.00567272518766376,
57.69717978381));
#23354=CARTESIAN_POINT('',(-6.76699917942892,0.00177812752557784,57.3028202161898));
#23355=CARTESIAN_POINT('Ctrl Pts',(3.09917575053263,6.01559628526637,56.6515777772535));
#23356=CARTESIAN_POINT('Ctrl Pts',(2.94405292266811,6.09551403301305,56.6597795375883));
#23357=CARTESIAN_POINT('Ctrl Pts',(2.78573390061559,6.16948079869564,56.6679812979231));
#23358=CARTESIAN_POINT('Ctrl Pts',(2.62471678447104,6.2372390367306,56.6761830582579));
#23359=CARTESIAN_POINT('Ctrl Pts',(2.46377224922607,6.3049667317153,56.6843811215253));
#23360=CARTESIAN_POINT('Ctrl Pts',(2.3001323728999,6.36649133592748,56.6925791847926));
#23361=CARTESIAN_POINT('Ctrl Pts',(2.13431734198294,6.42160248565036,56.7007772480599));
#23362=CARTESIAN_POINT('Ctrl Pts',(1.96851864043036,6.47670820806041,56.7089745039869));
#23363=CARTESIAN_POINT('Ctrl Pts',(1.80054554873222,6.52540161398418,56.7171717599139));
#23364=CARTESIAN_POINT('Ctrl Pts',(1.63093593018586,6.56752137351899,56.7253690158409));
#23365=CARTESIAN_POINT('Ctrl Pts',(1.46132768219545,6.60964079269878,56.7335662055288));
#23366=CARTESIAN_POINT('Ctrl Pts',(1.29008328168006,6.64518658412611,56.7417633952166));
#23367=CARTESIAN_POINT('Ctrl Pts',(1.11775327674701,6.6740479929591,56.7499605849045));
#23368=CARTESIAN_POINT('Ctrl Pts',(0.945393343640902,6.70291441408949,56.7581591981802));
#23369=CARTESIAN_POINT('Ctrl Pts',(0.771947784351753,6.72509408092856,56.766357811456));
#23370=CARTESIAN_POINT('Ctrl Pts',(0.597974857397319,6.74052780351218,56.7745564247317));
#23371=CARTESIAN_POINT('Ctrl Pts',(0.423940097438025,6.7559670115093,56.7827579519373));
#23372=CARTESIAN_POINT('Ctrl Pts',(0.24937795353745,6.76465546779899,56.7909594791428));
#23373=CARTESIAN_POINT('Ctrl Pts',(0.0748493465936413,6.76658603546238,
56.7991610063483));
#23374=CARTESIAN_POINT('Ctrl Pts',(-0.09986542506865,6.76851866240759,56.8073712818905));
#23375=CARTESIAN_POINT('Ctrl Pts',(-0.274546229425493,6.76367899881959,
56.8155815574327));
#23376=CARTESIAN_POINT('Ctrl Pts',(-0.448633668200303,6.75211202748867,
56.8237918329748));
#23377=CARTESIAN_POINT('Ctrl Pts',(-0.622824548304756,6.74053818315816,
56.8320069869955));
#23378=CARTESIAN_POINT('Ctrl Pts',(-0.796421004089131,6.72222910078704,
56.8402221410161));
#23379=CARTESIAN_POINT('Ctrl Pts',(-0.968871311662083,6.69728134256268,
56.8484372950367));
#23380=CARTESIAN_POINT('Ctrl Pts',(-1.14155771237634,6.67229942960303,56.8566636960162));
#23381=CARTESIAN_POINT('Ctrl Pts',(-1.31309447847888,6.64066075042655,56.8648900969957));
#23382=CARTESIAN_POINT('Ctrl Pts',(-1.4829415689939,6.60251265072244,56.8731164979752));
#23383=CARTESIAN_POINT('Ctrl Pts',(-1.57685225994353,6.58142006449818,56.8776649833079));
#23384=CARTESIAN_POINT('Ctrl Pts',(-1.6702466723437,6.55833834733766,56.8822134686406));
#23385=CARTESIAN_POINT('Ctrl Pts',(-1.76303592873773,6.53329880795145,56.8867619539734));
#23386=CARTESIAN_POINT('Ctrl Pts',(-1.92934835439208,6.48841875723844,56.8949145101866));
#23387=CARTESIAN_POINT('Ctrl Pts',(-2.09420608726525,6.43711385937417,56.9030670663999));
#23388=CARTESIAN_POINT('Ctrl Pts',(-2.25707025773122,6.37949236629884,56.9112196226131));
#23389=CARTESIAN_POINT('Ctrl Pts',(-2.41974574612937,6.32193762911238,56.9193627338935));
#23390=CARTESIAN_POINT('Ctrl Pts',(-2.58043192847426,6.25808098443318,56.9275058451738));
#23391=CARTESIAN_POINT('Ctrl Pts',(-2.73860145605382,6.18808137187124,56.9356489564542));
#23392=CARTESIAN_POINT('Ctrl Pts',(-2.89662099359569,6.11814813900132,56.9437843457315));
#23393=CARTESIAN_POINT('Ctrl Pts',(-3.05212829561936,6.04208368258898,56.9519197350089));
#23394=CARTESIAN_POINT('Ctrl Pts',(-3.20461248564616,5.96009629258125,56.9600551242862));
#23395=CARTESIAN_POINT('Ctrl Pts',(-3.35698411757205,5.8781694225849,56.9681845083248));
#23396=CARTESIAN_POINT('Ctrl Pts',(-3.50633676029002,5.7903284969734,56.9763138923634));
#23397=CARTESIAN_POINT('Ctrl Pts',(-3.65218080266926,5.69682932732008,56.9844432764019));
#23398=CARTESIAN_POINT('Ctrl Pts',(-3.79794782267948,5.60337953594392,56.9925683671941));
#23399=CARTESIAN_POINT('Ctrl Pts',(-3.94020962550192,5.50427764850932,57.0006934579862));
#23400=CARTESIAN_POINT('Ctrl Pts',(-4.07850245121144,5.39982469673436,57.0088185487783));
#23401=CARTESIAN_POINT('Ctrl Pts',(-4.21732317061703,5.29497302539824,57.0169746548035));
#23402=CARTESIAN_POINT('Ctrl Pts',(-4.35214422810211,5.18472953990045,57.0251307608286));
#23403=CARTESIAN_POINT('Ctrl Pts',(-4.48252671162608,5.06944210732884,57.0332868668537));
#23404=CARTESIAN_POINT('Ctrl Pts',(-4.61238442923383,4.95461868582334,57.0414101460271));
#23405=CARTESIAN_POINT('Ctrl Pts',(-4.73783897379996,4.83479210393786,57.0495334252005));
#23406=CARTESIAN_POINT('Ctrl Pts',(-4.85849089436494,4.71034555307495,57.0576567043739));
#23407=CARTESIAN_POINT('Ctrl Pts',(-4.97915888075271,4.58588243110217,57.0657810652306));
#23408=CARTESIAN_POINT('Ctrl Pts',(-5.09502271468609,4.45679837748956,57.0739054260873));
#23409=CARTESIAN_POINT('Ctrl Pts',(-5.20572086942813,4.32351237185699,57.082029786944));
#23410=CARTESIAN_POINT('Ctrl Pts',(-5.31645482545819,4.19018325971837,57.0901567753294));
#23411=CARTESIAN_POINT('Ctrl Pts',(-5.42201954189366,4.05264977069983,57.0982837637148));
#23412=CARTESIAN_POINT('Ctrl Pts',(-5.52209476250759,3.91136273361168,57.1064107521003));
#23413=CARTESIAN_POINT('Ctrl Pts',(-5.62281695802919,3.76916229191435,57.1145902805403));
#23414=CARTESIAN_POINT('Ctrl Pts',(-5.71797821649251,3.62315990804978,57.1227698089804));
#23415=CARTESIAN_POINT('Ctrl Pts',(-5.8072976639558,3.47384266227093,57.1309493374205));
#23416=CARTESIAN_POINT('Ctrl Pts',(-5.89619647734567,3.32522859954018,57.1390903458242));
#23417=CARTESIAN_POINT('Ctrl Pts',(-5.97930826431235,3.17333118059628,57.1472313542278));
#23418=CARTESIAN_POINT('Ctrl Pts',(-6.05640359250733,3.01865276649441,57.1553723626315));
#23419=CARTESIAN_POINT('Ctrl Pts',(-6.13404609766739,2.8628765366471,57.1635711510898));
#23420=CARTESIAN_POINT('Ctrl Pts',(-6.20558627238428,2.70428003495723,57.1717699395481));
#23421=CARTESIAN_POINT('Ctrl Pts',(-6.27084024999759,2.54339370900577,57.1799687280064));
#23422=CARTESIAN_POINT('Ctrl Pts',(-6.33609422761088,2.38250738305437,57.1881675164646));
#23423=CARTESIAN_POINT('Ctrl Pts',(-6.39506194283338,2.21933160411982,57.1963663049229));
#23424=CARTESIAN_POINT('Ctrl Pts',(-6.44761148990513,2.05440869235978,57.2045650933811));
#23425=CARTESIAN_POINT('Ctrl Pts',(-6.5133098196148,1.84821928755487,57.2148153569394));
#23426=CARTESIAN_POINT('Ctrl Pts',(-6.56914272493654,1.63878519480052,57.2250656204976));
#23427=CARTESIAN_POINT('Ctrl Pts',(-6.61484041058002,1.42694615965621,57.2353158840558));
#23428=CARTESIAN_POINT('Ctrl Pts',(-6.66019682625352,1.21668913682053,57.2454895987235));
#23429=CARTESIAN_POINT('Ctrl Pts',(-6.69556881076077,1.00406286086859,57.2556633133912));
#23430=CARTESIAN_POINT('Ctrl Pts',(-6.72073887317306,0.789910120596348,
57.2658370280589));
#23431=CARTESIAN_POINT('Ctrl Pts',(-6.74554717001033,0.578835365907071,
57.2758645174342));
#23432=CARTESIAN_POINT('Ctrl Pts',(-6.76044466374881,0.36627764876757,57.2858920068094));
#23433=CARTESIAN_POINT('Ctrl Pts',(-6.76526863623834,0.153066258626491,
57.2959194961847));
#23434=CARTESIAN_POINT('Ctrl Pts',(-6.76637522374717,0.104156970361828,
57.2982197361864));
#23435=CARTESIAN_POINT('Ctrl Pts',(-6.76695192245588,0.0552133810525768,
57.3005199761882));
#23436=CARTESIAN_POINT('Ctrl Pts',(-6.76699711774311,0.00624567502194366,
57.3028202161899));
#23437=CARTESIAN_POINT('Ctrl Pts',(-6.767,2.30894580037963E-12,57.3028202161898));
#23438=CARTESIAN_POINT('Ctrl Pts',(-6.76700000000006,-0.186007249413423,
57.3115697279958));
#23439=CARTESIAN_POINT('Ctrl Pts',(-6.7593263729545,-0.372014355525331,
57.3203192398017));
#23440=CARTESIAN_POINT('Ctrl Pts',(-6.74400518266946,-0.557389537152904,
57.3290687516077));
#23441=CARTESIAN_POINT('Ctrl Pts',(-6.72868405709669,-0.742763935809257,
57.3378182264582));
#23442=CARTESIAN_POINT('Ctrl Pts',(-6.70571545653021,-0.927506129692905,
57.3465677013088));
#23443=CARTESIAN_POINT('Ctrl Pts',(-6.67517739415685,-1.11098863924764,
57.3553171761593));
#23444=CARTESIAN_POINT('Ctrl Pts',(-6.64463945823106,-1.29447038906471,
57.3640666147813));
#23445=CARTESIAN_POINT('Ctrl Pts',(-6.60653217027161,-1.47669218228203,
57.3728160534033));
#23446=CARTESIAN_POINT('Ctrl Pts',(-6.56098496116711,-1.65703510504124,
57.3815654920253));
#23447=CARTESIAN_POINT('Ctrl Pts',(-6.51543793687511,-1.83737729604043,
57.3903148951455));
#23448=CARTESIAN_POINT('Ctrl Pts',(-6.46245112202627,-2.01584035397095,
57.3990642982657));
#23449=CARTESIAN_POINT('Ctrl Pts',(-6.40220448416222,-2.19181813638204,
57.407813701386));
#23450=CARTESIAN_POINT('Ctrl Pts',(-6.34195808575158,-2.36779521936023,
57.4165630697313));
#23451=CARTESIAN_POINT('Ctrl Pts',(-6.27445201489196,-2.54128677544924,
57.4253124380765));
#23452=CARTESIAN_POINT('Ctrl Pts',(-6.19991555136134,-2.71170355237955,
57.4340618064218));
#23453=CARTESIAN_POINT('Ctrl Pts',(-6.12537937788983,-2.8821196661319,57.4428111407189));
#23454=CARTESIAN_POINT('Ctrl Pts',(-6.04381298133556,-3.04946076210566,
57.4515604750159));
#23455=CARTESIAN_POINT('Ctrl Pts',(-5.95549339426239,-3.21315848206979,
57.460309809313));
#23456=CARTESIAN_POINT('Ctrl Pts',(-5.86717414355093,-3.37685557859754,
57.4690591102886));
#23457=CARTESIAN_POINT('Ctrl Pts',(-5.7721018898617,-3.53690907467422,57.4778084112641));
#23458=CARTESIAN_POINT('Ctrl Pts',(-5.67059953467,-3.69277536785009,57.4865577122397));
#23459=CARTESIAN_POINT('Ctrl Pts',(-5.56909755761692,-3.84864108035899,
57.4953069806205));
#23460=CARTESIAN_POINT('Ctrl Pts',(-5.46116568337991,-4.00031938104388,
57.5040562490012));
#23461=CARTESIAN_POINT('Ctrl Pts',(-5.34717048686029,-4.14729511663328,
57.512805517382));
#23462=CARTESIAN_POINT('Ctrl Pts',(-5.23317570555419,-4.2942703168816,57.5215547538946));
#23463=CARTESIAN_POINT('Ctrl Pts',(-5.11311782178693,-4.43654275987259,
57.5303039904072));
#23464=CARTESIAN_POINT('Ctrl Pts',(-4.98740459171888,-4.57362924147787,
57.5390532269199));
#23465=CARTESIAN_POINT('Ctrl Pts',(-4.86169180910706,-4.71071523514563,
57.547802432291));
#23466=CARTESIAN_POINT('Ctrl Pts',(-4.73032391415311,-4.84261509316641,
57.5565516376621));
#23467=CARTESIAN_POINT('Ctrl Pts',(-4.59374707237177,-4.96888084331631,
57.5653008430332));
#23468=CARTESIAN_POINT('Ctrl Pts',(-4.45717070537292,-5.0951461545282,57.5740500179894));
#23469=CARTESIAN_POINT('Ctrl Pts',(-4.31538563819405,-5.21577720253718,
57.5827991929457));
#23470=CARTESIAN_POINT('Ctrl Pts',(-4.16887341290552,-5.33036429028725,
57.5915483679019));
#23471=CARTESIAN_POINT('Ctrl Pts',(-4.02236168477258,-5.44495098921236,
57.6002975131698));
#23472=CARTESIAN_POINT('Ctrl Pts',(-3.87112305634375,-5.55349359238803,
57.6090466584377));
#23473=CARTESIAN_POINT('Ctrl Pts',(-3.71567117316686,-5.65562346102504,
57.6177958037056));
#23474=CARTESIAN_POINT('Ctrl Pts',(-3.56021980457275,-5.75775299158784,
57.6265449200117));
#23475=CARTESIAN_POINT('Ctrl Pts',(-3.40055544862384,-5.85346967275354,
57.6352940363179));
#23476=CARTESIAN_POINT('Ctrl Pts',(-3.23722036323423,-5.94244842803551,
57.6440431526241));
#23477=CARTESIAN_POINT('Ctrl Pts',(-3.07388580496088,-6.03142689616454,
57.652792240695));
#23478=CARTESIAN_POINT('Ctrl Pts',(-2.90688079257771,-6.11366734484792,
57.6615413287659));
#23479=CARTESIAN_POINT('Ctrl Pts',(-2.73677251094701,-6.18889046787264,
57.6702904168368));
#23480=CARTESIAN_POINT('Ctrl Pts',(-2.56666476416755,-6.26411335438225,
57.6790394773991));
#23481=CARTESIAN_POINT('Ctrl Pts',(-2.39345402972227,-6.33231884350239,
57.6877885379613));
#23482=CARTESIAN_POINT('Ctrl Pts',(-2.21772856474196,-6.39327529620988,
57.6965375985235));
#23483=CARTESIAN_POINT('Ctrl Pts',(-2.04200363768462,-6.4542315623202,57.7052866323035));
#23484=CARTESIAN_POINT('Ctrl Pts',(-1.86376426620321,-6.5079387425199,57.7140356660835));
#23485=CARTESIAN_POINT('Ctrl Pts',(-1.68361578194952,-6.55421443796055,
57.7227846998635));
#23486=CARTESIAN_POINT('Ctrl Pts',(-1.50346783420109,-6.60048999558625,
57.7315337075877));
#23487=CARTESIAN_POINT('Ctrl Pts',(-1.32141106257464,-6.63933404145453,
57.7402827153119));
#23488=CARTESIAN_POINT('Ctrl Pts',(-1.13806375959237,-6.67061465526997,
57.7490317230362));
#23489=CARTESIAN_POINT('Ctrl Pts',(-0.954716987420905,-6.70189517852456,
57.7577807054311));
#23490=CARTESIAN_POINT('Ctrl Pts',(-0.770079973811447,-6.7256122653581,
57.766529687826));
#23491=CARTESIAN_POINT('Ctrl Pts',(-0.584779770553844,-6.7416853693977,
57.7752786702208));
#23492=CARTESIAN_POINT('Ctrl Pts',(-0.391490647555292,-6.75845143942386,
57.7844048508969));
#23493=CARTESIAN_POINT('Ctrl Pts',(-0.197480213105708,-6.76689975924022,
57.793531031573));
#23494=CARTESIAN_POINT('Ctrl Pts',(-0.00346532629915959,-6.76699911271707,
57.802657212249));
#23495=CARTESIAN_POINT('Ctrl Pts',(0.184486595294652,-6.76709536139777,
57.8114981997789));
#23496=CARTESIAN_POINT('Ctrl Pts',(0.372442378183787,-6.75935659726778,
57.8203391873089));
#23497=CARTESIAN_POINT('Ctrl Pts',(0.559750217720607,-6.74380965729029,
57.8291801748388));
#23498=CARTESIAN_POINT('Ctrl Pts',(0.745129914456277,-6.7284227571727,57.8379301534366));
#23499=CARTESIAN_POINT('Ctrl Pts',(0.929874656312708,-6.70538772273493,
57.8466801320343));
#23500=CARTESIAN_POINT('Ctrl Pts',(1.1133568828963,-6.67478280180767,57.8554301106321));
#23501=CARTESIAN_POINT('Ctrl Pts',(1.29683723118703,-6.64417819418053,57.864179999657));
#23502=CARTESIAN_POINT('Ctrl Pts',(1.47905480730076,-6.60600390230111,57.872929888682));
#23503=CARTESIAN_POINT('Ctrl Pts',(1.65939064804643,-6.56038959797176,57.8816797777069));
#23504=CARTESIAN_POINT('Ctrl Pts',(1.839724702641,-6.51477574543303,57.8904295800679));
#23505=CARTESIAN_POINT('Ctrl Pts',(2.01817678125683,-6.46172209820151,57.8991793824288));
#23506=CARTESIAN_POINT('Ctrl Pts',(2.19414072347515,-6.40140886724071,57.9079291847898));
#23507=CARTESIAN_POINT('Ctrl Pts',(2.37010298131935,-6.34109621361435,57.9166789033953));
#23508=CARTESIAN_POINT('Ctrl Pts',(2.54357687926754,-6.27352420826035,57.9254286220007));
#23509=CARTESIAN_POINT('Ctrl Pts',(2.71397317789815,-6.19892237325565,57.9341783406062));
#23510=CARTESIAN_POINT('Ctrl Pts',(2.88436790207039,-6.12432122757039,57.9429279783645));
#23511=CARTESIAN_POINT('Ctrl Pts',(3.0516848212609,-6.04269049717501,57.9516776161227));
#23512=CARTESIAN_POINT('Ctrl Pts',(3.21535561997218,-5.95430745235022,57.960427253881));
#23513=CARTESIAN_POINT('Ctrl Pts',(3.37902496075111,-5.86592519481614,57.9691768137));
#23514=CARTESIAN_POINT('Ctrl Pts',(3.53904799384707,-5.77079087940335,57.977926373519));
#23515=CARTESIAN_POINT('Ctrl Pts',(3.69488118814818,-5.66922763747132,57.986675933338));
#23516=CARTESIAN_POINT('Ctrl Pts',(3.85071304610672,-5.56766526649163,57.9954254181255));
#23517=CARTESIAN_POINT('Ctrl Pts',(4.00235489705812,-5.45967423580828,58.0041749029129));
#23518=CARTESIAN_POINT('Ctrl Pts',(4.14929168607503,-5.34562133936446,58.0129243877004));
#23519=CARTESIAN_POINT('Ctrl Pts',(4.29622726385604,-5.23156938308656,58.0216738003637));
#23520=CARTESIAN_POINT('Ctrl Pts',(4.43845763091913,-5.11145583677336,58.030423213027));
#23521=CARTESIAN_POINT('Ctrl Pts',(4.57549970660807,-4.98568866204353,58.0391726256903));
#23522=CARTESIAN_POINT('Ctrl Pts',(4.71254069815142,-4.8599224822631,58.0479219691366));
#23523=CARTESIAN_POINT('Ctrl Pts',(4.84439326931163,-4.72850295734157,58.0566713125829));
#23524=CARTESIAN_POINT('Ctrl Pts',(4.9706095943455,-4.59187644221842,58.0654206560292));
#23525=CARTESIAN_POINT('Ctrl Pts',(5.09682496280371,-4.45525096256828,58.0741699331655));
#23526=CARTESIAN_POINT('Ctrl Pts',(5.217403976157,-4.31341878218494,58.0829192103018));
#23527=CARTESIAN_POINT('Ctrl Pts',(5.331937104518,-4.16686161438848,58.0916684874381));
#23528=CARTESIAN_POINT('Ctrl Pts',(5.44646940289262,-4.02030550864678,58.1004177011711));
#23529=CARTESIAN_POINT('Ctrl Pts',(5.55495572749556,-3.8690247098029,58.1091669149041));
#23530=CARTESIAN_POINT('Ctrl Pts',(5.65702762491359,-3.71353301465929,58.117916128637));
#23531=CARTESIAN_POINT('Ctrl Pts',(5.75909881655059,-3.55804239467046,58.1266652818731));
#23532=CARTESIAN_POINT('Ctrl Pts',(5.8547555125069,-3.39834117619712,58.1354144351092));
#23533=CARTESIAN_POINT('Ctrl Pts',(5.94367283728005,-3.23497174692134,58.1441635883454));
#23534=CARTESIAN_POINT('Ctrl Pts',(6.03258957676231,-3.07160339301124,58.1529126839909));
#23535=CARTESIAN_POINT('Ctrl Pts',(6.11476689685213,-2.90456712829655,58.1616617796364));
#23536=CARTESIAN_POINT('Ctrl Pts',(6.18992570525198,-2.73443024476048,58.170410875282));
#23537=CARTESIAN_POINT('Ctrl Pts',(6.26508404388646,-2.56429442463157,58.179159916243));
#23538=CARTESIAN_POINT('Ctrl Pts',(6.33322384283274,-2.39105828656103,58.1879089572041));
#23539=CARTESIAN_POINT('Ctrl Pts',(6.39411368720001,-2.21531017132174,58.1966579981651));
#23540=CARTESIAN_POINT('Ctrl Pts',(6.45500317120857,-2.03956309619618,58.2054069873475));
#23541=CARTESIAN_POINT('Ctrl Pts',(6.5086426927004,-1.86130434438747,58.2141559765299));
#23542=CARTESIAN_POINT('Ctrl Pts',(6.55485008446302,-1.68113930720069,58.2229049657123));
#23543=CARTESIAN_POINT('Ctrl Pts',(6.60199664749377,-1.4973123921196,58.2318317792417));
#23544=CARTESIAN_POINT('Ctrl Pts',(6.64140563640884,-1.31150116499787,58.240758592771));
#23545=CARTESIAN_POINT('Ctrl Pts',(6.67293772282154,-1.12436255155771,58.2496854063004));
#23546=CARTESIAN_POINT('Ctrl Pts',(6.70384494949855,-0.940932395052457,
58.2584353204559));
#23547=CARTESIAN_POINT('Ctrl Pts',(6.72718449348918,-0.75622726050783,58.2671852346114));
#23548=CARTESIAN_POINT('Ctrl Pts',(6.74287707373923,-0.570874564542807,
58.275935148767));
#23549=CARTESIAN_POINT('Ctrl Pts',(6.75856934538664,-0.38552551363361,58.284684890851));
#23550=CARTESIAN_POINT('Ctrl Pts',(6.766614930041,-0.199529212419383,58.2934346329349));
#23551=CARTESIAN_POINT('Ctrl Pts',(6.76698649908906,-0.0135174386015994,
58.3021843750189));
#23552=CARTESIAN_POINT('Ctrl Pts',(6.76735806132392,0.172490924444619,58.3109339566648));
#23553=CARTESIAN_POINT('Ctrl Pts',(6.76005588896295,0.358514472900262,58.3196835383107));
#23554=CARTESIAN_POINT('Ctrl Pts',(6.74510478454594,0.543921359661082,58.3284331199566));
#23555=CARTESIAN_POINT('Ctrl Pts',(6.730153934407,0.729325093149309,58.3371825527956));
#23556=CARTESIAN_POINT('Ctrl Pts',(6.70755443556913,0.914111900255213,58.3459319856347));
#23557=CARTESIAN_POINT('Ctrl Pts',(6.67738304682337,1.09765415591424,58.3546814184737));
#23558=CARTESIAN_POINT('Ctrl Pts',(6.6472121311188,1.28119353391173,58.3634307141351));
#23559=CARTESIAN_POINT('Ctrl Pts',(6.60946960955513,1.46348811672568,58.3721800097964));
#23560=CARTESIAN_POINT('Ctrl Pts',(6.56428366991201,1.64391876348151,58.3809293054577));
#23561=CARTESIAN_POINT('Ctrl Pts',(6.51909837867738,1.82434682109643,58.3896784755686));
#23562=CARTESIAN_POINT('Ctrl Pts',(6.46646995271944,2.0029107182037,58.3984276456794));
#23563=CARTESIAN_POINT('Ctrl Pts',(6.40657713281575,2.17900400212627,58.4071768157902));
#23564=CARTESIAN_POINT('Ctrl Pts',(6.3466850927909,2.35509499309575,58.415925871976));
#23565=CARTESIAN_POINT('Ctrl Pts',(6.27952894037561,2.52871516398034,58.4246749281618));
#23566=CARTESIAN_POINT('Ctrl Pts',(6.20533675061488,2.69927486771325,58.4334239843475));
#23567=CARTESIAN_POINT('Ctrl Pts',(6.1283211790796,2.87632521635831,58.4425059856298));
#23568=CARTESIAN_POINT('Ctrl Pts',(6.04372366626125,3.05007728919907,58.4515879869121));
#23569=CARTESIAN_POINT('Ctrl Pts',(5.95185378007915,3.21989527478108,58.4606699881943));
#23570=CARTESIAN_POINT('Ctrl Pts',(5.8633445081742,3.38350129286667,58.4694197685015));
#23571=CARTESIAN_POINT('Ctrl Pts',(5.76808562057306,3.5434556712488,58.4781695488086));
#23572=CARTESIAN_POINT('Ctrl Pts',(5.66640068804536,3.6992150846523,58.4869193291157));
#23573=CARTESIAN_POINT('Ctrl Pts',(5.56471941107977,3.85496889852205,58.4956687948692));
#23574=CARTESIAN_POINT('Ctrl Pts',(5.4566127081517,4.0065278091956,58.5044182606227));
#23575=CARTESIAN_POINT('Ctrl Pts',(5.34244776449173,4.15337704569154,58.5131677263762));
#23576=CARTESIAN_POINT('Ctrl Pts',(5.22828631819657,4.30022178356175,58.5219169240958));
#23577=CARTESIAN_POINT('Ctrl Pts',(5.10806717844134,4.44235690972605,58.5306661218153));
#23578=CARTESIAN_POINT('Ctrl Pts',(4.98219864544787,4.57929969070571,58.5394153195349));
#23579=CARTESIAN_POINT('Ctrl Pts',(4.85633329944113,4.71623900429909,58.5481642957252));
#23580=CARTESIAN_POINT('Ctrl Pts',(4.72481904033758,4.84798602483508,58.5569132719154));
#23581=CARTESIAN_POINT('Ctrl Pts',(4.58810250737332,4.97409332259002,58.5656622481056));
#23582=CARTESIAN_POINT('Ctrl Pts',(4.45137708685774,5.1002088182202,58.5744117930418));
#23583=CARTESIAN_POINT('Ctrl Pts',(4.30944892636181,5.22068366307826,58.583161337978));
#23584=CARTESIAN_POINT('Ctrl Pts',(4.16280009466788,5.33510865604752,58.5919108829141));
#23585=CARTESIAN_POINT('Ctrl Pts',(4.01615988348915,5.44952692272799,58.6006599135224));
#23586=CARTESIAN_POINT('Ctrl Pts',(3.86479978232356,5.55789587288539,58.6094089441307));
#23587=CARTESIAN_POINT('Ctrl Pts',(3.70923383581191,5.65984746713797,58.618157974739));
#23588=CARTESIAN_POINT('Ctrl Pts',(3.55366577799659,5.7618004450531,58.626907124087));
#23589=CARTESIAN_POINT('Ctrl Pts',(3.39389200026952,5.85733573570994,58.635656273435));
#23590=CARTESIAN_POINT('Ctrl Pts',(3.23045513626147,5.9461288762187,58.6444054227831));
#23591=CARTESIAN_POINT('Ctrl Pts',(3.18695122151651,5.9697639920665,58.6467342868961));
#23592=CARTESIAN_POINT('Ctrl Pts',(3.14318791262702,5.99292165435313,58.649063151009));
#23593=CARTESIAN_POINT('Ctrl Pts',(3.09917575053262,6.01559628526637,58.651392015122));
#23594=CARTESIAN_POINT('Origin',(0.,0.,-3.69717978381041));
#23595=CARTESIAN_POINT('',(3.09917575053255,6.01559628526641,61.0455262068868));
#23596=CARTESIAN_POINT('',(3.09917575053261,6.01559628526638,60.6511868721373));
#23597=CARTESIAN_POINT('',(3.09917575053259,6.01559628526639,-3.69717978381041));
#23598=CARTESIAN_POINT('',(-6.76765222831417,-0.00200817279939102,59.6960497532493));
#23599=CARTESIAN_POINT('Ctrl Pts',(-6.76699734633338,-0.0059928888702975,
59.69717978381));
#23600=CARTESIAN_POINT('Ctrl Pts',(-6.76681265505105,-0.214540960501165,
59.7069683551803));
#23601=CARTESIAN_POINT('Ctrl Pts',(-6.75698359187389,-0.422659502131963,
59.7167569265505));
#23602=CARTESIAN_POINT('Ctrl Pts',(-6.73765166604857,-0.629554625900658,
59.7265454979208));
#23603=CARTESIAN_POINT('Ctrl Pts',(-6.71817163684709,-0.838034789184822,
59.736409060292));
#23604=CARTESIAN_POINT('Ctrl Pts',(-6.6890426811903,-1.04527270412106,59.7462726226633));
#23605=CARTESIAN_POINT('Ctrl Pts',(-6.65045814561019,-1.25047808996683,
59.7561361850345));
#23606=CARTESIAN_POINT('Ctrl Pts',(-6.61153030721492,-1.45750927429865,
59.766087507662));
#23607=CARTESIAN_POINT('Ctrl Pts',(-6.56297792934071,-1.66247158939489,
59.7760388302894));
#23608=CARTESIAN_POINT('Ctrl Pts',(-6.50504769461876,-1.86457595467043,
59.7859901529169));
#23609=CARTESIAN_POINT('Ctrl Pts',(-6.47109324051564,-1.98303470816466,
59.7918228882587));
#23610=CARTESIAN_POINT('Ctrl Pts',(-6.43391797308779,-2.10051205147262,
59.7976556236004));
#23611=CARTESIAN_POINT('Ctrl Pts',(-6.39357906915677,-2.21685265329938,
59.8034883589422));
#23612=CARTESIAN_POINT('Ctrl Pts',(-6.33718716150031,-2.37949139247111,
59.8116422511089));
#23613=CARTESIAN_POINT('Ctrl Pts',(-6.27449306449052,-2.54024340953854,
59.8197961432757));
#23614=CARTESIAN_POINT('Ctrl Pts',(-6.20563962095389,-2.69857849521693,
59.8279500354424));
#23615=CARTESIAN_POINT('Ctrl Pts',(-6.13687019785494,-2.85672036785448,
59.8360939775826));
#23616=CARTESIAN_POINT('Ctrl Pts',(-6.06195653347624,-3.01245084821206,
59.8442379197229));
#23617=CARTESIAN_POINT('Ctrl Pts',(-5.98109130842289,-3.16525445427506,
59.8523818618631));
#23618=CARTESIAN_POINT('Ctrl Pts',(-5.90030774101968,-3.31790375935895,
59.860517580256));
#23619=CARTESIAN_POINT('Ctrl Pts',(-5.81358474718157,-3.46763175332366,
59.8686532986489));
#23620=CARTESIAN_POINT('Ctrl Pts',(-5.72116319629874,-3.61394253984714,
59.8767890170418));
#23621=CARTESIAN_POINT('Ctrl Pts',(-5.6288155317408,-3.76013635834526,59.884918231342));
#23622=CARTESIAN_POINT('Ctrl Pts',(-5.53077857539011,-3.90291810117333,
59.8930474456422));
#23623=CARTESIAN_POINT('Ctrl Pts',(-5.42733925560266,-4.04181612701448,
59.9011766599424));
#23624=CARTESIAN_POINT('Ctrl Pts',(-5.32396088088463,-4.18063231598893,
59.9093010846179));
#23625=CARTESIAN_POINT('Ctrl Pts',(-5.21518669939534,-4.31556905237643,
59.9174255092933));
#23626=CARTESIAN_POINT('Ctrl Pts',(-5.10134710952039,-4.44618338220411,
59.9255499339687));
#23627=CARTESIAN_POINT('Ctrl Pts',(-4.98681644045892,-4.5775906246284,59.9337236791029));
#23628=CARTESIAN_POINT('Ctrl Pts',(-4.86715886167765,-4.70462249188359,
59.9418974242371));
#23629=CARTESIAN_POINT('Ctrl Pts',(-4.7427525719935,-4.82686099249285,59.9500711693713));
#23630=CARTESIAN_POINT('Ctrl Pts',(-4.61914294378451,-4.94831671351384,
59.9581925722334));
#23631=CARTESIAN_POINT('Ctrl Pts',(-4.49084552583913,-5.06504003602356,
59.9663139750956));
#23632=CARTESIAN_POINT('Ctrl Pts',(-4.35826863593558,-5.17665756033951,
59.9744353779577));
#23633=CARTESIAN_POINT('Ctrl Pts',(-4.22568149588488,-5.28828371433481,
59.982557408724));
#23634=CARTESIAN_POINT('Ctrl Pts',(-4.08881450476893,-5.39480304807199,
59.9906794394903));
#23635=CARTESIAN_POINT('Ctrl Pts',(-3.94810925875312,-5.49588230231943,
59.9988014702565));
#23636=CARTESIAN_POINT('Ctrl Pts',(-3.80736634062081,-5.59698861930653,
60.0069256755977));
#23637=CARTESIAN_POINT('Ctrl Pts',(-3.66278341847713,-5.69265174318178,
60.0150498809388));
#23638=CARTESIAN_POINT('Ctrl Pts',(-3.51483122164988,-5.78258164519233,
60.0231740862799));
#23639=CARTESIAN_POINT('Ctrl Pts',(-3.36527754466686,-5.87348497616553,
60.0313862305223));
#23640=CARTESIAN_POINT('Ctrl Pts',(-3.21228155414851,-5.95853004384766,
60.0395983747647));
#23641=CARTESIAN_POINT('Ctrl Pts',(-3.05635434741772,-6.03746528793507,
60.0478105190072));
#23642=CARTESIAN_POINT('Ctrl Pts',(-2.90185058423,-6.11567994024203,60.0559476954236));
#23643=CARTESIAN_POINT('Ctrl Pts',(-2.74446925827017,-6.18789576148942,
60.0640848718401));
#23644=CARTESIAN_POINT('Ctrl Pts',(-2.58472673772144,-6.25391690793121,
60.0722220482565));
#23645=CARTESIAN_POINT('Ctrl Pts',(-2.42277665483177,-6.32085043384523,
60.0804716764119));
#23646=CARTESIAN_POINT('Ctrl Pts',(-2.25840000661337,-6.38141668080218,
60.0887213045673));
#23647=CARTESIAN_POINT('Ctrl Pts',(-2.09214928617978,-6.43546426952535,
60.0969709327227));
#23648=CARTESIAN_POINT('Ctrl Pts',(-1.92589856574613,-6.48951185824855,
60.1052205608782));
#23649=CARTESIAN_POINT('Ctrl Pts',(-1.75777416057214,-6.53704074493859,
60.1134701890336));
#23650=CARTESIAN_POINT('Ctrl Pts',(-1.58833733130281,-6.57795359682553,
60.121719817189));
#23651=CARTESIAN_POINT('Ctrl Pts',(-1.41940905063369,-6.61874365266129,
60.1299446848666));
#23652=CARTESIAN_POINT('Ctrl Pts',(-1.24867130851606,-6.65307942640394,
60.1381695525442));
#23653=CARTESIAN_POINT('Ctrl Pts',(-1.07665842662517,-6.68080052331882,
60.1463944202218));
#23654=CARTESIAN_POINT('Ctrl Pts',(-0.904839336499182,-6.7084903893152,
60.1546100216653));
#23655=CARTESIAN_POINT('Ctrl Pts',(-0.731748318183226,-6.72958036109917,
60.1628256231089));
#23656=CARTESIAN_POINT('Ctrl Pts',(-0.557933309136579,-6.74396021804369,
60.1710412245524));
#23657=CARTESIAN_POINT('Ctrl Pts',(-0.384279199229741,-6.75832676367162,
60.1792492208806));
#23658=CARTESIAN_POINT('Ctrl Pts',(-0.209902788589785,-6.76599553539176,
60.1874572172087));
#23659=CARTESIAN_POINT('Ctrl Pts',(-0.0353607199741979,-6.76690761127141,
60.1956652135368));
#23660=CARTESIAN_POINT('Ctrl Pts',(0.139054834150475,-6.76781902604502,
60.2038672604083));
#23661=CARTESIAN_POINT('Ctrl Pts',(0.313635449772633,-6.76198349800724,
60.2120693072797));
#23662=CARTESIAN_POINT('Ctrl Pts',(0.487820776911681,-6.74939403869809,
60.2202713541511));
#23663=CARTESIAN_POINT('Ctrl Pts',(0.661914826112078,-6.73681117661452,
60.2284691029227));
#23664=CARTESIAN_POINT('Ctrl Pts',(0.835613642499457,-6.71748145980735,
60.2366668516943));
#23665=CARTESIAN_POINT('Ctrl Pts',(1.00835820546982,-6.69144997212575,60.2448646004659));
#23666=CARTESIAN_POINT('Ctrl Pts',(1.18106982088387,-6.66542344942765,60.2530607856815));
#23667=CARTESIAN_POINT('Ctrl Pts',(1.35282719007815,-6.63269774918149,60.2612569708971));
#23668=CARTESIAN_POINT('Ctrl Pts',(1.52307742835258,-6.59336971109939,60.2694531561128));
#23669=CARTESIAN_POINT('Ctrl Pts',(1.69331507189868,-6.55404458241679,60.2776487349931));
#23670=CARTESIAN_POINT('Ctrl Pts',(1.86204545674993,-6.5081181685023,60.2858443138735));
#23671=CARTESIAN_POINT('Ctrl Pts',(2.02872694719519,-6.45573822066261,60.2940398927538));
#23672=CARTESIAN_POINT('Ctrl Pts',(2.19542643264329,-6.40335261786204,60.3022363564323));
#23673=CARTESIAN_POINT('Ctrl Pts',(2.36007624059371,-6.34451220064319,60.3104328201107));
#23674=CARTESIAN_POINT('Ctrl Pts',(2.52215087996938,-6.27941429901465,60.3186292837891));
#23675=CARTESIAN_POINT('Ctrl Pts',(2.68427250467484,-6.21429752554788,60.3268281236169));
#23676=CARTESIAN_POINT('Ctrl Pts',(2.84381714090245,-6.14291978804291,60.3350269634447));
#23677=CARTESIAN_POINT('Ctrl Pts',(3.00028018016918,-6.06552618001802,60.3432258032725));
#23678=CARTESIAN_POINT('Ctrl Pts',(3.15690664953161,-5.9880517321678,60.3514332070217));
#23679=CARTESIAN_POINT('Ctrl Pts',(3.31044476909495,-5.9045490189965,60.359640610771));
#23680=CARTESIAN_POINT('Ctrl Pts',(3.46041453008442,-5.81530913021661,60.3678480145202));
#23681=CARTESIAN_POINT('Ctrl Pts',(3.61046462281412,-5.7260214398298,60.3760598145893));
#23682=CARTESIAN_POINT('Ctrl Pts',(3.7569422457987,-5.63099064257468,60.3842716146583));
#23683=CARTESIAN_POINT('Ctrl Pts',(3.89939731408626,-5.53055056815294,60.3924834147273));
#23684=CARTESIAN_POINT('Ctrl Pts',(4.04206209613958,-5.42996263190717,60.4007073037134));
#23685=CARTESIAN_POINT('Ctrl Pts',(4.18069220397646,-5.32394972221459,60.4089311926996));
#23686=CARTESIAN_POINT('Ctrl Pts',(4.31487051633804,-5.2128860938291,60.4171550816857));
#23687=CARTESIAN_POINT('Ctrl Pts',(4.43884895730922,-5.11026522124924,60.4247538129358));
#23688=CARTESIAN_POINT('Ctrl Pts',(4.55902693142482,-5.0033329036962,60.4323525441859));
#23689=CARTESIAN_POINT('Ctrl Pts',(4.67510465874965,-4.8924110037626,60.439951275436));
#23690=CARTESIAN_POINT('Ctrl Pts',(4.80074690998782,-4.77234940761958,60.448176123758));
#23691=CARTESIAN_POINT('Ctrl Pts',(4.92193756477516,-4.64727625819529,60.45640097208));
#23692=CARTESIAN_POINT('Ctrl Pts',(5.03825283089154,-4.5175543618216,60.4646258204021));
#23693=CARTESIAN_POINT('Ctrl Pts',(5.15443710022891,-4.3879785610651,60.4728414057213));
#23694=CARTESIAN_POINT('Ctrl Pts',(5.26575667708866,-4.25376470329733,60.4810569910405));
#23695=CARTESIAN_POINT('Ctrl Pts',(5.37182261935113,-4.11531417345354,60.4892725763597));
#23696=CARTESIAN_POINT('Ctrl Pts',(5.47779041860503,-3.97699175213588,60.4974805597829));
#23697=CARTESIAN_POINT('Ctrl Pts',(5.5785140476264,-3.83444074891005,60.5056885432062));
#23698=CARTESIAN_POINT('Ctrl Pts',(5.67364301506104,-3.68809760413809,60.5138965266294));
#23699=CARTESIAN_POINT('Ctrl Pts',(5.76870306662689,-3.54186047717789,60.5220985638059));
#23700=CARTESIAN_POINT('Ctrl Pts',(5.85817633474329,-3.39183698016989,60.5303006009824));
#23701=CARTESIAN_POINT('Ctrl Pts',(5.94175401476835,-3.23849474725283,60.538502638159));
#23702=CARTESIAN_POINT('Ctrl Pts',(6.02528793035647,-3.08523281013342,60.5467003804384));
#23703=CARTESIAN_POINT('Ctrl Pts',(6.10293223666537,-2.92865591338539,60.5548981227178));
#23704=CARTESIAN_POINT('Ctrl Pts',(6.17442265531003,-2.76925872276215,60.5630958649972));
#23705=CARTESIAN_POINT('Ctrl Pts',(6.24589948123463,-2.60989183887696,60.5712920486115));
#23706=CARTESIAN_POINT('Ctrl Pts',(6.31122459774818,-2.44770605369602,60.5794882322259));
#23707=CARTESIAN_POINT('Ctrl Pts',(6.37018058473801,-2.28321885018212,60.5876844158402));
#23708=CARTESIAN_POINT('Ctrl Pts',(6.42913223174462,-2.11874375522138,60.5958799961011));
#23709=CARTESIAN_POINT('Ctrl Pts',(6.48171556105628,-1.95196791680613,60.604075576362));
#23710=CARTESIAN_POINT('Ctrl Pts',(6.52776206483786,-1.7834268767919,60.6122711566229));
#23711=CARTESIAN_POINT('Ctrl Pts',(6.57381355657095,-1.61486757970135,60.6204676246636));
#23712=CARTESIAN_POINT('Ctrl Pts',(6.61332671744159,-1.44454304626998,60.6286640927043));
#23713=CARTESIAN_POINT('Ctrl Pts',(6.64618347708717,-1.27300203805553,60.636860560745));
#23714=CARTESIAN_POINT('Ctrl Pts',(6.67904977383951,-1.1014112378066,60.6450594079184));
#23715=CARTESIAN_POINT('Ctrl Pts',(6.70525575336807,-0.928603611784166,
60.6532582550918));
#23716=CARTESIAN_POINT('Ctrl Pts',(6.72473481698215,-0.755136173989895,
60.6614571022652));
#23717=CARTESIAN_POINT('Ctrl Pts',(6.74423423811189,-0.581487445854731,
60.6696645180311));
#23718=CARTESIAN_POINT('Ctrl Pts',(6.75699265764824,-0.407177885348716,
60.6778719337971));
#23719=CARTESIAN_POINT('Ctrl Pts',(6.76299547117577,-0.232768676707155,
60.6860793495631));
#23720=CARTESIAN_POINT('Ctrl Pts',(6.76900150200023,-0.0582659908640812,
60.6942911642152));
#23721=CARTESIAN_POINT('Ctrl Pts',(6.76824471028132,0.116336091098023,60.7025029788674));
#23722=CARTESIAN_POINT('Ctrl Pts',(6.76076262469402,0.29047845452012,60.7107147935195));
#23723=CARTESIAN_POINT('Ctrl Pts',(6.75326952059825,0.464877269046196,60.7189387013171));
#23724=CARTESIAN_POINT('Ctrl Pts',(6.73903135900979,0.638814654417665,60.7271626091147));
#23725=CARTESIAN_POINT('Ctrl Pts',(6.71813749751791,0.811737374058775,60.7353865169123));
#23726=CARTESIAN_POINT('Ctrl Pts',(6.69883195537331,0.971514773420187,60.7429852558358));
#23727=CARTESIAN_POINT('Ctrl Pts',(6.67384477093599,1.1304257897702,60.7505839947593));
#23728=CARTESIAN_POINT('Ctrl Pts',(6.64328465932267,1.28804422874686,60.7581827336827));
#23729=CARTESIAN_POINT('Ctrl Pts',(6.61050133861164,1.45712920789633,60.7663342711601));
#23730=CARTESIAN_POINT('Ctrl Pts',(6.57120696873145,1.62522739997276,60.7744858086374));
#23731=CARTESIAN_POINT('Ctrl Pts',(6.5254704576766,1.79179360027598,60.7826373461148));
#23732=CARTESIAN_POINT('Ctrl Pts',(6.4797877416664,1.95816388628719,60.7907792957964));
#23733=CARTESIAN_POINT('Ctrl Pts',(6.42767806415106,2.12300541842217,60.7989212454781));
#23734=CARTESIAN_POINT('Ctrl Pts',(6.36926173053051,2.28578083113835,60.8070631951598));
#23735=CARTESIAN_POINT('Ctrl Pts',(6.31090181179256,2.4483990454268,60.8151972818499));
#23736=CARTESIAN_POINT('Ctrl Pts',(6.24624748588144,2.60895477103907,60.8233313685401));
#23737=CARTESIAN_POINT('Ctrl Pts',(6.17546947516548,2.76692351923566,60.8314654552303));
#23738=CARTESIAN_POINT('Ctrl Pts',(6.10474493038905,2.92477293732599,60.8395933974049));
#23739=CARTESIAN_POINT('Ctrl Pts',(6.02790606129483,3.08003893707896,60.8477213395795));
#23740=CARTESIAN_POINT('Ctrl Pts',(5.94517252486965,3.23221482106852,60.8558492817541));
#23741=CARTESIAN_POINT('Ctrl Pts',(5.86248222417664,3.38431117943829,60.8639729763461));
#23742=CARTESIAN_POINT('Ctrl Pts',(5.77390356492504,3.53332031724075,60.8720966709381));
#23743=CARTESIAN_POINT('Ctrl Pts',(5.67970318818474,3.67875803690921,60.8802203655301));
#23744=CARTESIAN_POINT('Ctrl Pts',(5.58552832753847,3.82415636180389,60.8883418596536));
#23745=CARTESIAN_POINT('Ctrl Pts',(5.48573497913876,3.96598488739328,60.8964633537772));
#23746=CARTESIAN_POINT('Ctrl Pts',(5.38063437906526,4.10378638318577,60.9045848479008));
#23747=CARTESIAN_POINT('Ctrl Pts',(5.27554223581709,4.24157679090475,60.9127056885356));
#23748=CARTESIAN_POINT('Ctrl Pts',(5.16514391309833,4.37534052320748,60.9208265291705));
#23749=CARTESIAN_POINT('Ctrl Pts',(5.04979236142588,4.50465160767011,60.9289473698053));
#23750=CARTESIAN_POINT('Ctrl Pts',(4.93442812738708,4.63397690928476,60.9370691032888));
#23751=CARTESIAN_POINT('Ctrl Pts',(4.81410982419634,4.75884831586788,60.9451908367723));
#23752=CARTESIAN_POINT('Ctrl Pts',(4.68922881402648,4.87887508855308,60.9533125702557));
#23753=CARTESIAN_POINT('Ctrl Pts',(4.56425269415373,4.99899327394125,60.9614404892726));
#23754=CARTESIAN_POINT('Ctrl Pts',(4.43470718941319,5.11425920068743,60.9695684082895));
#23755=CARTESIAN_POINT('Ctrl Pts',(4.30101898063026,5.22432050397544,60.9776963273064));
#23756=CARTESIAN_POINT('Ctrl Pts',(4.16727776249131,5.33442544820131,60.9858274691636));
#23757=CARTESIAN_POINT('Ctrl Pts',(4.02939085683188,5.43932143362197,60.9939586110208));
#23758=CARTESIAN_POINT('Ctrl Pts',(3.88781555167283,5.53869833410079,61.002089752878));
#23759=CARTESIAN_POINT('Ctrl Pts',(3.74607089457628,5.63819410891734,61.0102306211817));
#23760=CARTESIAN_POINT('Ctrl Pts',(3.60062932981021,5.73215740947761,61.0183714894854));
#23761=CARTESIAN_POINT('Ctrl Pts',(3.45197527296536,5.82032264697033,61.0265123577891));
#23762=CARTESIAN_POINT('Ctrl Pts',(3.33624290883387,5.88896235708532,61.0328503074883));
#23763=CARTESIAN_POINT('Ctrl Pts',(3.21856396001261,5.95408865972539,61.0391882571876));
#23764=CARTESIAN_POINT('Ctrl Pts',(3.09917575053255,6.01559628526641,61.0455262068868));
#23765=CARTESIAN_POINT('Ctrl Pts',(3.09917575053261,6.01559628526638,59.0457515827422));
#23766=CARTESIAN_POINT('Ctrl Pts',(2.93382384459273,6.10078395293755,59.0545010306546));
#23767=CARTESIAN_POINT('Ctrl Pts',(2.76495772122997,6.17915010267043,59.063250478567));
#23768=CARTESIAN_POINT('Ctrl Pts',(2.5931509331673,6.25042856433169,59.0719999264794));
#23769=CARTESIAN_POINT('Ctrl Pts',(2.42134553245641,6.32170645041442,59.0807493037394));
#23770=CARTESIAN_POINT('Ctrl Pts',(2.24659977927619,6.38589665313447,59.0894986809994));
#23771=CARTESIAN_POINT('Ctrl Pts',(2.06950718689952,6.44278115439065,59.0982480582594));
#23772=CARTESIAN_POINT('Ctrl Pts',(1.89241596572899,6.49966521519713,59.1069973677741));
#23773=CARTESIAN_POINT('Ctrl Pts',(1.7129782145724,6.54924360009535,59.1157466772888));
#23774=CARTESIAN_POINT('Ctrl Pts',(1.53180337335892,6.59134792173545,59.1244959868034));
#23775=CARTESIAN_POINT('Ctrl Pts',(1.35062987477835,6.63345193135294,59.1332452314795));
#23776=CARTESIAN_POINT('Ctrl Pts',(1.1677195910301,6.66808192368227,59.1419944761557));
#23777=CARTESIAN_POINT('Ctrl Pts',(0.983693746907481,6.69512028363159,59.1507437208318));
#23778=CARTESIAN_POINT('Ctrl Pts',(0.799669205420618,6.72215845218858,59.1594929035759));
#23779=CARTESIAN_POINT('Ctrl Pts',(0.614529402874333,6.74160505424571,59.1682420863201));
#23780=CARTESIAN_POINT('Ctrl Pts',(0.428903127364216,6.75339404354116,59.1769912690643));
#23781=CARTESIAN_POINT('Ctrl Pts',(0.243278104164918,6.76518295330326,59.1857403927829));
#23782=CARTESIAN_POINT('Ctrl Pts',(0.0571669005402259,6.76931433552275,
59.1944895165015));
#23783=CARTESIAN_POINT('Ctrl Pts',(-0.128798404776336,6.76577415902475,
59.2032386402201));
#23784=CARTESIAN_POINT('Ctrl Pts',(-0.314762517257839,6.76223400523447,
59.2119877078193));
#23785=CARTESIAN_POINT('Ctrl Pts',(-0.50058044681817,6.75102239665099,59.2207367754185));
#23786=CARTESIAN_POINT('Ctrl Pts',(-0.685621118841192,6.73217741012512,
59.2294858430177));
#23787=CARTESIAN_POINT('Ctrl Pts',(-0.870660665413108,6.7133325382179,59.2382348574035));
#23788=CARTESIAN_POINT('Ctrl Pts',(-1.05492267885353,6.68685441030633,59.2469838717893));
#23789=CARTESIAN_POINT('Ctrl Pts',(-1.23778137635122,6.65283295028201,59.2557328861751));
#23790=CARTESIAN_POINT('Ctrl Pts',(-1.42999922978717,6.61707018861893,59.2649296965425));
#23791=CARTESIAN_POINT('Ctrl Pts',(-1.62066601233565,6.57297172934445,59.2741265069099));
#23792=CARTESIAN_POINT('Ctrl Pts',(-1.80906628500255,6.5207030431133,59.2833233172772));
#23793=CARTESIAN_POINT('Ctrl Pts',(-1.98831342545394,6.47097374915072,59.292073315015));
#23794=CARTESIAN_POINT('Ctrl Pts',(-2.16550875896565,6.41384933989575,59.3008233127528));
#23795=CARTESIAN_POINT('Ctrl Pts',(-2.34005036713871,6.34952386240527,59.3095733104905));
#23796=CARTESIAN_POINT('Ctrl Pts',(-2.51458843546951,6.28519968948651,59.3183231307714));
#23797=CARTESIAN_POINT('Ctrl Pts',(-2.68647261717919,6.21367483971158,59.3270729510523));
#23798=CARTESIAN_POINT('Ctrl Pts',(-2.85511905908597,6.13519226743906,59.3358227713331));
#23799=CARTESIAN_POINT('Ctrl Pts',(-3.02376230488747,6.05671118253005,59.3445724257917));
#23800=CARTESIAN_POINT('Ctrl Pts',(-3.18916767379764,5.97127275992708,59.3533220802502));
#23801=CARTESIAN_POINT('Ctrl Pts',(-3.35077334102644,5.87916720438078,59.3620717347087));
#23802=CARTESIAN_POINT('Ctrl Pts',(-3.51237616037225,5.7870632719573,59.3708212349771));
#23803=CARTESIAN_POINT('Ctrl Pts',(-3.67017916302158,5.6882925836239,59.3795707352456));
#23804=CARTESIAN_POINT('Ctrl Pts',(-3.82364636566321,5.58319061741139,59.388320235514));
#23805=CARTESIAN_POINT('Ctrl Pts',(-3.97711106778666,5.47809036367798,59.3970695932225));
#23806=CARTESIAN_POINT('Ctrl Pts',(-4.12623987481805,5.36665920043319,59.4058189509309));
#23807=CARTESIAN_POINT('Ctrl Pts',(-4.27052628213816,5.24927559512427,59.4145683086394));
#23808=CARTESIAN_POINT('Ctrl Pts',(-4.4148105302487,5.1318937464313,59.4233175354159));
#23809=CARTESIAN_POINT('Ctrl Pts',(-4.55425230136426,5.00855981477448,59.4320667621924));
#23810=CARTESIAN_POINT('Ctrl Pts',(-4.68837800630449,4.87969268192172,59.4408159889689));
#23811=CARTESIAN_POINT('Ctrl Pts',(-4.82250188228786,4.75082730631919,59.4495650964398));
#23812=CARTESIAN_POINT('Ctrl Pts',(-4.95130963052849,4.6164290790365,59.4583142039106));
#23813=CARTESIAN_POINT('Ctrl Pts',(-5.07436379033244,4.47695444731829,59.4670633113814));
#23814=CARTESIAN_POINT('Ctrl Pts',(-5.19741643562668,4.33748153220749,59.4758123111712));
#23815=CARTESIAN_POINT('Ctrl Pts',(-5.31471544462624,4.19293255254776,59.4845613109609));
#23816=CARTESIAN_POINT('Ctrl Pts',(-5.42586245275469,4.04379841779816,59.4933103107506));
#23817=CARTESIAN_POINT('Ctrl Pts',(-5.53702160019002,3.89464799484558,59.5020602660928));
#23818=CARTESIAN_POINT('Ctrl Pts',(-5.64202723081108,3.74091164444066,59.510810221435));
#23819=CARTESIAN_POINT('Ctrl Pts',(-5.74052265232831,3.5831115916345,59.5195601767771));
#23820=CARTESIAN_POINT('Ctrl Pts',(-5.83901427066792,3.42531763191999,59.5283097942596));
#23821=CARTESIAN_POINT('Ctrl Pts',(-5.93099603115622,3.26346052695826,59.537059411742));
#23822=CARTESIAN_POINT('Ctrl Pts',(-6.01615550622645,3.09809004467287,59.5458090292245));
#23823=CARTESIAN_POINT('Ctrl Pts',(-6.10131214578696,2.93272506864043,59.5545583553756));
#23824=CARTESIAN_POINT('Ctrl Pts',(-6.17964682328649,2.76384720417114,59.5633076815266));
#23825=CARTESIAN_POINT('Ctrl Pts',(-6.25089348288471,2.59203002791816,59.5720570076777));
#23826=CARTESIAN_POINT('Ctrl Pts',(-6.32213814889247,2.42021765937248,59.5808060890093));
#23827=CARTESIAN_POINT('Ctrl Pts',(-6.3862950841251,2.24546640832132,59.5895551703409));
#23828=CARTESIAN_POINT('Ctrl Pts',(-6.44314639819745,2.0683697666025,59.5983042516725));
#23829=CARTESIAN_POINT('Ctrl Pts',(-6.50000285283642,1.89125711158476,59.6070541241069));
#23830=CARTESIAN_POINT('Ctrl Pts',(-6.54955227673199,1.71179891440447,59.6158039965413));
#23831=CARTESIAN_POINT('Ctrl Pts',(-6.59162635926342,1.53060476278615,59.6245538689757));
#23832=CARTESIAN_POINT('Ctrl Pts',(-6.63369752055164,1.34942319164859,59.6333031338982));
#23833=CARTESIAN_POINT('Ctrl Pts',(-6.6682943142423,1.16650618642847,59.6420523988207));
#23834=CARTESIAN_POINT('Ctrl Pts',(-6.695299237454,0.98247499761977,59.6508016637432));
#23835=CARTESIAN_POINT('Ctrl Pts',(-6.7223055473143,0.798434359178909,59.6595513779229));
#23836=CARTESIAN_POINT('Ctrl Pts',(-6.74171916496693,0.613279706241456,
59.6683010921026));
#23837=CARTESIAN_POINT('Ctrl Pts',(-6.75347414817268,0.427639953656448,
59.6770508062823));
#23838=CARTESIAN_POINT('Ctrl Pts',(-6.7624883775874,0.285283364199705,59.6837604654582));
#23839=CARTESIAN_POINT('Ctrl Pts',(-6.76699999999994,0.142641701106312,
59.6904701246341));
#23840=CARTESIAN_POINT('Ctrl Pts',(-6.767,2.82448417516006E-12,59.69717978381));
#23841=CARTESIAN_POINT('',(-6.76699904389988,-0.00254360543768349,59.3028202161898));
#23842=CARTESIAN_POINT('Ctrl Pts',(3.09917575053262,6.01559628526637,58.651392015122));
#23843=CARTESIAN_POINT('Ctrl Pts',(2.93382384459268,6.10078395293758,58.6601414630344));
#23844=CARTESIAN_POINT('Ctrl Pts',(2.76495772122987,6.17915010267048,58.6688909109468));
#23845=CARTESIAN_POINT('Ctrl Pts',(2.59315093316714,6.25042856433176,58.6776403588593));
#23846=CARTESIAN_POINT('Ctrl Pts',(2.42134553245624,6.32170645041448,58.6863897361193));
#23847=CARTESIAN_POINT('Ctrl Pts',(2.24659977927602,6.38589665313453,58.6951391133793));
#23848=CARTESIAN_POINT('Ctrl Pts',(2.06950718689935,6.4427811543907,58.7038884906393));
#23849=CARTESIAN_POINT('Ctrl Pts',(1.89241596572876,6.4996652151972,58.7126378001539));
#23850=CARTESIAN_POINT('Ctrl Pts',(1.7129782145721,6.54924360009543,58.7213871096686));
#23851=CARTESIAN_POINT('Ctrl Pts',(1.53180337335855,6.59134792173554,58.7301364191833));
#23852=CARTESIAN_POINT('Ctrl Pts',(1.35062987477805,6.633451931353,58.7388856638594));
#23853=CARTESIAN_POINT('Ctrl Pts',(1.16771959102986,6.66808192368232,58.7476349085355));
#23854=CARTESIAN_POINT('Ctrl Pts',(0.983693746907299,6.69512028363162,58.7563841532116));
#23855=CARTESIAN_POINT('Ctrl Pts',(0.799669205420246,6.72215845218863,58.7651333359558));
#23856=CARTESIAN_POINT('Ctrl Pts',(0.614529402873771,6.74160505424577,58.7738825186999));
#23857=CARTESIAN_POINT('Ctrl Pts',(0.428903127363461,6.75339404354121,58.7826317014441));
#23858=CARTESIAN_POINT('Ctrl Pts',(0.243278104164161,6.76518295330329,58.7913808251627));
#23859=CARTESIAN_POINT('Ctrl Pts',(0.0571669005394668,6.76931433552275,
58.8001299488813));
#23860=CARTESIAN_POINT('Ctrl Pts',(-0.128798404777095,6.76577415902474,
58.8088790726));
#23861=CARTESIAN_POINT('Ctrl Pts',(-0.314762517258661,6.76223400523443,
58.8176281401992));
#23862=CARTESIAN_POINT('Ctrl Pts',(-0.500580446819053,6.75102239665092,
58.8263772077984));
#23863=CARTESIAN_POINT('Ctrl Pts',(-0.685621118842137,6.73217741012502,
58.8351262753976));
#23864=CARTESIAN_POINT('Ctrl Pts',(-0.870660665413986,6.71333253821778,
58.8438752897834));
#23865=CARTESIAN_POINT('Ctrl Pts',(-1.05492267885434,6.6868544103062,58.8526243041691));
#23866=CARTESIAN_POINT('Ctrl Pts',(-1.23778137635196,6.65283295028188,58.8613733185549));
#23867=CARTESIAN_POINT('Ctrl Pts',(-1.42999922978791,6.61707018861877,58.8705701289223));
#23868=CARTESIAN_POINT('Ctrl Pts',(-1.62066601233639,6.57297172934427,58.8797669392897));
#23869=CARTESIAN_POINT('Ctrl Pts',(-1.80906628500328,6.5207030431131,58.8889637496571));
#23870=CARTESIAN_POINT('Ctrl Pts',(-1.98831342545466,6.47097374915049,58.8977137473948));
#23871=CARTESIAN_POINT('Ctrl Pts',(-2.16550875896637,6.4138493398955,58.9064637451326));
#23872=CARTESIAN_POINT('Ctrl Pts',(-2.34005036713942,6.34952386240501,58.9152137428704));
#23873=CARTESIAN_POINT('Ctrl Pts',(-2.51458843547009,6.28519968948628,58.9239635631512));
#23874=CARTESIAN_POINT('Ctrl Pts',(-2.68647261717965,6.21367483971138,58.9327133834321));
#23875=CARTESIAN_POINT('Ctrl Pts',(-2.85511905908631,6.1351922674389,58.9414632037129));
#23876=CARTESIAN_POINT('Ctrl Pts',(-3.02376230488786,6.05671118252986,58.9502128581715));
#23877=CARTESIAN_POINT('Ctrl Pts',(-3.18916767379808,5.97127275992684,58.95896251263));
#23878=CARTESIAN_POINT('Ctrl Pts',(-3.35077334102693,5.8791672043805,58.9677121670885));
#23879=CARTESIAN_POINT('Ctrl Pts',(-3.51237616037285,5.78706327195694,58.976461667357));
#23880=CARTESIAN_POINT('Ctrl Pts',(-3.67017916302227,5.68829258362346,58.9852111676254));
#23881=CARTESIAN_POINT('Ctrl Pts',(-3.823646365664,5.58319061741085,58.9939606678939));
#23882=CARTESIAN_POINT('Ctrl Pts',(-3.97711106778738,5.47809036367745,59.0027100256023));
#23883=CARTESIAN_POINT('Ctrl Pts',(-4.1262398748187,5.36665920043269,59.0114593833108));
#23884=CARTESIAN_POINT('Ctrl Pts',(-4.27052628213875,5.24927559512379,59.0202087410192));
#23885=CARTESIAN_POINT('Ctrl Pts',(-4.41481053024922,5.13189374643084,59.0289579677957));
#23886=CARTESIAN_POINT('Ctrl Pts',(-4.55425230136473,5.00855981477405,59.0377071945722));
#23887=CARTESIAN_POINT('Ctrl Pts',(-4.68837800630489,4.87969268192133,59.0464564213487));
#23888=CARTESIAN_POINT('Ctrl Pts',(-4.82250188228821,4.75082730631883,59.0552055288196));
#23889=CARTESIAN_POINT('Ctrl Pts',(-4.95130963052879,4.61642907903618,59.0639546362904));
#23890=CARTESIAN_POINT('Ctrl Pts',(-5.07436379033269,4.47695444731801,59.0727037437613));
#23891=CARTESIAN_POINT('Ctrl Pts',(-5.19741643562739,4.33748153220667,59.081452743551));
#23892=CARTESIAN_POINT('Ctrl Pts',(-5.31471544462736,4.19293255254638,59.0902017433408));
#23893=CARTESIAN_POINT('Ctrl Pts',(-5.42586245275617,4.04379841779617,59.0989507431306));
#23894=CARTESIAN_POINT('Ctrl Pts',(-5.53702160019137,3.89464799484365,59.1077006984727));
#23895=CARTESIAN_POINT('Ctrl Pts',(-5.64202723081231,3.7409116444388,59.1164506538149));
#23896=CARTESIAN_POINT('Ctrl Pts',(-5.74052265232942,3.58311159163272,59.125200609157));
#23897=CARTESIAN_POINT('Ctrl Pts',(-5.83901427066901,3.42531763191812,59.1339502266395));
#23898=CARTESIAN_POINT('Ctrl Pts',(-5.9309960311573,3.26346052695631,59.1426998441219));
#23899=CARTESIAN_POINT('Ctrl Pts',(-6.0161555062275,3.09809004467083,59.1514494616044));
#23900=CARTESIAN_POINT('Ctrl Pts',(-6.10131214578804,2.93272506863819,59.1601987877555));
#23901=CARTESIAN_POINT('Ctrl Pts',(-6.17964682328759,2.76384720416869,59.1689481139066));
#23902=CARTESIAN_POINT('Ctrl Pts',(-6.25089348288581,2.59203002791551,59.1776974400577));
#23903=CARTESIAN_POINT('Ctrl Pts',(-6.32213814889339,2.42021765937003,59.1864465213892));
#23904=CARTESIAN_POINT('Ctrl Pts',(-6.38629508412587,2.24546640831909,59.1951956027208));
#23905=CARTESIAN_POINT('Ctrl Pts',(-6.44314639819809,2.0683697666005,59.2039446840524));
#23906=CARTESIAN_POINT('Ctrl Pts',(-6.50000285283701,1.89125711158275,59.2126945564868));
#23907=CARTESIAN_POINT('Ctrl Pts',(-6.54955227673252,1.71179891440244,59.2214444289212));
#23908=CARTESIAN_POINT('Ctrl Pts',(-6.5916263592639,1.5306047627841,59.2301943013556));
#23909=CARTESIAN_POINT('Ctrl Pts',(-6.63369752055203,1.34942319164666,59.2389435662781));
#23910=CARTESIAN_POINT('Ctrl Pts',(-6.66829431424261,1.16650618642665,59.2476928312006));
#23911=CARTESIAN_POINT('Ctrl Pts',(-6.69529923745424,0.982474997618072,
59.2564420961231));
#23912=CARTESIAN_POINT('Ctrl Pts',(-6.7223055473145,0.798434359177204,59.2651918103028));
#23913=CARTESIAN_POINT('Ctrl Pts',(-6.74171916496709,0.613279706239749,
59.2739415244825));
#23914=CARTESIAN_POINT('Ctrl Pts',(-6.75347414817279,0.427639953654739,
59.2826912386622));
#23915=CARTESIAN_POINT('Ctrl Pts',(-6.76248837758744,0.285283364198505,
59.289400897838));
#23916=CARTESIAN_POINT('Ctrl Pts',(-6.76699999999995,0.142641701105622,
59.2961105570139));
#23917=CARTESIAN_POINT('Ctrl Pts',(-6.767,2.6471802258598E-12,59.3028202161898));
#23918=CARTESIAN_POINT('Ctrl Pts',(-6.76699808779975,-0.00508721087801415,
59.3028202161898));
#23919=CARTESIAN_POINT('Ctrl Pts',(-6.76685389172481,-0.196896551357745,
59.3117968853725));
#23920=CARTESIAN_POINT('Ctrl Pts',(-6.75855052427745,-0.388401106019233,
59.3207735545552));
#23921=CARTESIAN_POINT('Ctrl Pts',(-6.74218962523088,-0.578937006442967,
59.3297502237379));
#23922=CARTESIAN_POINT('Ctrl Pts',(-6.72574110339922,-0.770493345059413,
59.3387749685644));
#23923=CARTESIAN_POINT('Ctrl Pts',(-6.70114859654504,-0.961070402327572,
59.3477997133909));
#23924=CARTESIAN_POINT('Ctrl Pts',(-6.66856551188544,-1.15001000590954,
59.3568244582174));
#23925=CARTESIAN_POINT('Ctrl Pts',(-6.63589346638885,-1.33946546688962,
59.3658738430944));
#23926=CARTESIAN_POINT('Ctrl Pts',(-6.59518726618906,-1.52727431190146,
59.3749232279714));
#23927=CARTESIAN_POINT('Ctrl Pts',(-6.54665030744605,-1.71279267630867,
59.3839726128485));
#23928=CARTESIAN_POINT('Ctrl Pts',(-6.49792014969984,-1.89904948754086,
59.3930580183618));
#23929=CARTESIAN_POINT('Ctrl Pts',(-6.44129688469831,-2.08299734195364,
59.4021434238751));
#23930=CARTESIAN_POINT('Ctrl Pts',(-6.37703367310896,-2.26400762631985,
59.4112288293884));
#23931=CARTESIAN_POINT('Ctrl Pts',(-6.3346927207129,-2.38326945037125,59.4172149093372));
#23932=CARTESIAN_POINT('Ctrl Pts',(-6.28903618429288,-2.50125653358099,
59.423200989286));
#23933=CARTESIAN_POINT('Ctrl Pts',(-6.24014724426247,-2.61779513520891,
59.4291870692348));
#23934=CARTESIAN_POINT('Ctrl Pts',(-6.17290706410859,-2.7780783518929,59.4374201193668));
#23935=CARTESIAN_POINT('Ctrl Pts',(-6.09938911658582,-2.9360035466864,59.4456531694988));
#23936=CARTESIAN_POINT('Ctrl Pts',(-6.01977864578517,-3.09104416916823,
59.4538862196308));
#23937=CARTESIAN_POINT('Ctrl Pts',(-5.94026297881782,-3.24590016210093,
59.4621094654656));
#23938=CARTESIAN_POINT('Ctrl Pts',(-5.85466939759303,-3.39787810731453,
59.4703327113005));
#23939=CARTESIAN_POINT('Ctrl Pts',(-5.76323171819324,-3.54646995791751,
59.4785559571353));
#23940=CARTESIAN_POINT('Ctrl Pts',(-5.67188462556532,-3.69491459944695,
59.4867710562488));
#23941=CARTESIAN_POINT('Ctrl Pts',(-5.57470515147535,-3.83997952410623,
59.4949861553623));
#23942=CARTESIAN_POINT('Ctrl Pts',(-5.47197370948423,-3.98117981542073,
59.5032012544759));
#23943=CARTESIAN_POINT('Ctrl Pts',(-5.36932348843731,-4.12226847176974,
59.5114098586148));
#23944=CARTESIAN_POINT('Ctrl Pts',(-5.26113025220341,-4.25949829225545,
59.5196184627536));
#23945=CARTESIAN_POINT('Ctrl Pts',(-5.14771859082211,-4.39241190118874,
59.5278270668925));
#23946=CARTESIAN_POINT('Ctrl Pts',(-5.03437390882547,-4.5252470131524,59.5360308231415));
#23947=CARTESIAN_POINT('Ctrl Pts',(-4.91581717317682,-4.6537707199673,59.5442345793905));
#23948=CARTESIAN_POINT('Ctrl Pts',(-4.79241430671134,-4.77755733747158,
59.5524383356394));
#23949=CARTESIAN_POINT('Ctrl Pts',(-4.66904795204328,-4.90130732963617,
59.5606396646037));
#23950=CARTESIAN_POINT('Ctrl Pts',(-4.54083857255589,-5.02032276832821,
59.568840993568));
#23951=CARTESIAN_POINT('Ctrl Pts',(-4.4081903020088,-5.13421340238946,59.5770423225322));
#23952=CARTESIAN_POINT('Ctrl Pts',(-4.27556032492461,-5.24808832984497,
59.5852425204549));
#23953=CARTESIAN_POINT('Ctrl Pts',(-4.13849294721889,-5.35683962636661,
59.5934427183777));
#23954=CARTESIAN_POINT('Ctrl Pts',(-3.99742687846337,-5.46011605658145,
59.6016429163004));
#23955=CARTESIAN_POINT('Ctrl Pts',(-3.85635470002368,-5.56339695978102,
59.6098434693802));
#23956=CARTESIAN_POINT('Ctrl Pts',(-3.71128377457562,-5.66120231256384,
59.6180440224601));
#23957=CARTESIAN_POINT('Ctrl Pts',(-3.56268344058216,-5.75322307078404,
59.6262445755399));
#23958=CARTESIAN_POINT('Ctrl Pts',(-3.41404974129794,-5.84526449046085,
59.6344469698931));
#23959=CARTESIAN_POINT('Ctrl Pts',(-3.26188535965923,-5.93151854010717,
59.6426493642463));
#23960=CARTESIAN_POINT('Ctrl Pts',(-3.10668601908128,-6.01172113282418,
59.6508517585995));
#23961=CARTESIAN_POINT('Ctrl Pts',(-2.95134153983737,-6.09199872906422,
59.6590618236333));
#23962=CARTESIAN_POINT('Ctrl Pts',(-2.79295674983463,-6.16621339711428,
59.6672718886672));
#23963=CARTESIAN_POINT('Ctrl Pts',(-2.63205008647175,-6.23414800452348,
59.675481953701));
#23964=CARTESIAN_POINT('Ctrl Pts',(-2.47106641603435,-6.30211512423059,
59.6836959479263));
#23965=CARTESIAN_POINT('Ctrl Pts',(-2.30755880086754,-6.3637960643812,59.6919099421516));
#23966=CARTESIAN_POINT('Ctrl Pts',(-2.14206271716062,-6.41902300321089,
59.7001239363769));
#23967=CARTESIAN_POINT('Ctrl Pts',(-1.97634100717147,-6.47432523475208,
59.7083491290121));
#23968=CARTESIAN_POINT('Ctrl Pts',(-1.80862575487906,-6.52315577996311,
59.7165743216473));
#23969=CARTESIAN_POINT('Ctrl Pts',(-1.6394657449671,-6.56539725158192,59.7247995142825));
#23970=CARTESIAN_POINT('Ctrl Pts',(-1.48734051036217,-6.60338491653545,
59.7321964124025));
#23971=CARTESIAN_POINT('Ctrl Pts',(-1.33404717200257,-6.63604440680909,
59.7395933105225));
#23972=CARTESIAN_POINT('Ctrl Pts',(-1.17998895555638,-6.66332612624994,
59.7469902086425));
#23973=CARTESIAN_POINT('Ctrl Pts',(-0.999915882299108,-6.69521474067624,
59.7556361751334));
#23974=CARTESIAN_POINT('Ctrl Pts',(-0.818389007109079,-6.71982792700986,
59.7642821416243));
#23975=CARTESIAN_POINT('Ctrl Pts',(-0.636008931829445,-6.73704546805446,
59.7729281081152));
#23976=CARTESIAN_POINT('Ctrl Pts',(-0.453862145459705,-6.75424098552343,
59.7815630152395));
#23977=CARTESIAN_POINT('Ctrl Pts',(-0.270864637381904,-6.76405969304869,
59.7901979223639));
#23978=CARTESIAN_POINT('Ctrl Pts',(-0.0876255804028921,-6.76643264635503,
59.7988328294883));
#23979=CARTESIAN_POINT('Ctrl Pts',(0.101696865371653,-6.76888437979587,
59.8077544085598));
#23980=CARTESIAN_POINT('Ctrl Pts',(0.291276863503035,-6.76338739230685,
59.8166759876313));
#23981=CARTESIAN_POINT('Ctrl Pts',(0.480435422154191,-6.74992376291314,
59.8255975667027));
#23982=CARTESIAN_POINT('Ctrl Pts',(0.663010220993306,-6.7369287419861,59.8342086256784));
#23983=CARTESIAN_POINT('Ctrl Pts',(0.845192075588722,-6.71651228279546,
59.8428196846541));
#23984=CARTESIAN_POINT('Ctrl Pts',(1.02636874057709,-6.68871110217553,59.8514307436298));
#23985=CARTESIAN_POINT('Ctrl Pts',(1.20737454760633,-6.66093613935238,59.8600336819794));
#23986=CARTESIAN_POINT('Ctrl Pts',(1.38737675453623,-6.62579038585825,59.868636620329));
#23987=CARTESIAN_POINT('Ctrl Pts',(1.56576778775354,-6.58336238064057,59.8772395586785));
#23988=CARTESIAN_POINT('Ctrl Pts',(1.7439590642814,-6.54098188497372,59.8858328637273));
#23989=CARTESIAN_POINT('Ctrl Pts',(1.92054247025903,-6.4913354758701,59.894426168776));
#23990=CARTESIAN_POINT('Ctrl Pts',(2.09491996763691,-6.4345628700943,59.9030194738248));
#23991=CARTESIAN_POINT('Ctrl Pts',(2.11434847511248,-6.42823747253837,59.9039769086652));
#23992=CARTESIAN_POINT('Ctrl Pts',(2.13374960972759,-6.4218236654166,59.9049343435057));
#23993=CARTESIAN_POINT('Ctrl Pts',(2.15312255267417,-6.41532168119151,59.9058917783461));
#23994=CARTESIAN_POINT('Ctrl Pts',(2.32705096379606,-6.35694749465068,59.9144875358937));
#23995=CARTESIAN_POINT('Ctrl Pts',(2.49850201340885,-6.29153030270548,59.9230832934413));
#23996=CARTESIAN_POINT('Ctrl Pts',(2.66691143544978,-6.21931446346518,59.9316790509889));
#23997=CARTESIAN_POINT('Ctrl Pts',(2.83547798920735,-6.14703124439156,59.9402828286705));
#23998=CARTESIAN_POINT('Ctrl Pts',(3.00099697016294,-6.06793683674931,59.9488866063521));
#23999=CARTESIAN_POINT('Ctrl Pts',(3.16292726653382,-5.982322300463,59.9574903840337));
#24000=CARTESIAN_POINT('Ctrl Pts',(3.33122156515136,-5.89334303803536,59.9664322977018));
#24001=CARTESIAN_POINT('Ctrl Pts',(3.49563907118009,-5.79732097715773,59.9753742113698));
#24002=CARTESIAN_POINT('Ctrl Pts',(3.65560508503817,-5.69463260116428,59.9843161250378));
#24003=CARTESIAN_POINT('Ctrl Pts',(3.80994108277038,-5.59555835043932,59.9929433273685));
#24004=CARTESIAN_POINT('Ctrl Pts',(3.9601333743541,-5.49027924038039,60.0015705296993));
#24005=CARTESIAN_POINT('Ctrl Pts',(4.10569899548884,-5.37917510018422,60.01019773203));
#24006=CARTESIAN_POINT('Ctrl Pts',(4.2514032455969,-5.26796515030053,60.0188331504504));
#24007=CARTESIAN_POINT('Ctrl Pts',(4.39247179358532,-5.15091928931802,60.0274685688709));
#24008=CARTESIAN_POINT('Ctrl Pts',(4.52845631495592,-5.02845626445491,60.0361039872913));
#24009=CARTESIAN_POINT('Ctrl Pts',(4.66464173408752,-4.90581231791593,60.0447521633124));
#24010=CARTESIAN_POINT('Ctrl Pts',(4.7957278961417,-4.77773542460653,60.0534003393336));
#24011=CARTESIAN_POINT('Ctrl Pts',(4.92130370304089,-4.64468070618811,60.0620485153547));
#24012=CARTESIAN_POINT('Ctrl Pts',(4.93458914726629,-4.63060402148169,60.0629634595865));
#24013=CARTESIAN_POINT('Ctrl Pts',(4.94781295268266,-4.61647165060833,60.0638784038184));
#24014=CARTESIAN_POINT('Ctrl Pts',(4.96097465947815,-4.60228415333252,60.0647933480502));
#24015=CARTESIAN_POINT('Ctrl Pts',(5.07930766619511,-4.47472856829164,60.0730193405916));
#24016=CARTESIAN_POINT('Ctrl Pts',(5.19287330028552,-4.34243880531907,60.0812453331329));
#24017=CARTESIAN_POINT('Ctrl Pts',(5.30127216306996,-4.20580580306076,60.0894713256743));
#24018=CARTESIAN_POINT('Ctrl Pts',(5.40955738365779,-4.06931604284492,60.0976886943257));
#24019=CARTESIAN_POINT('Ctrl Pts',(5.51268639872425,-3.92849238907775,60.1059060629771));
#24020=CARTESIAN_POINT('Ctrl Pts',(5.61029721093421,-3.78376191177297,60.1141234316285));
#24021=CARTESIAN_POINT('Ctrl Pts',(5.7078252223249,-3.639154205725,60.1223338296909));
#24022=CARTESIAN_POINT('Ctrl Pts',(5.79984415439632,-3.49064657191445,60.1305442277533));
#24023=CARTESIAN_POINT('Ctrl Pts',(5.88603275743845,-3.33869845574014,60.1387546258157));
#24024=CARTESIAN_POINT('Ctrl Pts',(5.97216548994621,-3.18684883776797,60.1469597016045));
#24025=CARTESIAN_POINT('Ctrl Pts',(6.05247524563156,-3.03156349044571,60.1551647773933));
#24026=CARTESIAN_POINT('Ctrl Pts',(6.12668448284336,-2.87333016684238,60.163369853182));
#24027=CARTESIAN_POINT('Ctrl Pts',(6.20086045672258,-2.71516776928363,60.1715712511515));
#24028=CARTESIAN_POINT('Ctrl Pts',(6.26894120819666,-2.55406035175253,60.179772649121));
#24029=CARTESIAN_POINT('Ctrl Pts',(6.33069544938897,-2.39051963536923,60.1879740470905));
#24030=CARTESIAN_POINT('Ctrl Pts',(6.39244485347498,-2.22699172885638,60.1961748026582));
#24031=CARTESIAN_POINT('Ctrl Pts',(6.44786859971942,-2.06103123497598,60.2043755582259));
#24032=CARTESIAN_POINT('Ctrl Pts',(6.49678367114102,-1.89316954613037,60.2125763137936));
#24033=CARTESIAN_POINT('Ctrl Pts',(6.54569849409731,-1.72530870994231,60.2207770277054));
#24034=CARTESIAN_POINT('Ctrl Pts',(6.5881046068,-1.55554704178981,60.2289777416172));
#24035=CARTESIAN_POINT('Ctrl Pts',(6.62386901663486,-1.38443065931981,60.237178455529));
#24036=CARTESIAN_POINT('Ctrl Pts',(6.65963972620516,-1.2132841354902,60.2453806139586));
#24037=CARTESIAN_POINT('Ctrl Pts',(6.6887663287528,-1.04078277271815,60.2535827723882));
#24038=CARTESIAN_POINT('Ctrl Pts',(6.71116704694042,-0.86748248861922,60.2617849308178));
#24039=CARTESIAN_POINT('Ctrl Pts',(6.73357577052176,-0.694120271818259,
60.2699900204707));
#24040=CARTESIAN_POINT('Ctrl Pts',(6.74925377563276,-0.519958920123828,
60.2781951101237));
#24041=CARTESIAN_POINT('Ctrl Pts',(6.75817119392634,-0.345559131820007,
60.2864001997766));
#24042=CARTESIAN_POINT('Ctrl Pts',(6.76709879931602,-0.170960112377284,
60.2946146627744));
#24043=CARTESIAN_POINT('Ctrl Pts',(6.76925037003157,0.00387752958574603,
60.3028291257722));
#24044=CARTESIAN_POINT('Ctrl Pts',(6.76464819222189,0.17839236381944,60.31104358877));
#24045=CARTESIAN_POINT('Ctrl Pts',(6.76004328776732,0.353010592576657,60.3192629185774));
#24046=CARTESIAN_POINT('Ctrl Pts',(6.74867668177691,0.527305275350919,60.3274822483849));
#24047=CARTESIAN_POINT('Ctrl Pts',(6.73062253549272,0.700720546807031,60.3357015781924));
#24048=CARTESIAN_POINT('Ctrl Pts',(6.71254041540346,0.874404514712382,60.343933643353));
#24049=CARTESIAN_POINT('Ctrl Pts',(6.68775009868203,1.04720599381189,60.3521657085137));
#24050=CARTESIAN_POINT('Ctrl Pts',(6.65637706510546,1.2185784205943,60.3603977736744));
#24051=CARTESIAN_POINT('Ctrl Pts',(6.62817672981943,1.37262026300166,60.3677973449355));
#24052=CARTESIAN_POINT('Ctrl Pts',(6.59465848349134,1.5255074604202,60.3751969161967));
#24053=CARTESIAN_POINT('Ctrl Pts',(6.55594747915721,1.67685468974871,60.3825964874578));
#24054=CARTESIAN_POINT('Ctrl Pts',(6.51327697742987,1.84368224489941,60.3907529128389));
#24055=CARTESIAN_POINT('Ctrl Pts',(6.46416488242527,2.00915214045401,60.3989093382201));
#24056=CARTESIAN_POINT('Ctrl Pts',(6.40870973227483,2.17272376694459,60.4070657636012));
#24057=CARTESIAN_POINT('Ctrl Pts',(6.35332336696102,2.33609250429729,60.415212072007));
#24058=CARTESIAN_POINT('Ctrl Pts',(6.29160972490991,2.49756731724697,60.4233583804128));
#24059=CARTESIAN_POINT('Ctrl Pts',(6.22371824315168,2.65661819422004,60.4315046888185));
#24060=CARTESIAN_POINT('Ctrl Pts',(6.15589669331968,2.81550524012171,60.4396426060827));
#24061=CARTESIAN_POINT('Ctrl Pts',(6.08191011608718,2.97197298738088,60.4477805233468));
#24062=CARTESIAN_POINT('Ctrl Pts',(6.00195759739385,3.12550699872618,60.455918440611));
#24063=CARTESIAN_POINT('Ctrl Pts',(5.92202210112849,3.27900832164973,60.4640546252579));
#24064=CARTESIAN_POINT('Ctrl Pts',(5.83612332874608,3.42957681351207,60.4721908099048));
#24065=CARTESIAN_POINT('Ctrl Pts',(5.74450873561673,3.57671754356186,60.4803269945518));
#24066=CARTESIAN_POINT('Ctrl Pts',(5.65300859758315,3.72367444911626,60.4884530145758));
#24067=CARTESIAN_POINT('Ctrl Pts',(5.55580708295737,3.86721182911656,60.4965790345998));
#24068=CARTESIAN_POINT('Ctrl Pts',(5.45319686416382,4.00686073637129,60.5047050546238));
#24069=CARTESIAN_POINT('Ctrl Pts',(5.35062109290156,4.14646276174468,60.5128283466414));
#24070=CARTESIAN_POINT('Ctrl Pts',(5.24264044877855,4.28217861910984,60.5209516386591));
#24071=CARTESIAN_POINT('Ctrl Pts',(5.12959067261962,4.41356868433853,60.5290749306768));
#24072=CARTESIAN_POINT('Ctrl Pts',(5.01655734279137,4.54493963511576,60.5371970409287));
#24073=CARTESIAN_POINT('Ctrl Pts',(4.898456588398,4.67198577034943,60.5453191511807));
#24074=CARTESIAN_POINT('Ctrl Pts',(4.77566411355636,4.79430091613886,60.5534412614327));
#24075=CARTESIAN_POINT('Ctrl Pts',(4.65251851601471,4.91696781194059,60.5615867289914));
#24076=CARTESIAN_POINT('Ctrl Pts',(4.52465442212268,5.03487619368594,60.5697321965501));
#24077=CARTESIAN_POINT('Ctrl Pts',(4.39248754888795,5.14765404168387,60.5778776641088));
#24078=CARTESIAN_POINT('Ctrl Pts',(4.26062336331425,5.26017360663259,60.586004476974));
#24079=CARTESIAN_POINT('Ctrl Pts',(4.12447638791394,5.36758590235807,60.5941312898391));
#24080=CARTESIAN_POINT('Ctrl Pts',(3.98449184794063,5.46956247918375,60.6022581027042));
#24081=CARTESIAN_POINT('Ctrl Pts',(3.84402531667306,5.57189017922817,60.6104128976098));
#24082=CARTESIAN_POINT('Ctrl Pts',(3.69969504955309,5.66874444752584,60.6185676925152));
#24083=CARTESIAN_POINT('Ctrl Pts',(3.55197900450941,5.75983803170926,60.6267224874208));
#24084=CARTESIAN_POINT('Ctrl Pts',(3.40426295946573,5.85093161589267,60.6348772823263));
#24085=CARTESIAN_POINT('Ctrl Pts',(3.25316147405337,5.93626436243895,60.6430320772318));
#24086=CARTESIAN_POINT('Ctrl Pts',(3.0991757505326,6.01559628526638,60.6511868721373));
#24087=CARTESIAN_POINT('Origin',(0.,0.,-3.69717978381041));
#24088=CARTESIAN_POINT('',(3.09917575053259,6.01559628526639,63.0459622914914));
#24089=CARTESIAN_POINT('',(3.09917575053255,6.01559628526641,62.6516502284592));
#24090=CARTESIAN_POINT('',(3.09917575053259,6.01559628526639,-3.69717978381041));
#24091=CARTESIAN_POINT('',(-6.76699995039181,-0.000819388301575002,61.6971797837649));
#24092=CARTESIAN_POINT('Ctrl Pts',(-6.7669999503917,-0.000819389256966134,
61.69717978381));
#24093=CARTESIAN_POINT('Ctrl Pts',(-6.76698654599217,-0.11152082960351,
61.7024122253477));
#24094=CARTESIAN_POINT('Ctrl Pts',(-6.76425673829185,-0.222188623443844,
61.7076446668854));
#24095=CARTESIAN_POINT('Ctrl Pts',(-6.75881518896444,-0.332725474563706,
61.712877108423));
#24096=CARTESIAN_POINT('Ctrl Pts',(-6.75026182071719,-0.506474224346479,
61.7211017879418));
#24097=CARTESIAN_POINT('Ctrl Pts',(-6.73499304333732,-0.68012191140438,
61.7293264674606));
#24098=CARTESIAN_POINT('Ctrl Pts',(-6.71300920765678,-0.853109827581033,
61.7375511469794));
#24099=CARTESIAN_POINT('Ctrl Pts',(-6.69104847947462,-1.02591591388727,
61.7457671814295));
#24100=CARTESIAN_POINT('Ctrl Pts',(-6.66238679335155,-1.19806325767366,
61.7539832158797));
#24101=CARTESIAN_POINT('Ctrl Pts',(-6.62707648148646,-1.36899463422218,
61.7621992503298));
#24102=CARTESIAN_POINT('Ctrl Pts',(-6.59179621203621,-1.53978058041187,
61.7704082944844));
#24103=CARTESIAN_POINT('Ctrl Pts',(-6.54987865498482,-1.70935227077692,
61.778617338639));
#24104=CARTESIAN_POINT('Ctrl Pts',(-6.50142777761176,-1.87715898434261,
61.7868263827936));
#24105=CARTESIAN_POINT('Ctrl Pts',(-6.45300842074125,-2.04485652853454,
61.7950300864217));
#24106=CARTESIAN_POINT('Ctrl Pts',(-6.3980643089523,-2.21079103998572,61.8032337900497));
#24107=CARTESIAN_POINT('Ctrl Pts',(-6.33675020530368,-2.37442326378086,
61.8114374936778));
#24108=CARTESIAN_POINT('Ctrl Pts',(-6.27546371518033,-2.53798179388603,
61.8196375026718));
#24109=CARTESIAN_POINT('Ctrl Pts',(-6.20781307413923,-2.69923976711647,
61.8278375116657));
#24110=CARTESIAN_POINT('Ctrl Pts',(-6.13400251700446,-2.85767425039716,
61.8360375206597));
#24111=CARTESIAN_POINT('Ctrl Pts',(-6.06019786191762,-3.01609606492218,
61.8442368739637));
#24112=CARTESIAN_POINT('Ctrl Pts',(-5.98023441516054,-3.17169451087125,
61.8524362272676));
#24113=CARTESIAN_POINT('Ctrl Pts',(-5.89436422029642,-3.32396742440256,
61.8606355805715));
#24114=CARTESIAN_POINT('Ctrl Pts',(-5.80849458528061,-3.47623934515944,
61.8688348804181));
#24115=CARTESIAN_POINT('Ctrl Pts',(-5.71671845402208,-3.62518546386789,
61.8770341802647));
#24116=CARTESIAN_POINT('Ctrl Pts',(-5.61933336673632,-3.77032909882994,
61.8852334801113));
#24117=CARTESIAN_POINT('Ctrl Pts',(-5.52193124776209,-3.91549811797806,
61.8934342139343));
#24118=CARTESIAN_POINT('Ctrl Pts',(-5.41891841813569,-4.05686303072718,
61.9016349477573));
#24119=CARTESIAN_POINT('Ctrl Pts',(-5.31063522389015,-4.19397693350563,
61.9098356815803));
#24120=CARTESIAN_POINT('Ctrl Pts',(-5.20231344813795,-4.33113969022664,
61.9180393373403));
#24121=CARTESIAN_POINT('Ctrl Pts',(-5.08871778906956,-4.46404813854992,
61.9262429931003));
#24122=CARTESIAN_POINT('Ctrl Pts',(-4.97022829260731,-4.59228915894523,
61.9344466488602));
#24123=CARTESIAN_POINT('Ctrl Pts',(-4.85160305880967,-4.72067708767348,
61.9426597024353));
#24124=CARTESIAN_POINT('Ctrl Pts',(-4.72807303084948,-4.84438664272941,
61.9508727560103));
#24125=CARTESIAN_POINT('Ctrl Pts',(-4.60005523419539,-4.96304149109713,
61.9590858095853));
#24126=CARTESIAN_POINT('Ctrl Pts',(-4.47196168653879,-5.08176655020079,
61.9673037230084));
#24127=CARTESIAN_POINT('Ctrl Pts',(-4.33937534849418,-5.19543070751279,
61.9755216364315));
#24128=CARTESIAN_POINT('Ctrl Pts',(-4.20274552019563,-5.30369862383559,
61.9837395498546));
#24129=CARTESIAN_POINT('Ctrl Pts',(-4.06590259545257,-5.4121354015872,61.9919702804505));
#24130=CARTESIAN_POINT('Ctrl Pts',(-3.92500386664062,-5.51515890747701,
62.0002010110466));
#24131=CARTESIAN_POINT('Ctrl Pts',(-3.78052786042997,-5.61247700186939,
62.0084317416425));
#24132=CARTESIAN_POINT('Ctrl Pts',(-3.6478439277254,-5.70185203254728,62.0159906833184));
#24133=CARTESIAN_POINT('Ctrl Pts',(-3.51214333222039,-5.78641540611171,
62.0235496249942));
#24134=CARTESIAN_POINT('Ctrl Pts',(-3.37381337021396,-5.86597582188723,
62.0311085666701));
#24135=CARTESIAN_POINT('Ctrl Pts',(-3.2245957095948,-5.95179829264999,62.0392624588368));
#24136=CARTESIAN_POINT('Ctrl Pts',(-3.07185677620594,-6.0320639703605,62.0474163510036));
#24137=CARTESIAN_POINT('Ctrl Pts',(-2.91605207173513,-6.10646618879768,
62.0555702431703));
#24138=CARTESIAN_POINT('Ctrl Pts',(-2.76043749253325,-6.18077761574151,
62.0637141853105));
#24139=CARTESIAN_POINT('Ctrl Pts',(-2.60176491531566,-6.24923966991835,
62.0718581274507));
#24140=CARTESIAN_POINT('Ctrl Pts',(-2.44051781454467,-6.31158948260184,
62.0800020695909));
#24141=CARTESIAN_POINT('Ctrl Pts',(-2.27943354098797,-6.37387633448626,
62.0881377879838));
#24142=CARTESIAN_POINT('Ctrl Pts',(-2.11578025795185,-6.43006310150856,
62.0962735063767));
#24143=CARTESIAN_POINT('Ctrl Pts',(-1.95006498203012,-6.47993329949159,
62.1044092247696));
#24144=CARTESIAN_POINT('Ctrl Pts',(-1.78448218703509,-6.52976362879016,
62.1125384390698));
#24145=CARTESIAN_POINT('Ctrl Pts',(-1.61684102990984,-6.57328733880246,
62.12066765337));
#24146=CARTESIAN_POINT('Ctrl Pts',(-1.4476673996933,-6.6103364589002,62.1287968676703));
#24147=CARTESIAN_POINT('Ctrl Pts',(-1.27859344432647,-6.64736375014983,
62.1369212923457));
#24148=CARTESIAN_POINT('Ctrl Pts',(-1.1079891702708,-6.67792397036248,62.1450457170211));
#24149=CARTESIAN_POINT('Ctrl Pts',(-0.936394478055206,-6.70189931149877,
62.1531701416965));
#24150=CARTESIAN_POINT('Ctrl Pts',(-0.763758096208908,-6.72602019830394,
62.1613438868307));
#24151=CARTESIAN_POINT('Ctrl Pts',(-0.590119591330146,-6.74347588739461,
62.1695176319649));
#24152=CARTESIAN_POINT('Ctrl Pts',(-0.416038587367723,-6.75419876031355,
62.1776913770991));
#24153=CARTESIAN_POINT('Ctrl Pts',(-0.243072347214923,-6.76485296709205,
62.1858127799612));
#24154=CARTESIAN_POINT('Ctrl Pts',(-0.0696696296329457,-6.76886033584515,
62.1939341828234));
#24155=CARTESIAN_POINT('Ctrl Pts',(0.103616438768401,-6.76620666500935,
62.2020555856855));
#24156=CARTESIAN_POINT('Ctrl Pts',(0.276915904736252,-6.76355278900569,
62.2101776164518));
#24157=CARTESIAN_POINT('Ctrl Pts',(0.450098337609681,-6.75423685314459,
62.218299647218));
#24158=CARTESIAN_POINT('Ctrl Pts',(0.622611803962377,-6.73829678342879,
62.2264216779843));
#24159=CARTESIAN_POINT('Ctrl Pts',(0.795171458695426,-6.72235244595338,
62.2345458833254));
#24160=CARTESIAN_POINT('Ctrl Pts',(0.967061425990442,-6.69978047686512,
62.2426700886665));
#24161=CARTESIAN_POINT('Ctrl Pts',(1.13773612147734,-6.67067054484673,62.2507942940076));
#24162=CARTESIAN_POINT('Ctrl Pts',(1.31025825244533,-6.64124551795671,62.2590064382501));
#24163=CARTESIAN_POINT('Ctrl Pts',(1.48153827060829,-6.60514022707172,62.2672185824925));
#24164=CARTESIAN_POINT('Ctrl Pts',(1.65102533557588,-6.56249985457421,62.2754307267349));
#24165=CARTESIAN_POINT('Ctrl Pts',(1.81896517043931,-6.52024874168182,62.2835679031514));
#24166=CARTESIAN_POINT('Ctrl Pts',(1.98514431810167,-6.47158153011745,62.2917050795678));
#24167=CARTESIAN_POINT('Ctrl Pts',(2.14904449102325,-6.41668892619883,62.2998422559843));
#24168=CARTESIAN_POINT('Ctrl Pts',(2.31520968297819,-6.36103773374152,62.3080918841397));
#24169=CARTESIAN_POINT('Ctrl Pts',(2.47903208332613,-6.29898796424722,62.3163415122951));
#24170=CARTESIAN_POINT('Ctrl Pts',(2.63999528366881,-6.2307875828186,62.3245911404505));
#24171=CARTESIAN_POINT('Ctrl Pts',(2.80095848401154,-6.16258720138996,62.332840768606));
#24172=CARTESIAN_POINT('Ctrl Pts',(2.95906216307362,-6.08823642901855,62.3410903967614));
#24173=CARTESIAN_POINT('Ctrl Pts',(3.11381873017303,-6.00802978651268,62.3493400249168));
#24174=CARTESIAN_POINT('Ctrl Pts',(3.2681108100888,-5.92806387665025,62.3575648925944));
#24175=CARTESIAN_POINT('Ctrl Pts',(3.41953711714995,-5.84203832537791,62.365789760272));
#24176=CARTESIAN_POINT('Ctrl Pts',(3.56758905171279,-5.75018237607287,62.3740146279496));
#24177=CARTESIAN_POINT('Ctrl Pts',(3.71547418919984,-5.65842991277619,62.3822302293931));
#24178=CARTESIAN_POINT('Ctrl Pts',(3.85999222207756,-5.56086031861584,62.3904458308366));
#24179=CARTESIAN_POINT('Ctrl Pts',(4.00065716874635,-5.45774964780892,62.3986614322802));
#24180=CARTESIAN_POINT('Ctrl Pts',(4.14119190301844,-5.35473442571108,62.4068694286083));
#24181=CARTESIAN_POINT('Ctrl Pts',(4.27788036684366,-5.24618855289939,62.4150774249364));
#24182=CARTESIAN_POINT('Ctrl Pts',(4.41026364162656,-5.13243252379872,62.4232854212646));
#24183=CARTESIAN_POINT('Ctrl Pts',(4.54255096015806,-5.0187589492388,62.431487468136));
#24184=CARTESIAN_POINT('Ctrl Pts',(4.67053903420414,-4.89988297336291,62.4396895150074));
#24185=CARTESIAN_POINT('Ctrl Pts',(4.79380019810623,-4.77616673291843,62.4478915618789));
#24186=CARTESIAN_POINT('Ctrl Pts',(4.91699676974234,-4.65251532321265,62.4560893106504));
#24187=CARTESIAN_POINT('Ctrl Pts',(5.03547111325602,-4.5240289554722,62.464287059422));
#24188=CARTESIAN_POINT('Ctrl Pts',(5.1488307097639,-4.39110821116859,62.4724848081936));
#24189=CARTESIAN_POINT('Ctrl Pts',(5.26216868520536,-4.25821281882749,62.4806809934092));
#24190=CARTESIAN_POINT('Ctrl Pts',(5.37039361948129,-4.12088500325434,62.4888771786248));
#24191=CARTESIAN_POINT('Ctrl Pts',(5.47315156208715,-3.97956040014761,62.4970733638405));
#24192=CARTESIAN_POINT('Ctrl Pts',(5.57590190289238,-3.838246251916,62.5052689427208));
#24193=CARTESIAN_POINT('Ctrl Pts',(5.67318584573008,-3.69293619468311,62.5134645216012));
#24194=CARTESIAN_POINT('Ctrl Pts',(5.76469131545445,-3.54409692834776,62.5216601004815));
#24195=CARTESIAN_POINT('Ctrl Pts',(5.85620666414728,-3.39524159326349,62.5298565641599));
#24196=CARTESIAN_POINT('Ctrl Pts',(5.94194210886517,-3.24285659572238,62.5380530278384));
#24197=CARTESIAN_POINT('Ctrl Pts',(6.02163027224256,-3.08743548344123,62.5462494915168));
#24198=CARTESIAN_POINT('Ctrl Pts',(6.10134153716534,-2.93196931468335,62.5544483313446));
#24199=CARTESIAN_POINT('Ctrl Pts',(6.175001865117,-2.77346559723053,62.5626471711724));
#24200=CARTESIAN_POINT('Ctrl Pts',(6.24239096363938,-2.61244024947431,62.5708460110002));
#24201=CARTESIAN_POINT('Ctrl Pts',(6.30985045199229,-2.45124670616144,62.5790534147494));
#24202=CARTESIAN_POINT('Ctrl Pts',(6.37102548520224,-2.28752660178286,62.5872608184986));
#24203=CARTESIAN_POINT('Ctrl Pts',(6.42574450346411,-2.12181445376377,62.5954682222479));
#24204=CARTESIAN_POINT('Ctrl Pts',(6.48049283212787,-1.95601354154876,62.6036800223169));
#24205=CARTESIAN_POINT('Ctrl Pts',(6.52877815272834,-1.78821880302378,62.6118918223859));
#24206=CARTESIAN_POINT('Ctrl Pts',(6.57047952295643,-1.61897740515742,62.6201036224549));
#24207=CARTESIAN_POINT('Ctrl Pts',(6.6122422834284,-1.44948686030543,62.6283275114411));
#24208=CARTESIAN_POINT('Ctrl Pts',(6.64740165105475,-1.27854575147428,62.6365514004272));
#24209=CARTESIAN_POINT('Ctrl Pts',(6.67588807835824,-1.10671015412091,62.6447752894134));
#24210=CARTESIAN_POINT('Ctrl Pts',(6.70220904471821,-0.947937032830664,
62.6523740206634));
#24211=CARTESIAN_POINT('Ctrl Pts',(6.72283357712056,-0.788400533362211,
62.6599727519134));
#24212=CARTESIAN_POINT('Ctrl Pts',(6.7377463720338,-0.628540234309178,62.6675714831635));
#24213=CARTESIAN_POINT('Ctrl Pts',(6.75388794517058,-0.455507833351089,
62.6757963314855));
#24214=CARTESIAN_POINT('Ctrl Pts',(6.76338240844148,-0.281610384600581,
62.6840211798076));
#24215=CARTESIAN_POINT('Ctrl Pts',(6.76614767100241,-0.107399693615434,
62.6922460281296));
#24216=CARTESIAN_POINT('Ctrl Pts',(6.76890981926458,0.066614797505694,62.7004616134488));
#24217=CARTESIAN_POINT('Ctrl Pts',(6.76495785204496,0.240941472929343,62.708677198768));
#24218=CARTESIAN_POINT('Ctrl Pts',(6.75426128694405,0.41502224963117,62.7168927840872));
#24219=CARTESIAN_POINT('Ctrl Pts',(6.7435746193942,0.588941949075024,62.7251007675104));
#24220=CARTESIAN_POINT('Ctrl Pts',(6.72615580448716,0.762615847088591,62.7333087509337));
#24221=CARTESIAN_POINT('Ctrl Pts',(6.70202637679818,0.935484604203326,62.7415167343569));
#24222=CARTESIAN_POINT('Ctrl Pts',(6.67791442959404,1.10822812711328,62.7497187715335));
#24223=CARTESIAN_POINT('Ctrl Pts',(6.64710160215835,1.28016731702472,62.75792080871));
#24224=CARTESIAN_POINT('Ctrl Pts',(6.6096613572644,1.45074661546589,62.7661228458865));
#24225=CARTESIAN_POINT('Ctrl Pts',(6.57224071749989,1.6212365921295,62.7743205881659));
#24226=CARTESIAN_POINT('Ctrl Pts',(6.52819965053682,1.7903677463213,62.7825183304454));
#24227=CARTESIAN_POINT('Ctrl Pts',(6.47766296223122,1.95759330498904,62.7907160727248));
#24228=CARTESIAN_POINT('Ctrl Pts',(6.42713588264062,2.12478706848404,62.7989122563391));
#24229=CARTESIAN_POINT('Ctrl Pts',(6.37011573945722,2.29007561325848,62.8071084399534));
#24230=CARTESIAN_POINT('Ctrl Pts',(6.30677767904757,2.45292566276831,62.8153046235678));
#24231=CARTESIAN_POINT('Ctrl Pts',(6.2434442812029,2.6157637242423,62.8235002038287));
#24232=CARTESIAN_POINT('Ctrl Pts',(6.17379402159843,2.77616331319956,62.8316957840896));
#24233=CARTESIAN_POINT('Ctrl Pts',(6.09805081799695,2.93360958907737,62.8398913643505));
#24234=CARTESIAN_POINT('Ctrl Pts',(6.02229940957214,3.09107292019998,62.8480878323912));
#24235=CARTESIAN_POINT('Ctrl Pts',(5.94045389779311,3.24558197745001,62.8562843004319));
#24236=CARTESIAN_POINT('Ctrl Pts',(5.85278495040703,3.39664501004873,62.8644807684726));
#24237=CARTESIAN_POINT('Ctrl Pts',(5.76509055595571,3.54775189067987,62.872679615646));
#24238=CARTESIAN_POINT('Ctrl Pts',(5.67156953904491,3.69541044400648,62.8808784628194));
#24239=CARTESIAN_POINT('Ctrl Pts',(5.57253684130363,3.83915643759326,62.8890773099928));
#24240=CARTESIAN_POINT('Ctrl Pts',(5.47340064476296,3.98305265972167,62.8972847257588));
#24241=CARTESIAN_POINT('Ctrl Pts',(5.36874146302995,4.12302785692412,62.9054921415247));
#24242=CARTESIAN_POINT('Ctrl Pts',(5.2589162295534,4.25864873998078,62.9136995572907));
#24243=CARTESIAN_POINT('Ctrl Pts',(5.14903213361444,4.39434231106074,62.9219113719429));
#24244=CARTESIAN_POINT('Ctrl Pts',(5.03397670244471,4.52567664593781,62.930123186595));
#24245=CARTESIAN_POINT('Ctrl Pts',(4.914144874771,4.6522542008968,62.9383350012471));
#24246=CARTESIAN_POINT('Ctrl Pts',(4.79413657651372,4.7790181605483,62.9465589090448));
#24247=CARTESIAN_POINT('Ctrl Pts',(4.66933808116413,4.90101108999017,62.9547828168424));
#24248=CARTESIAN_POINT('Ctrl Pts',(4.54017960588137,5.0178738671213,62.96300672464));
#24249=CARTESIAN_POINT('Ctrl Pts',(4.42083956005578,5.12585291493526,62.9706054635635));
#24250=CARTESIAN_POINT('Ctrl Pts',(4.29777775434849,5.22945244427701,62.978204202487));
#24251=CARTESIAN_POINT('Ctrl Pts',(4.17135572179625,5.32842194671534,62.9858029414105));
#24252=CARTESIAN_POINT('Ctrl Pts',(4.03572133038419,5.43460334532583,62.9939553995587));
#24253=CARTESIAN_POINT('Ctrl Pts',(3.89581693059393,5.53576935291031,63.0021078577069));
#24254=CARTESIAN_POINT('Ctrl Pts',(3.75205217390674,5.63155338110913,63.0102603158551));
#24255=CARTESIAN_POINT('Ctrl Pts',(3.60847848010543,5.72721011265146,63.0184019394134));
#24256=CARTESIAN_POINT('Ctrl Pts',(3.46105494864114,5.8174989092354,63.0265435629716));
#24257=CARTESIAN_POINT('Ctrl Pts',(3.31022470676398,5.90209296696768,63.0346851865299));
#24258=CARTESIAN_POINT('Ctrl Pts',(3.24058550614499,5.94115053582307,63.0384442215171));
#24259=CARTESIAN_POINT('Ctrl Pts',(3.17022055591669,5.97899470370963,63.0422032565043));
#24260=CARTESIAN_POINT('Ctrl Pts',(3.09917575053259,6.01559628526639,63.0459622914914));
#24261=CARTESIAN_POINT('Ctrl Pts',(3.09917575053255,6.01559628526641,61.0455262068868));
#24262=CARTESIAN_POINT('Ctrl Pts',(2.94555351499629,6.09474094267679,61.0536815348355));
#24263=CARTESIAN_POINT('Ctrl Pts',(2.78910094792113,6.16789239804414,61.0618368627841));
#24264=CARTESIAN_POINT('Ctrl Pts',(2.630338046527,6.23487054885605,61.0699921907328));
#24265=CARTESIAN_POINT('Ctrl Pts',(2.5886648585963,6.25245143860753,61.0721328577983));
#24266=CARTESIAN_POINT('Ctrl Pts',(2.54683256238906,6.26960726075716,61.0742735248638));
#24267=CARTESIAN_POINT('Ctrl Pts',(2.50485070333391,6.28633533579045,61.0764141919293));
#24268=CARTESIAN_POINT('Ctrl Pts',(2.34341266435111,6.35066187325475,61.0846459639602));
#24269=CARTESIAN_POINT('Ctrl Pts',(2.17925810486761,6.40886006779471,61.092877735991));
#24270=CARTESIAN_POINT('Ctrl Pts',(2.01289222894281,6.46069298718502,61.1011095080218));
#24271=CARTESIAN_POINT('Ctrl Pts',(1.84672501049944,6.51246401288971,61.1093314504943));
#24272=CARTESIAN_POINT('Ctrl Pts',(1.67835207224814,6.55788479280917,61.1175533929666));
#24273=CARTESIAN_POINT('Ctrl Pts',(1.50829947536923,6.59676600256527,61.125775335439));
#24274=CARTESIAN_POINT('Ctrl Pts',(1.33841586675202,6.63560857446361,61.1339891074289));
#24275=CARTESIAN_POINT('Ctrl Pts',(1.166856270493,6.66792443889963,61.1422028794189));
#24276=CARTESIAN_POINT('Ctrl Pts',(0.994162919560558,6.69357371583901,61.1504166514088));
#24277=CARTESIAN_POINT('Ctrl Pts',(0.821606593053894,6.71920264122793,61.1586239061391));
#24278=CARTESIAN_POINT('Ctrl Pts',(0.647918656475359,6.73817546252874,61.1668311608695));
#24279=CARTESIAN_POINT('Ctrl Pts',(0.473652670493714,6.75040311001752,61.1750384155998));
#24280=CARTESIAN_POINT('Ctrl Pts',(0.299490062808121,6.76262350380526,61.1832408016118));
#24281=CARTESIAN_POINT('Ctrl Pts',(0.124750445316112,6.76810666999312,61.1914431876238));
#24282=CARTESIAN_POINT('Ctrl Pts',(-0.0500062489708984,6.7668152313377,
61.1996455736357));
#24283=CARTESIAN_POINT('Ctrl Pts',(-0.224710782623472,6.76552417814539,
61.2078455114344));
#24284=CARTESIAN_POINT('Ctrl Pts',(-0.399432025036917,6.75746254672673,
61.2160454492332));
#24285=CARTESIAN_POINT('Ctrl Pts',(-0.573608529755235,6.74264504883596,
61.2242453870319));
#24286=CARTESIAN_POINT('Ctrl Pts',(-0.747760680102598,6.72782962281384,
61.2324441782676));
#24287=CARTESIAN_POINT('Ctrl Pts',(-0.921367887376428,6.70626024126302,
61.2406429695034));
#24288=CARTESIAN_POINT('Ctrl Pts',(-1.09387229603085,6.67800362383671,61.2488417607391));
#24289=CARTESIAN_POINT('Ctrl Pts',(-1.26638387731199,6.64974583151771,61.2570408928756));
#24290=CARTESIAN_POINT('Ctrl Pts',(-1.4377922148764,6.61480030724318,61.265240025012));
#24291=CARTESIAN_POINT('Ctrl Pts',(-1.60754807733957,6.57328518923695,61.2734391571484));
#24292=CARTESIAN_POINT('Ctrl Pts',(-1.77734179262776,6.53176081402761,61.2816401175593));
#24293=CARTESIAN_POINT('Ctrl Pts',(-1.94548195082092,6.48366401253082,61.2898410779702));
#24294=CARTESIAN_POINT('Ctrl Pts',(-2.11143289407961,6.42916325300568,61.2980420383812));
#24295=CARTESIAN_POINT('Ctrl Pts',(-2.27753937332141,6.37461141314893,61.3062506850662));
#24296=CARTESIAN_POINT('Ctrl Pts',(-2.44145219723324,6.3136437355179,61.3144593317513));
#24297=CARTESIAN_POINT('Ctrl Pts',(-2.602653275827,6.24647780159563,61.3226679784363));
#24298=CARTESIAN_POINT('Ctrl Pts',(-2.76393131634332,6.17927980077003,61.3308805441598));
#24299=CARTESIAN_POINT('Ctrl Pts',(-2.9224947051069,6.10587779396102,61.3390931098833));
#24300=CARTESIAN_POINT('Ctrl Pts',(-3.07784858531042,6.02653607687722,61.3473056756068));
#24301=CARTESIAN_POINT('Ctrl Pts',(-3.23341563345513,5.94708549150858,61.3555295101556));
#24302=CARTESIAN_POINT('Ctrl Pts',(-3.38576405884343,5.86167908273416,61.3637533447044));
#24303=CARTESIAN_POINT('Ctrl Pts',(-3.53442564233534,5.7706259954014,61.3719771792532));
#24304=CARTESIAN_POINT('Ctrl Pts',(-3.67101767300739,5.68696533603261,61.3795333362275));
#24305=CARTESIAN_POINT('Ctrl Pts',(-3.80449737468062,5.59853828613694,61.3870894932019));
#24306=CARTESIAN_POINT('Ctrl Pts',(-3.93452598659682,5.50561479408016,61.3946456501763));
#24307=CARTESIAN_POINT('Ctrl Pts',(-4.08330409181379,5.39929218650467,61.4032913682287));
#24308=CARTESIAN_POINT('Ctrl Pts',(-4.22790301321821,5.2868403360242,61.4119370862811));
#24309=CARTESIAN_POINT('Ctrl Pts',(-4.36781656082279,5.16860401762431,61.4205828043335));
#24310=CARTESIAN_POINT('Ctrl Pts',(-4.50755048794591,5.0505194905613,61.4292174230459));
#24311=CARTESIAN_POINT('Ctrl Pts',(-4.64261080379205,4.92666549947308,61.4378520417583));
#24312=CARTESIAN_POINT('Ctrl Pts',(-4.77252193589838,4.7974288292135,61.4464866604707));
#24313=CARTESIAN_POINT('Ctrl Pts',(-4.90702102452552,4.66362802180546,61.4554262203731));
#24314=CARTESIAN_POINT('Ctrl Pts',(-5.03600031520607,4.52405756887495,61.4643657802755));
#24315=CARTESIAN_POINT('Ctrl Pts',(-5.15896883919704,4.37919279276375,61.4733053401779));
#24316=CARTESIAN_POINT('Ctrl Pts',(-5.2774130730106,4.23965791947924,61.4819159934485));
#24317=CARTESIAN_POINT('Ctrl Pts',(-5.39028068970313,4.09521158941102,61.490526646719));
#24318=CARTESIAN_POINT('Ctrl Pts',(-5.49716951174906,3.94631680926615,61.4991372999895));
#24319=CARTESIAN_POINT('Ctrl Pts',(-5.60395715637359,3.79756296799242,61.5077398027006));
#24320=CARTESIAN_POINT('Ctrl Pts',(-5.70477711225701,3.64436931869997,61.5163423054117));
#24321=CARTESIAN_POINT('Ctrl Pts',(-5.79926748747544,3.48723179738748,61.5249448081228));
#24322=CARTESIAN_POINT('Ctrl Pts',(-5.89365151567872,3.33027113119192,61.5335376288903));
#24323=CARTESIAN_POINT('Ctrl Pts',(-5.98172001818,3.16937570896732,61.5421304496577));
#24324=CARTESIAN_POINT('Ctrl Pts',(-6.063154334882,3.00507046696107,61.5507232704252));
#24325=CARTESIAN_POINT('Ctrl Pts',(-6.07275173900028,2.98570634787531,61.5517359733834));
#24326=CARTESIAN_POINT('Ctrl Pts',(-6.08225704614675,2.96629489997478,61.5527486763416));
#24327=CARTESIAN_POINT('Ctrl Pts',(-6.09166977497695,2.94683700815506,61.5537613792998));
#24328=CARTESIAN_POINT('Ctrl Pts',(-6.16973431150839,2.78546283769022,61.5621602388123));
#24329=CARTESIAN_POINT('Ctrl Pts',(-6.24135027080265,2.62105142964491,61.5705590983248));
#24330=CARTESIAN_POINT('Ctrl Pts',(-6.3063014248226,2.4541498200559,61.5789579578373));
#24331=CARTESIAN_POINT('Ctrl Pts',(-6.37129295259934,2.28714446411944,61.5873620380963));
#24332=CARTESIAN_POINT('Ctrl Pts',(-6.42961129234394,2.11764613002741,61.5957661183554));
#24333=CARTESIAN_POINT('Ctrl Pts',(-6.48108965391801,1.94621835822112,61.6041701986144));
#24334=CARTESIAN_POINT('Ctrl Pts',(-6.53263955916306,1.77455233928095,61.6125859587081));
#24335=CARTESIAN_POINT('Ctrl Pts',(-6.57733039319003,1.60095184351121,61.6210017188018));
#24336=CARTESIAN_POINT('Ctrl Pts',(-6.61504586263275,1.42599342048459,61.6294174788956));
#24337=CARTESIAN_POINT('Ctrl Pts',(-6.65278947490392,1.2509044455927,61.637839518728));
#24338=CARTESIAN_POINT('Ctrl Pts',(-6.68354728082114,1.07445584971838,61.6462615585603));
#24339=CARTESIAN_POINT('Ctrl Pts',(-6.70725467162531,0.89723116862962,61.6546835983928));
#24340=CARTESIAN_POINT('Ctrl Pts',(-6.7309994247517,0.719727185373209,61.6631189111732));
#24341=CARTESIAN_POINT('Ctrl Pts',(-6.74767152196744,0.54144500394835,61.6715542239536));
#24342=CARTESIAN_POINT('Ctrl Pts',(-6.7572583650388,0.362971607860936,61.6799895367341));
#24343=CARTESIAN_POINT('Ctrl Pts',(-6.76377067841043,0.241735172136537,
61.6857196190777));
#24344=CARTESIAN_POINT('Ctrl Pts',(-6.76701462962386,0.120410512533247,
61.6914497014212));
#24345=CARTESIAN_POINT('Ctrl Pts',(-6.76699995039181,-0.000819388301668836,
61.6971797837648));
#24346=CARTESIAN_POINT('',(-6.76699930182051,-0.00307394872789667,61.3028202161439));
#24347=CARTESIAN_POINT('Ctrl Pts',(3.0991757505326,6.01559628526638,60.6511868721373));
#24348=CARTESIAN_POINT('Ctrl Pts',(2.94429628532114,6.0953886549795,60.6593889979253));
#24349=CARTESIAN_POINT('Ctrl Pts',(2.78649934526633,6.16911017648326,60.6675911237134));
#24350=CARTESIAN_POINT('Ctrl Pts',(2.62631334247578,6.2365669424078,60.6757932495014));
#24351=CARTESIAN_POINT('Ctrl Pts',(2.46612733968517,6.30402370833236,60.6839953752894));
#24352=CARTESIAN_POINT('Ctrl Pts',(2.30355264512538,6.36521564451638,60.6921975010774));
#24353=CARTESIAN_POINT('Ctrl Pts',(2.13913066466676,6.42000070089423,60.7003996268654));
#24354=CARTESIAN_POINT('Ctrl Pts',(1.9742258990232,6.47494662027531,60.7086258362024));
#24355=CARTESIAN_POINT('Ctrl Pts',(1.80697223583982,6.52361162574131,60.7168520455394));
#24356=CARTESIAN_POINT('Ctrl Pts',(1.63788877021495,6.56579084165828,60.7250782548764));
#24357=CARTESIAN_POINT('Ctrl Pts',(1.46899526262028,6.60792267103311,60.7332952224196));
#24358=CARTESIAN_POINT('Ctrl Pts',(1.29827639086296,6.64358313425741,60.7415121899627));
#24359=CARTESIAN_POINT('Ctrl Pts',(1.12626903778939,6.67261620764427,60.7497291575059));
#24360=CARTESIAN_POINT('Ctrl Pts',(0.954420404354541,6.70162249078736,60.7579385428493));
#24361=CARTESIAN_POINT('Ctrl Pts',(0.781286008843523,6.7240135038616,60.7661479281927));
#24362=CARTESIAN_POINT('Ctrl Pts',(0.60741572512062,6.73968360806917,60.7743573135361));
#24363=CARTESIAN_POINT('Ctrl Pts',(0.433670994096106,6.75534239680738,60.7825607708367));
#24364=CARTESIAN_POINT('Ctrl Pts',(0.259191789036619,6.76428991136996,60.7907642281373));
#24365=CARTESIAN_POINT('Ctrl Pts',(0.0845360497352806,6.76647195045506,
60.7989676854379));
#24366=CARTESIAN_POINT('Ctrl Pts',(-0.0900286051981397,6.76865285158929,
60.8071668645697));
#24367=CARTESIAN_POINT('Ctrl Pts',(-0.264769253210243,6.76407530167798,
60.8153660437016));
#24368=CARTESIAN_POINT('Ctrl Pts',(-0.439124893712001,6.75273709896383,
60.8235652228334));
#24369=CARTESIAN_POINT('Ctrl Pts',(-0.613447681853623,6.74140103261141,
60.8317628570632));
#24370=CARTESIAN_POINT('Ctrl Pts',(-0.787385249069672,6.72330686788164,
60.8399604912931));
#24371=CARTESIAN_POINT('Ctrl Pts',(-0.960378348078167,6.69850449194017,
60.8481581255229));
#24372=CARTESIAN_POINT('Ctrl Pts',(-1.13335896025528,6.67370390626137,60.8563551680385));
#24373=CARTESIAN_POINT('Ctrl Pts',(-1.30539488482131,6.642196123723,60.8645522105541));
#24374=CARTESIAN_POINT('Ctrl Pts',(-1.47593379243997,6.60408270998583,60.8727492530697));
#24375=CARTESIAN_POINT('Ctrl Pts',(-1.64649138553442,6.56596512026747,60.8809471937125));
#24376=CARTESIAN_POINT('Ctrl Pts',(-1.81555128478065,6.52124053565646,60.8891451343553));
#24377=CARTESIAN_POINT('Ctrl Pts',(-1.98257306739036,6.47006128506202,60.8973430749982));
#24378=CARTESIAN_POINT('Ctrl Pts',(-2.14964350615569,6.41886712512138,60.9055434038341));
#24379=CARTESIAN_POINT('Ctrl Pts',(-2.31467430277852,6.36121465882843,60.9137437326701));
#24380=CARTESIAN_POINT('Ctrl Pts',(-2.4771418132325,6.29730556961747,60.9219440615061));
#24381=CARTESIAN_POINT('Ctrl Pts',(-2.63977861904817,6.23332988547721,60.9301529352975));
#24382=CARTESIAN_POINT('Ctrl Pts',(-2.79984646819465,6.16308468478895,60.9383618090889));
#24383=CARTESIAN_POINT('Ctrl Pts',(-2.95684235178738,6.08681955594845,60.9465706828803));
#24384=CARTESIAN_POINT('Ctrl Pts',(-3.1139224933389,6.01051349645464,60.9547839622838));
#24385=CARTESIAN_POINT('Ctrl Pts',(-3.26792706660759,5.9281812369788,60.9629972416872));
#24386=CARTESIAN_POINT('Ctrl Pts',(-3.41837927031567,5.84011747863655,60.9712105210906));
#24387=CARTESIAN_POINT('Ctrl Pts',(-3.56905153401845,5.75192491320662,60.9794358137061));
#24388=CARTESIAN_POINT('Ctrl Pts',(-3.71616074221359,5.65798428862504,60.9876611063215));
#24389=CARTESIAN_POINT('Ctrl Pts',(-3.85925953728978,5.55863335936433,60.9958863989369));
#24390=CARTESIAN_POINT('Ctrl Pts',(-3.98867520777543,5.46878237832146,61.003325188049));
#24391=CARTESIAN_POINT('Ctrl Pts',(-4.11481101145358,5.37450694914118,61.0107639771612));
#24392=CARTESIAN_POINT('Ctrl Pts',(-4.23736099882772,5.27608384747758,61.0182027662733));
#24393=CARTESIAN_POINT('Ctrl Pts',(-4.37105208055609,5.16871304140562,61.0263178202561));
#24394=CARTESIAN_POINT('Ctrl Pts',(-4.50087193157398,5.05608682975706,61.0344328742391));
#24395=CARTESIAN_POINT('Ctrl Pts',(-4.62637357311772,4.93851764823799,61.042547928222));
#24396=CARTESIAN_POINT('Ctrl Pts',(-4.75173320454199,4.82108150094307,61.0506537996972));
#24397=CARTESIAN_POINT('Ctrl Pts',(-4.87278408495042,4.69871376635119,61.0587596711725));
#24398=CARTESIAN_POINT('Ctrl Pts',(-4.98911012961864,4.57176870746286,61.0668655426477));
#24399=CARTESIAN_POINT('Ctrl Pts',(-5.10532954422664,4.4449400125351,61.0749639838904));
#24400=CARTESIAN_POINT('Ctrl Pts',(-5.21683249680145,4.31354261643889,61.0830624251331));
#24401=CARTESIAN_POINT('Ctrl Pts',(-5.32323783316524,4.17796935981563,61.0911608663758));
#24402=CARTESIAN_POINT('Ctrl Pts',(-5.42956848042597,4.04249126613515,61.0992536230792));
#24403=CARTESIAN_POINT('Ctrl Pts',(-5.53080840856302,3.90284343752029,61.1073463797826));
#24404=CARTESIAN_POINT('Ctrl Pts',(-5.62661508061142,3.75945364842235,61.1154391364861));
#24405=CARTESIAN_POINT('Ctrl Pts',(-5.72238045895121,3.61612566186951,61.1235284051241));
#24406=CARTESIAN_POINT('Ctrl Pts',(-5.81271703735493,3.469059231583,61.1316176737622));
#24407=CARTESIAN_POINT('Ctrl Pts',(-5.89732414460166,3.31871314420187,61.1397069424002));
#24408=CARTESIAN_POINT('Ctrl Pts',(-5.98191328451942,3.16839898460672,61.1477944931855));
#24409=CARTESIAN_POINT('Ctrl Pts',(-6.06077519345288,3.01480687577612,61.1558820439708));
#24410=CARTESIAN_POINT('Ctrl Pts',(-6.13365395582839,2.85842231836913,61.1639695947561));
#24411=CARTESIAN_POINT('Ctrl Pts',(-6.20653140322502,2.70204058266743,61.1720569996147));
#24412=CARTESIAN_POINT('Ctrl Pts',(-6.27342576295178,2.5428668337222,61.1801444044733));
#24413=CARTESIAN_POINT('Ctrl Pts',(-6.33412833012273,2.38140867923519,61.1882318093319));
#24414=CARTESIAN_POINT('Ctrl Pts',(-6.39484159834729,2.21992206182728,61.1963206398921));
#24415=CARTESIAN_POINT('Ctrl Pts',(-6.44936077169434,2.05615058330686,61.2044094704524));
#24416=CARTESIAN_POINT('Ctrl Pts',(-6.49752632398515,1.89061912322921,61.2124983010127));
#24417=CARTESIAN_POINT('Ctrl Pts',(-6.54573346668213,1.72494472861995,61.2205941161861));
#24418=CARTESIAN_POINT('Ctrl Pts',(-6.58757592708849,1.55750767229182,61.2286899313595));
#24419=CARTESIAN_POINT('Ctrl Pts',(-6.62294466919305,1.38884589094952,61.2367857465329));
#24420=CARTESIAN_POINT('Ctrl Pts',(-6.65832968734877,1.22010649452627,61.244885287253));
#24421=CARTESIAN_POINT('Ctrl Pts',(-6.68723498928914,1.05014161398107,61.2529848279732));
#24422=CARTESIAN_POINT('Ctrl Pts',(-6.70960323088031,0.879496153579135,
61.2610843686933));
#24423=CARTESIAN_POINT('Ctrl Pts',(-6.73200003672778,0.708632778834374,
61.2691942525312));
#24424=CARTESIAN_POINT('Ctrl Pts',(-6.74784307313428,0.537087455670259,
61.2773041363692));
#24425=CARTESIAN_POINT('Ctrl Pts',(-6.75712705912241,0.365407863729989,
61.2854140202071));
#24426=CARTESIAN_POINT('Ctrl Pts',(-6.76376911394562,0.242582897907103,
61.2912160855193));
#24427=CARTESIAN_POINT('Ctrl Pts',(-6.76705506770958,0.11968923497642,61.2970181508316));
#24428=CARTESIAN_POINT('Ctrl Pts',(-6.76699930182051,-0.00307394872799501,
61.3028202161439));
#24429=CARTESIAN_POINT('Ctrl Pts',(-6.76699930182007,-0.00307394969982656,
61.3028202161898));
#24430=CARTESIAN_POINT('Ctrl Pts',(-6.7668929816298,-0.237127439049988,
61.3138821126868));
#24431=CARTESIAN_POINT('Ctrl Pts',(-6.75464487673108,-0.470843644988345,
61.3249440091838));
#24432=CARTESIAN_POINT('Ctrl Pts',(-6.73035212995149,-0.703313021959266,
61.3360059056808));
#24433=CARTESIAN_POINT('Ctrl Pts',(-6.71244851064451,-0.874641660238803,
61.344158461894));
#24434=CARTESIAN_POINT('Ctrl Pts',(-6.68797057376292,-1.04555419704913,
61.3523110181073));
#24435=CARTESIAN_POINT('Ctrl Pts',(-6.65693963625638,-1.21550141062804,
61.3604635743205));
#24436=CARTESIAN_POINT('Ctrl Pts',(-6.62594464883903,-1.385251736263,61.3686066856009));
#24437=CARTESIAN_POINT('Ctrl Pts',(-6.58841183801031,-1.55403860890881,
61.3767497968813));
#24438=CARTESIAN_POINT('Ctrl Pts',(-6.54441439465594,-1.7213161333759,61.3848929081616));
#24439=CARTESIAN_POINT('Ctrl Pts',(-6.50045867348595,-1.88843503081411,
61.3930282974389));
#24440=CARTESIAN_POINT('Ctrl Pts',(-6.45005061682981,-2.05404707849207,
61.4011636867163));
#24441=CARTESIAN_POINT('Ctrl Pts',(-6.39331475531231,-2.21761480864147,
61.4092990759936));
#24442=CARTESIAN_POINT('Ctrl Pts',(-6.33662077407636,-2.3810617992373,61.4174284600322));
#24443=CARTESIAN_POINT('Ctrl Pts',(-6.27360840794948,-2.54246713314629,
61.4255578440708));
#24444=CARTESIAN_POINT('Ctrl Pts',(-6.20445248283445,-2.70130679269302,
61.4336872281094));
#24445=CARTESIAN_POINT('Ctrl Pts',(-6.13533307997369,-2.86006256669525,
61.4418123189015));
#24446=CARTESIAN_POINT('Ctrl Pts',(-6.06007672529144,-3.01625503039086,
61.4499374096936));
#24447=CARTESIAN_POINT('Ctrl Pts',(-5.97890699582596,-3.16937850930801,
61.4580625004858));
#24448=CARTESIAN_POINT('Ctrl Pts',(-5.89742742390638,-3.3230864937397,61.4662186065109));
#24449=CARTESIAN_POINT('Ctrl Pts',(-5.8099893722018,-3.47370166810867,61.474374712536));
#24450=CARTESIAN_POINT('Ctrl Pts',(-5.71686660431286,-3.62073545408835,
61.4825308185611));
#24451=CARTESIAN_POINT('Ctrl Pts',(-5.6241186387233,-3.7671774556707,61.4906540977345));
#24452=CARTESIAN_POINT('Ctrl Pts',(-5.52573184718002,-3.91006654457672,
61.4987773769079));
#24453=CARTESIAN_POINT('Ctrl Pts',(-5.42202113510328,-4.04894749416356,
61.5069006560813));
#24454=CARTESIAN_POINT('Ctrl Pts',(-5.31829661306878,-4.18784693692251,
61.515025016938));
#24455=CARTESIAN_POINT('Ctrl Pts',(-5.20924697736297,-4.32273688415053,
61.5231493777947));
#24456=CARTESIAN_POINT('Ctrl Pts',(-5.09522848922095,-4.45319386986814,
61.5312737386514));
#24457=CARTESIAN_POINT('Ctrl Pts',(-4.98117312594974,-4.58369304714854,
61.5394007270368));
#24458=CARTESIAN_POINT('Ctrl Pts',(-4.86214595082338,-4.70975613270178,
61.5475277154222));
#24459=CARTESIAN_POINT('Ctrl Pts',(-4.73854122315886,-4.83099535048671,
61.5556547038076));
#24460=CARTESIAN_POINT('Ctrl Pts',(-4.61413740500253,-4.95301836601139,
61.5638342322477));
#24461=CARTESIAN_POINT('Ctrl Pts',(-4.48509691070055,-5.07015466284871,
61.5720137606878));
#24462=CARTESIAN_POINT('Ctrl Pts',(-4.35185604424471,-5.18204959163561,
61.5801932891279));
#24463=CARTESIAN_POINT('Ctrl Pts',(-4.21924265198395,-5.29341757112954,
61.5883342975316));
#24464=CARTESIAN_POINT('Ctrl Pts',(-4.08246869228262,-5.39959326967789,
61.5964753059353));
#24465=CARTESIAN_POINT('Ctrl Pts',(-3.94199372397726,-5.50027040063704,
61.6046163143389));
#24466=CARTESIAN_POINT('Ctrl Pts',(-3.80052174757006,-5.60166207822643,
61.6128151027972));
#24467=CARTESIAN_POINT('Ctrl Pts',(-3.65529634943674,-5.6974766422748,61.6210138912555));
#24468=CARTESIAN_POINT('Ctrl Pts',(-3.50681205355254,-5.7874483342021,61.6292126797137));
#24469=CARTESIAN_POINT('Ctrl Pts',(-3.35832775766833,-5.8774200261294,61.637411468172));
#24470=CARTESIAN_POINT('Ctrl Pts',(-3.20658492023533,-5.96154872252506,
61.6456102566303));
#24471=CARTESIAN_POINT('Ctrl Pts',(-3.05209803754034,-6.03961808140568,
61.6538090450885));
#24472=CARTESIAN_POINT('Ctrl Pts',(-2.89696557419642,-6.11801368201303,
61.6620420952205));
#24473=CARTESIAN_POINT('Ctrl Pts',(-2.73858390273423,-6.19054299955712,
61.6702751453525));
#24474=CARTESIAN_POINT('Ctrl Pts',(-2.57743551803947,-6.2569253751622,61.6785081954846));
#24475=CARTESIAN_POINT('Ctrl Pts',(-2.41647903629973,-6.32322869956199,
61.6867314413194));
#24476=CARTESIAN_POINT('Ctrl Pts',(-2.25276272988472,-6.38339952299103,
61.6949546871543));
#24477=CARTESIAN_POINT('Ctrl Pts',(-2.08679406518591,-6.43720277212897,
61.7031779329891));
#24478=CARTESIAN_POINT('Ctrl Pts',(-1.92098982466843,-6.49095271870399,
61.7113930321026));
#24479=CARTESIAN_POINT('Ctrl Pts',(-1.75293800810747,-6.53834754438559,
61.7196081312162));
#24480=CARTESIAN_POINT('Ctrl Pts',(-1.5831665497045,-6.57920000272805,61.7278232303297));
#24481=CARTESIAN_POINT('Ctrl Pts',(-1.41352931503992,-6.6200201625338,61.7360318344686));
#24482=CARTESIAN_POINT('Ctrl Pts',(-1.24217549320595,-6.65430817414218,
61.7442404386074));
#24483=CARTESIAN_POINT('Ctrl Pts',(-1.06964878308494,-6.68192640492582,
61.7524490427463));
#24484=CARTESIAN_POINT('Ctrl Pts',(-0.897223964891428,-6.70952832475816,
61.7606527989953));
#24485=CARTESIAN_POINT('Ctrl Pts',(-0.72362799107796,-6.73046825448673,
61.7688565552442));
#24486=CARTESIAN_POINT('Ctrl Pts',(-0.549415468721582,-6.74465949049538,
61.7770603114932));
#24487=CARTESIAN_POINT('Ctrl Pts',(-0.375254491459373,-6.758846527675,61.7852616404575));
#24488=CARTESIAN_POINT('Ctrl Pts',(-0.200477685263298,-6.7662888157333,
61.7934629694218));
#24489=CARTESIAN_POINT('Ctrl Pts',(-0.0256457625954296,-6.76695140331752,
61.801664298386));
#24490=CARTESIAN_POINT('Ctrl Pts',(0.149162049081187,-6.76761389952458,
61.8098644963088));
#24491=CARTESIAN_POINT('Ctrl Pts',(0.324024603937487,-6.76149855526386,
61.8180646942315));
#24492=CARTESIAN_POINT('Ctrl Pts',(0.498380174682741,-6.74862254104371,
61.8262648921542));
#24493=CARTESIAN_POINT('Ctrl Pts',(0.67274329690716,-6.73574596915308,61.8344654452341));
#24494=CARTESIAN_POINT('Ctrl Pts',(0.846599033939123,-6.71610817028283,
61.8426659983139));
#24495=CARTESIAN_POINT('Ctrl Pts',(1.01938970737883,-6.68977829412082,61.8508665513937));
#24496=CARTESIAN_POINT('Ctrl Pts',(1.19221917757542,-6.66344250610151,61.8590689457469));
#24497=CARTESIAN_POINT('Ctrl Pts',(1.36398275375906,-6.63041170204703,61.8672713401002));
#24498=CARTESIAN_POINT('Ctrl Pts',(1.53413183069558,-6.59080636387132,61.8754737344534));
#24499=CARTESIAN_POINT('Ctrl Pts',(1.70444002692969,-6.55116398774215,61.8836837994872));
#24500=CARTESIAN_POINT('Ctrl Pts',(1.87313035797372,-6.50493487494192,61.891893864521));
#24501=CARTESIAN_POINT('Ctrl Pts',(2.03966738128879,-6.45228997904671,61.9001039295549));
#24502=CARTESIAN_POINT('Ctrl Pts',(2.20628410626878,-6.39961988823825,61.9083179237802));
#24503=CARTESIAN_POINT('Ctrl Pts',(2.37074513180857,-6.3405280133835,61.9165319180055));
#24504=CARTESIAN_POINT('Ctrl Pts',(2.53253402601486,-6.27523389261922,61.9247459122308));
#24505=CARTESIAN_POINT('Ctrl Pts',(2.69454349236949,-6.20985075422143,61.932971104866));
#24506=CARTESIAN_POINT('Ctrl Pts',(2.85387321990489,-6.13824861793555,61.9411962975012));
#24507=CARTESIAN_POINT('Ctrl Pts',(3.0100293556326,-6.06069404261839,61.9494214901364));
#24508=CARTESIAN_POINT('Ctrl Pts',(3.15046023403321,-5.99094937914409,61.9568183882563));
#24509=CARTESIAN_POINT('Ctrl Pts',(3.28832468724447,-5.91639146587919,61.9642152863762));
#24510=CARTESIAN_POINT('Ctrl Pts',(3.42328362396414,-5.83724406119009,61.9716121844961));
#24511=CARTESIAN_POINT('Ctrl Pts',(3.58103224042604,-5.74473152449021,61.980258150987));
#24512=CARTESIAN_POINT('Ctrl Pts',(3.73516901794116,-5.64573824605703,61.9889041174779));
#24513=CARTESIAN_POINT('Ctrl Pts',(3.88515882616753,-5.54056223640278,61.9975500839688));
#24514=CARTESIAN_POINT('Ctrl Pts',(4.03495677703869,-5.43552076116312,62.0061849910931));
#24515=CARTESIAN_POINT('Ctrl Pts',(4.18061808769504,-5.32431249906942,62.0148198982175));
#24516=CARTESIAN_POINT('Ctrl Pts',(4.3216343565494,-5.20728004703913,62.0234548053419));
#24517=CARTESIAN_POINT('Ctrl Pts',(4.46733225171322,-5.08636221206021,62.0323763844134));
#24518=CARTESIAN_POINT('Ctrl Pts',(4.60807109022155,-4.95922696164353,62.0412979634849));
#24519=CARTESIAN_POINT('Ctrl Pts',(4.74332241674989,-4.82630101120496,62.0502195425565));
#24520=CARTESIAN_POINT('Ctrl Pts',(4.87386625208897,-4.69800161605849,62.0588306015322));
#24521=CARTESIAN_POINT('Ctrl Pts',(4.99929785419993,-4.56430803677536,62.0674416605079));
#24522=CARTESIAN_POINT('Ctrl Pts',(5.11917500867218,-4.42564528973869,62.0760527194836));
#24523=CARTESIAN_POINT('Ctrl Pts',(5.23893911345366,-4.2871133080738,62.0846556578331));
#24524=CARTESIAN_POINT('Ctrl Pts',(5.35315901520982,-4.14362173155766,62.0932585961827));
#24525=CARTESIAN_POINT('Ctrl Pts',(5.46142966450565,-3.99563199252104,62.1018615345322));
#24526=CARTESIAN_POINT('Ctrl Pts',(5.56957907572101,-3.84780796775702,62.110454839581));
#24527=CARTESIAN_POINT('Ctrl Pts',(5.67179234487287,-3.69549607454804,62.1190481446298));
#24528=CARTESIAN_POINT('Ctrl Pts',(5.76770487186885,-3.5391905163498,62.1276414496785));
#24529=CARTESIAN_POINT('Ctrl Pts',(5.77839109730472,-3.52177551870455,62.1285988845191));
#24530=CARTESIAN_POINT('Ctrl Pts',(5.78899914961594,-3.50431097827565,62.1295563193596));
#24531=CARTESIAN_POINT('Ctrl Pts',(5.79952855630722,-3.48679760304167,62.1305137542002));
#24532=CARTESIAN_POINT('Ctrl Pts',(5.89406055285213,-3.32956421129886,62.1391095117478));
#24533=CARTESIAN_POINT('Ctrl Pts',(5.9821391368501,-3.16857652712314,62.1477052692953));
#24534=CARTESIAN_POINT('Ctrl Pts',(6.06349327923072,-3.00438650188751,62.1563010268429));
#24535=CARTESIAN_POINT('Ctrl Pts',(6.14492332779223,-2.84004328177587,62.1649048045245));
#24536=CARTESIAN_POINT('Ctrl Pts',(6.21961627579129,-2.67249203022544,62.1735085822061));
#24537=CARTESIAN_POINT('Ctrl Pts',(6.28734900686327,-2.5023052303617,62.1821123598877));
#24538=CARTESIAN_POINT('Ctrl Pts',(6.3577436934947,-2.32542994044489,62.1910542735557));
#24539=CARTESIAN_POINT('Ctrl Pts',(6.42061988745001,-2.14570810900155,62.1999961872238));
#24540=CARTESIAN_POINT('Ctrl Pts',(6.47578430699948,-1.96379902465076,62.2089381008918));
#24541=CARTESIAN_POINT('Ctrl Pts',(6.52900721057239,-1.78829224447416,62.2175653032225));
#24542=CARTESIAN_POINT('Ctrl Pts',(6.57505189391687,-1.61074984784267,62.2261925055532));
#24543=CARTESIAN_POINT('Ctrl Pts',(6.61379707200392,-1.43177417575271,62.2348197078839));
#24544=CARTESIAN_POINT('Ctrl Pts',(6.65257914894263,-1.25262805672969,62.2434551263043));
#24545=CARTESIAN_POINT('Ctrl Pts',(6.68404778913837,-1.07204623735428,62.2520905447247));
#24546=CARTESIAN_POINT('Ctrl Pts',(6.70813331464309,-0.890638216660103,
62.2607259631452));
#24547=CARTESIAN_POINT('Ctrl Pts',(6.73225442308106,-0.708962191454703,
62.2693741391663));
#24548=CARTESIAN_POINT('Ctrl Pts',(6.7489705878499,-0.52645782899367,62.2780223151874));
#24549=CARTESIAN_POINT('Ctrl Pts',(6.75826405733234,-0.343738172698098,
62.2866704912086));
#24550=CARTESIAN_POINT('Ctrl Pts',(6.75924727116554,-0.324407125879982,
62.2875854354403));
#24551=CARTESIAN_POINT('Ctrl Pts',(6.76014745201357,-0.305073667561077,
62.2885003796721));
#24552=CARTESIAN_POINT('Ctrl Pts',(6.76096461291053,-0.285738522029537,
62.2894153239038));
#24553=CARTESIAN_POINT('Ctrl Pts',(6.76831146445643,-0.111901956468381,
62.2976413164452));
#24554=CARTESIAN_POINT('Ctrl Pts',(6.76895917775932,0.0624463016276273,
62.3058673089865));
#24555=CARTESIAN_POINT('Ctrl Pts',(6.76285728096748,0.236749651034807,62.3140933015278));
#24556=CARTESIAN_POINT('Ctrl Pts',(6.75676178122574,0.410870265909723,62.3223106701793));
#24557=CARTESIAN_POINT('Ctrl Pts',(6.74393077494341,0.584945710722264,62.3305280388307));
#24558=CARTESIAN_POINT('Ctrl Pts',(6.72436569210212,0.758416138330427,62.3387454074821));
#24559=CARTESIAN_POINT('Ctrl Pts',(6.70481720583301,0.931739415298017,62.3469558055445));
#24560=CARTESIAN_POINT('Ctrl Pts',(6.67854605984623,1.10445834317808,62.3551662036068));
#24561=CARTESIAN_POINT('Ctrl Pts',(6.64560569714577,1.27601485808894,62.3633766016692));
#24562=CARTESIAN_POINT('Ctrl Pts',(6.61268668756626,1.4474601639325,62.371581677458));
#24563=CARTESIAN_POINT('Ctrl Pts',(6.57310714014275,1.61774420715714,62.3797867532467));
#24564=CARTESIAN_POINT('Ctrl Pts',(6.5269721262206,1.78631572336455,62.3879918290355));
#24565=CARTESIAN_POINT('Ctrl Pts',(6.48085779172285,1.95481167956599,62.396193227005));
#24566=CARTESIAN_POINT('Ctrl Pts',(6.42819393926824,2.12159629321306,62.4043946249745));
#24567=CARTESIAN_POINT('Ctrl Pts',(6.36913639184669,2.28613005361773,62.412596022944));
#24568=CARTESIAN_POINT('Ctrl Pts',(6.31008347030392,2.45065092636847,62.4207967785117));
#24569=CARTESIAN_POINT('Ctrl Pts',(6.24463796408132,2.61292095715668,62.4289975340794));
#24570=CARTESIAN_POINT('Ctrl Pts',(6.17300519655273,2.77241696779778,62.4371982896471));
#24571=CARTESIAN_POINT('Ctrl Pts',(6.10137279288451,2.93191216827505,62.4453990035588));
#24572=CARTESIAN_POINT('Ctrl Pts',(6.0235533363634,3.08863304931904,62.4535997174706));
#24573=CARTESIAN_POINT('Ctrl Pts',(5.93979977772341,3.24207766726169,62.4618004313824));
#24574=CARTESIAN_POINT('Ctrl Pts',(5.85603146628133,3.39554931376427,62.470002589812));
#24575=CARTESIAN_POINT('Ctrl Pts',(5.76632714190889,3.54574323282565,62.4782047482416));
#24576=CARTESIAN_POINT('Ctrl Pts',(5.67098509493223,3.69218323665774,62.4864069066712));
#24577=CARTESIAN_POINT('Ctrl Pts',(5.57560897535943,3.83867557407474,62.4946119963241));
#24578=CARTESIAN_POINT('Ctrl Pts',(5.47459131506278,3.98141102368854,62.5028170859771));
#24579=CARTESIAN_POINT('Ctrl Pts',(5.3682730167594,4.11994342406943,62.51102217563));
#24580=CARTESIAN_POINT('Ctrl Pts',(5.2618332623702,4.2586340813391,62.5192366386278));
#24581=CARTESIAN_POINT('Ctrl Pts',(5.150080990854,4.39311181226388,62.5274511016256));
#24582=CARTESIAN_POINT('Ctrl Pts',(5.03339727842801,4.52296372277222,62.5356655646233));
#24583=CARTESIAN_POINT('Ctrl Pts',(4.91664443459033,4.6528925664334,62.5438848944308));
#24584=CARTESIAN_POINT('Ctrl Pts',(4.79495457498674,4.77818986985511,62.5521042242383));
#24585=CARTESIAN_POINT('Ctrl Pts',(4.66874465285244,4.8984806181572,62.5603235540458));
#24586=CARTESIAN_POINT('Ctrl Pts',(4.5423391760957,5.01895774968075,62.5685556192064));
#24587=CARTESIAN_POINT('Ctrl Pts',(4.41139990957234,5.13441258701736,62.5767876843671));
#24588=CARTESIAN_POINT('Ctrl Pts',(4.27637683634421,5.24451047797397,62.5850197495278));
#24589=CARTESIAN_POINT('Ctrl Pts',(4.15500840293664,5.34347436782933,62.592419320789));
#24590=CARTESIAN_POINT('Ctrl Pts',(4.03034093818189,5.43811046666926,62.5998188920503));
#24591=CARTESIAN_POINT('Ctrl Pts',(3.90271960484759,5.52820664283982,62.6072184633115));
#24592=CARTESIAN_POINT('Ctrl Pts',(3.76207289121807,5.62749827973083,62.6153732549358));
#24593=CARTESIAN_POINT('Ctrl Pts',(3.6174051020321,5.72158092630715,62.6235280465601));
#24594=CARTESIAN_POINT('Ctrl Pts',(3.46914159230921,5.81010719458001,62.6316828381844));
#24595=CARTESIAN_POINT('Ctrl Pts',(3.34813153676848,5.88236076972154,62.6383386349427));
#24596=CARTESIAN_POINT('Ctrl Pts',(3.22472693851301,5.95091355411429,62.644994431701));
#24597=CARTESIAN_POINT('Ctrl Pts',(3.09917575053255,6.01559628526641,62.6516502284592));
#24598=CARTESIAN_POINT('Origin',(0.,0.,-3.69717978381041));
#24599=CARTESIAN_POINT('',(3.09917575053256,6.01559628526641,65.0457972463573));
#24600=CARTESIAN_POINT('',(3.09917575053261,6.01559628526638,64.6514343427993));
#24601=CARTESIAN_POINT('',(3.09917575053259,6.01559628526639,-3.69717978381041));
#24602=CARTESIAN_POINT('',(-6.76699856902015,0.00440078166664134,63.6971797838431));
#24603=CARTESIAN_POINT('Ctrl Pts',(-6.76699856902015,0.00440078166665036,
63.6971797838431));
#24604=CARTESIAN_POINT('Ctrl Pts',(-6.767108590525,-0.164777201310378,63.7051406601575));
#24605=CARTESIAN_POINT('Ctrl Pts',(-6.76087012901741,-0.334158426395189,
63.713101536472));
#24606=CARTESIAN_POINT('Ctrl Pts',(-6.74826403482701,-0.503211204426377,
63.7210624127865));
#24607=CARTESIAN_POINT('Ctrl Pts',(-6.73566544902183,-0.672163292001071,
63.7290185474795));
#24608=CARTESIAN_POINT('Ctrl Pts',(-6.71670680146507,-0.840786942478803,
63.7369746821726));
#24609=CARTESIAN_POINT('Ctrl Pts',(-6.69142101104761,-1.00855037202442,
63.7449308168656));
#24610=CARTESIAN_POINT('Ctrl Pts',(-6.66614483777729,-1.17624999476154,
63.7528839255383));
#24611=CARTESIAN_POINT('Ctrl Pts',(-6.63454636505756,-1.34308967047614,
63.7608370342109));
#24612=CARTESIAN_POINT('Ctrl Pts',(-6.59671034256163,-1.50854289178017,
63.7687901428835));
#24613=CARTESIAN_POINT('Ctrl Pts',(-6.57674288147224,-1.59585864382195,
63.7729872909315));
#24614=CARTESIAN_POINT('Ctrl Pts',(-6.55503909123649,-1.68278837295603,
63.7771844389794));
#24615=CARTESIAN_POINT('Ctrl Pts',(-6.53161718373125,-1.7692557659046,63.7813815870274));
#24616=CARTESIAN_POINT('Ctrl Pts',(-6.48365191542533,-1.94633065622099,
63.7899768447874));
#24617=CARTESIAN_POINT('Ctrl Pts',(-6.42850987667823,-2.12134953563729,
63.7985721025475));
#24618=CARTESIAN_POINT('Ctrl Pts',(-6.3664016514861,-2.29373473007561,63.8071673603075));
#24619=CARTESIAN_POINT('Ctrl Pts',(-6.30423526457459,-2.46628135593908,
63.815770667162));
#24620=CARTESIAN_POINT('Ctrl Pts',(-6.23508977348513,-2.63618908665449,
63.8243739740165));
#24621=CARTESIAN_POINT('Ctrl Pts',(-6.15922374956039,-2.80290060523939,
63.8329772808709));
#24622=CARTESIAN_POINT('Ctrl Pts',(-6.08021229397599,-2.97652404119465,
63.8419372838109));
#24623=CARTESIAN_POINT('Ctrl Pts',(-5.99391132970834,-3.14668024408994,
63.8508972867509));
#24624=CARTESIAN_POINT('Ctrl Pts',(-5.90066489955293,-3.3127696483734,63.8598572896909));
#24625=CARTESIAN_POINT('Ctrl Pts',(-5.81088565084752,-3.47268335133925,
63.8684841328956));
#24626=CARTESIAN_POINT('Ctrl Pts',(-5.71466832376391,-3.62882700613723,
63.8771109761004));
#24627=CARTESIAN_POINT('Ctrl Pts',(-5.61236363058181,-3.78069616315865,
63.8857378193051));
#24628=CARTESIAN_POINT('Ctrl Pts',(-5.50996115997395,-3.9327104687042,63.8943729075912));
#24629=CARTESIAN_POINT('Ctrl Pts',(-5.40145988802639,-4.0804418742919,63.9030079958773));
#24630=CARTESIAN_POINT('Ctrl Pts',(-5.28725141460612,-4.22341822209755,
63.9116430841634));
#24631=CARTESIAN_POINT('Ctrl Pts',(-5.17287331868323,-4.36660691847247,
63.9202909972886));
#24632=CARTESIAN_POINT('Ctrl Pts',(-5.05277127917993,-4.50502621113751,
63.9289389104137));
#24633=CARTESIAN_POINT('Ctrl Pts',(-4.92737540137381,-4.63823896041766,
63.9375868235388));
#24634=CARTESIAN_POINT('Ctrl Pts',(-4.91330789280599,-4.65318340296735,
63.9385569877428));
#24635=CARTESIAN_POINT('Ctrl Pts',(-4.89917379495111,-4.66806235925509,
63.9395271519469));
#24636=CARTESIAN_POINT('Ctrl Pts',(-4.8849737418991,-4.68287524294171,63.9404973161509));
#24637=CARTESIAN_POINT('Ctrl Pts',(-4.76459114582249,-4.80845318177368,
63.9487219956697));
#24638=CARTESIAN_POINT('Ctrl Pts',(-4.63920445119171,-4.92955161938866,
63.9569466751885));
#24639=CARTESIAN_POINT('Ctrl Pts',(-4.50918025965089,-5.0457489420278,63.9651713547073));
#24640=CARTESIAN_POINT('Ctrl Pts',(-4.37929273824527,-5.16182412813523,
63.9733873891574));
#24641=CARTESIAN_POINT('Ctrl Pts',(-4.24477769190263,-5.27300822111426,
63.9816034236076));
#24642=CARTESIAN_POINT('Ctrl Pts',(-4.10603999731073,-5.37891481067367,
63.9898194580577));
#24643=CARTESIAN_POINT('Ctrl Pts',(-3.96742034232716,-5.48473129370227,
63.9980285022123));
#24644=CARTESIAN_POINT('Ctrl Pts',(-3.82458547763046,-5.58527899973977,
64.0062375463669));
#24645=CARTESIAN_POINT('Ctrl Pts',(-3.6779750017535,-5.68021028540989,64.0144465905215));
#24646=CARTESIAN_POINT('Ctrl Pts',(-3.53145990569484,-5.77507981199545,
64.0226502941495));
#24647=CARTESIAN_POINT('Ctrl Pts',(-3.38117439093799,-5.86434000225391,
64.0308539977775));
#24648=CARTESIAN_POINT('Ctrl Pts',(-3.22758889044179,-5.94768517612497,
64.0390577014056));
#24649=CARTESIAN_POINT('Ctrl Pts',(-3.07407255897636,-6.03099281451985,
64.0472577103995));
#24650=CARTESIAN_POINT('Ctrl Pts',(-2.91725951703486,-6.1083905731466,64.0554577193934));
#24651=CARTESIAN_POINT('Ctrl Pts',(-2.75764684846178,-6.17961753340519,
64.0636577283874));
#24652=CARTESIAN_POINT('Ctrl Pts',(-2.59804694285403,-6.25083879820594,
64.0718570816913));
#24653=CARTESIAN_POINT('Ctrl Pts',(-2.43564818000986,-6.31589009354785,
64.0800564349952));
#24654=CARTESIAN_POINT('Ctrl Pts',(-2.27097012292736,-6.37455752980325,
64.0882557882992));
#24655=CARTESIAN_POINT('Ctrl Pts',(-2.10629313949679,-6.43322458356442,
64.0964550881457));
#24656=CARTESIAN_POINT('Ctrl Pts',(-1.93933722878695,-6.48550773980239,
64.1046543879924));
#24657=CARTESIAN_POINT('Ctrl Pts',(-1.77063959705818,-6.53124218026936,
64.1128536878389));
#24658=CARTESIAN_POINT('Ctrl Pts',(-1.60191246178225,-6.5769846192376,64.121054421662));
#24659=CARTESIAN_POINT('Ctrl Pts',(-1.43144334463502,-6.61617596679467,
64.129255155485));
#24660=CARTESIAN_POINT('Ctrl Pts',(-1.25978224665404,-6.64870195534552,
64.137455889308));
#24661=CARTESIAN_POINT('Ctrl Pts',(-1.08805998549927,-6.68123953296759,
64.145659545068));
#24662=CARTESIAN_POINT('Ctrl Pts',(-0.915145249504272,-6.70710695399991,
64.153863200828));
#24663=CARTESIAN_POINT('Ctrl Pts',(-0.74159586278167,-6.72624148959173,
64.162066856588));
#24664=CARTESIAN_POINT('Ctrl Pts',(-0.567847664080384,-6.74539794502408,
64.170279910163));
#24665=CARTESIAN_POINT('Ctrl Pts',(-0.393463718880097,-6.75780606641138,
64.1784929637381));
#24666=CARTESIAN_POINT('Ctrl Pts',(-0.219005651738879,-6.76345514692797,
64.1867060173131));
#24667=CARTESIAN_POINT('Ctrl Pts',(-0.0444443538451033,-6.76910757013225,
64.1949239307362));
#24668=CARTESIAN_POINT('Ctrl Pts',(0.13019079550207,-6.76799298229928,64.2031418441593));
#24669=CARTESIAN_POINT('Ctrl Pts',(0.304340682312922,-6.76015279036571,
64.2113597575824));
#24670=CARTESIAN_POINT('Ctrl Pts',(0.478762184203271,-6.75230037037736,
64.2195904881783));
#24671=CARTESIAN_POINT('Ctrl Pts',(0.652696554015657,-6.7377014134082,64.2278212187743));
#24672=CARTESIAN_POINT('Ctrl Pts',(0.825590936044537,-6.71644910695534,
64.2360519493703));
#24673=CARTESIAN_POINT('Ctrl Pts',(0.984373748163748,-6.69693140520583,
64.2436108910461));
#24674=CARTESIAN_POINT('Ctrl Pts',(1.14227931093385,-6.6718027559243,64.2511698327218));
#24675=CARTESIAN_POINT('Ctrl Pts',(1.29888976933328,-6.64117266505858,64.2587287743976));
#24676=CARTESIAN_POINT('Ctrl Pts',(1.46782675082405,-6.60813173569457,64.2668826665644));
#24677=CARTESIAN_POINT('Ctrl Pts',(1.63577890605571,-6.56858639027811,64.2750365587311));
#24678=CARTESIAN_POINT('Ctrl Pts',(1.80220123910377,-6.52260375109303,64.2831904508978));
#24679=CARTESIAN_POINT('Ctrl Pts',(1.96842049040956,-6.47667722357463,64.291334393038));
#24680=CARTESIAN_POINT('Ctrl Pts',(2.13311328691637,-6.42432913476805,64.2994783351782));
#24681=CARTESIAN_POINT('Ctrl Pts',(2.29574222967256,-6.36567801690425,64.3076222773184));
#24682=CARTESIAN_POINT('Ctrl Pts',(2.45820694983116,-6.30708612490004,64.3157579957113));
#24683=CARTESIAN_POINT('Ctrl Pts',(2.61861162384944,-6.24220399800913,64.3238937141042));
#24684=CARTESIAN_POINT('Ctrl Pts',(2.77643149132963,-6.1712006266166,64.3320294324971));
#24685=CARTESIAN_POINT('Ctrl Pts',(2.93412518986032,-6.10025401880475,64.3401586467973));
#24686=CARTESIAN_POINT('Ctrl Pts',(3.08923786441552,-6.0231960595287,64.3482878610975));
#24687=CARTESIAN_POINT('Ctrl Pts',(3.24126231487832,-5.94024474295038,64.3564170753977));
#24688=CARTESIAN_POINT('Ctrl Pts',(3.39319719455959,-5.85734230018304,64.3645415000731));
#24689=CARTESIAN_POINT('Ctrl Pts',(3.54204715351871,-5.76855358973366,64.3726659247485));
#24690=CARTESIAN_POINT('Ctrl Pts',(3.68732730335867,-5.67414366736565,64.3807903494239));
#24691=CARTESIAN_POINT('Ctrl Pts',(3.83348939671183,-5.57916061633067,64.3889640945581));
#24692=CARTESIAN_POINT('Ctrl Pts',(3.97603785477099,-5.47848803534081,64.3971378396923));
#24693=CARTESIAN_POINT('Ctrl Pts',(4.11450580585539,-5.37244180737049,64.4053115848265));
#24694=CARTESIAN_POINT('Ctrl Pts',(4.25208704869958,-5.26707466841282,64.4134329876886));
#24695=CARTESIAN_POINT('Ctrl Pts',(4.38563961262473,-5.15640274723064,64.4215543905508));
#24696=CARTESIAN_POINT('Ctrl Pts',(4.51473655633834,-5.04077799817272,64.4296757934129));
#24697=CARTESIAN_POINT('Ctrl Pts',(4.64384348114784,-4.92514430961807,64.4377978241792));
#24698=CARTESIAN_POINT('Ctrl Pts',(4.7684938269026,-4.80455727457664,64.4459198549454));
#24699=CARTESIAN_POINT('Ctrl Pts',(4.88829573248609,-4.67940742314219,64.4540418857117));
#24700=CARTESIAN_POINT('Ctrl Pts',(5.00812971357128,-4.55422406435866,64.4621660910528));
#24701=CARTESIAN_POINT('Ctrl Pts',(5.12311241673919,-4.42447572094981,64.4702902963939));
#24702=CARTESIAN_POINT('Ctrl Pts',(5.23289070154551,-4.29058782752184,64.478414501735));
#24703=CARTESIAN_POINT('Ctrl Pts',(5.34385726032461,-4.15525069029021,64.4866266459775));
#24704=CARTESIAN_POINT('Ctrl Pts',(5.44950583014637,-4.01568416011006,64.4948387902199));
#24705=CARTESIAN_POINT('Ctrl Pts',(5.54951570161092,-3.87235903262777,64.5030509344624));
#24706=CARTESIAN_POINT('Ctrl Pts',(5.64861259317411,-3.7303423055947,64.5111881108788));
#24707=CARTESIAN_POINT('Ctrl Pts',(5.74217316368213,-3.58463566111503,64.5193252872953));
#24708=CARTESIAN_POINT('Ctrl Pts',(5.82993113162976,-3.43572292253816,64.5274624637117));
#24709=CARTESIAN_POINT('Ctrl Pts',(5.91890187113345,-3.28475228383092,64.5357120918672));
#24710=CARTESIAN_POINT('Ctrl Pts',(6.00190826949739,-3.13048663444368,64.5439617200226));
#24711=CARTESIAN_POINT('Ctrl Pts',(6.07872300777909,-2.97345179794413,64.5522113481781));
#24712=CARTESIAN_POINT('Ctrl Pts',(6.15553774606078,-2.81641696144457,64.5604609763335));
#24713=CARTESIAN_POINT('Ctrl Pts',(6.22616072658722,-2.65661331534446,64.5687106044889));
#24714=CARTESIAN_POINT('Ctrl Pts',(6.29041691467294,-2.49458293900937,64.5769602326444));
#24715=CARTESIAN_POINT('Ctrl Pts',(6.35448024389379,-2.33303888150807,64.585185100322));
#24716=CARTESIAN_POINT('Ctrl Pts',(6.41240659834632,-2.16879863247724,64.5934099679995));
#24717=CARTESIAN_POINT('Ctrl Pts',(6.46396227940405,-2.00236875985461,64.6016348356771));
#24718=CARTESIAN_POINT('Ctrl Pts',(6.51545987721636,-1.83612638911222,64.6098504371206));
#24719=CARTESIAN_POINT('Ctrl Pts',(6.56060098822739,-1.66769964649672,64.6180660385642));
#24720=CARTESIAN_POINT('Ctrl Pts',(6.59919968439063,-1.49761561341308,64.6262816400077));
#24721=CARTESIAN_POINT('Ctrl Pts',(6.63776265005493,-1.32768902573478,64.6344896363359));
#24722=CARTESIAN_POINT('Ctrl Pts',(6.66979518313659,-1.15610855052929,64.642697632664));
#24723=CARTESIAN_POINT('Ctrl Pts',(6.69516092787743,-0.983417078265128,
64.6509056289921));
#24724=CARTESIAN_POINT('Ctrl Pts',(6.72050828659645,-0.810850779111668,
64.6591076758636));
#24725=CARTESIAN_POINT('Ctrl Pts',(6.73919843014089,-0.637175440410905,
64.667309722735));
#24726=CARTESIAN_POINT('Ctrl Pts',(6.75114590405125,-0.462944901918249,
64.6755117696065));
#24727=CARTESIAN_POINT('Ctrl Pts',(6.76308711715413,-0.288805665056759,
64.683709518378));
#24728=CARTESIAN_POINT('Ctrl Pts',(6.76829267512614,-0.114112165085269,
64.6919072671496));
#24729=CARTESIAN_POINT('Ctrl Pts',(6.76672886816929,0.0605757763829547,
64.7001050159211));
#24730=CARTESIAN_POINT('Ctrl Pts',(6.76516535947721,0.235230399634836,64.7083012011367));
#24731=CARTESIAN_POINT('Ctrl Pts',(6.75683505459466,0.409879108046038,64.7164973863524));
#24732=CARTESIAN_POINT('Ctrl Pts',(6.74175634871382,0.583960901582418,64.724693571568));
#24733=CARTESIAN_POINT('Ctrl Pts',(6.72667875832161,0.758029816940473,64.7328891504484));
#24734=CARTESIAN_POINT('Ctrl Pts',(6.70485379123764,0.931531543383801,64.7410847293287));
#24735=CARTESIAN_POINT('Ctrl Pts',(6.67635182832526,1.10390908340225,64.7492803082091));
#24736=CARTESIAN_POINT('Ctrl Pts',(6.64784678832906,1.27630523337192,64.7574767718875));
#24737=CARTESIAN_POINT('Ctrl Pts',(6.61266337489708,1.44757660101982,64.765673235566));
#24738=CARTESIAN_POINT('Ctrl Pts',(6.57092332096869,1.61717522549347,64.7738696992444));
#24739=CARTESIAN_POINT('Ctrl Pts',(6.52917116662659,1.78682301649487,64.7820685390722));
#24740=CARTESIAN_POINT('Ctrl Pts',(6.48085867143856,1.95479675006364,64.7902673789));
#24741=CARTESIAN_POINT('Ctrl Pts',(6.42615778718546,2.12056244760574,64.7984662187278));
#24742=CARTESIAN_POINT('Ctrl Pts',(6.37139976630256,2.28650129213487,64.806673622477));
#24743=CARTESIAN_POINT('Ctrl Pts',(6.31024013745913,2.45022715162502,64.8148810262263));
#24744=CARTESIAN_POINT('Ctrl Pts',(6.24289984237217,2.61122395786143,64.8230884299755));
#24745=CARTESIAN_POINT('Ctrl Pts',(6.17552347625953,2.77230700250717,64.8313002300446));
#24746=CARTESIAN_POINT('Ctrl Pts',(6.10195999499159,2.93065775459247,64.8395120301136));
#24747=CARTESIAN_POINT('Ctrl Pts',(6.02247685234882,3.08578378421474,64.8477238301826));
#24748=CARTESIAN_POINT('Ctrl Pts',(5.94287669941409,3.24113818102802,64.8559477191688));
#24749=CARTESIAN_POINT('Ctrl Pts',(5.85733964515753,3.39325805536864,64.8641716081549));
#24750=CARTESIAN_POINT('Ctrl Pts',(5.76617778938328,3.54167794995859,64.8723954971411));
#24751=CARTESIAN_POINT('Ctrl Pts',(5.68194581063761,3.67881536670334,64.8799942283911));
#24752=CARTESIAN_POINT('Ctrl Pts',(5.59291229325792,3.81279409181644,64.8875929596412));
#24753=CARTESIAN_POINT('Ctrl Pts',(5.49935390779853,3.94327219410239,64.8951916908913));
#24754=CARTESIAN_POINT('Ctrl Pts',(5.3980829195581,4.08450642230494,64.903416833077));
#24755=CARTESIAN_POINT('Ctrl Pts',(5.29122553709665,4.22203511372218,64.9116419752628));
#24756=CARTESIAN_POINT('Ctrl Pts',(5.17908162278455,4.35538776052551,64.9198671174485));
#24757=CARTESIAN_POINT('Ctrl Pts',(5.06705998759757,4.48859500269335,64.9280832911298));
#24758=CARTESIAN_POINT('Ctrl Pts',(4.94976352614232,4.61763499403864,64.9362994648111));
#24759=CARTESIAN_POINT('Ctrl Pts',(4.82753522675317,4.74206628322056,64.9445156384924));
#24760=CARTESIAN_POINT('Ctrl Pts',(4.7019751711756,4.86988937871769,64.9529557724812));
#24761=CARTESIAN_POINT('Ctrl Pts',(4.57121077534139,4.99284861819941,64.9613959064699));
#24762=CARTESIAN_POINT('Ctrl Pts',(4.43565908084522,5.11050071113539,64.9698360404586));
#24763=CARTESIAN_POINT('Ctrl Pts',(4.30393800121349,5.22482802190831,64.9780376609944));
#24764=CARTESIAN_POINT('Ctrl Pts',(4.16769680793882,5.33414380210309,64.9862392815301));
#24765=CARTESIAN_POINT('Ctrl Pts',(4.02735618745112,5.4380778901556,64.9944409020658));
#24766=CARTESIAN_POINT('Ctrl Pts',(3.88089364401347,5.54654577944627,65.0030002927811));
#24767=CARTESIAN_POINT('Ctrl Pts',(3.7299662655183,5.64915161858864,65.0115596834963));
#24768=CARTESIAN_POINT('Ctrl Pts',(3.57509119478739,5.74552103372303,65.0201190742116));
#24769=CARTESIAN_POINT('Ctrl Pts',(3.42021612405647,5.84189044885741,65.0286784649268));
#24770=CARTESIAN_POINT('Ctrl Pts',(3.26139372758728,5.93202318678242,65.0372378556421));
#24771=CARTESIAN_POINT('Ctrl Pts',(3.09917575053256,6.01559628526641,65.0457972463573));
#24772=CARTESIAN_POINT('Ctrl Pts',(3.09917575053259,6.01559628526639,63.0459622914914));
#24773=CARTESIAN_POINT('Ctrl Pts',(2.94550623433066,6.09476530120842,63.0540930631184));
#24774=CARTESIAN_POINT('Ctrl Pts',(2.78865426101915,6.168117870594,63.0622238347455));
#24775=CARTESIAN_POINT('Ctrl Pts',(2.6291048227603,6.23539067187763,63.0703546063725));
#24776=CARTESIAN_POINT('Ctrl Pts',(2.46965807767459,6.30262017336964,63.0784801446703));
#24777=CARTESIAN_POINT('Ctrl Pts',(2.30751766087169,6.36377755756109,63.0866056829681));
#24778=CARTESIAN_POINT('Ctrl Pts',(2.14319177109584,6.41864612144236,63.0947312212659));
#24779=CARTESIAN_POINT('Ctrl Pts',(1.97893710493117,6.47349090369515,63.1028532377195));
#24780=CARTESIAN_POINT('Ctrl Pts',(1.81249919881251,6.52205217898337,63.1109752541731));
#24781=CARTESIAN_POINT('Ctrl Pts',(1.64440476370505,6.56416193989028,63.1190972706267));
#24782=CARTESIAN_POINT('Ctrl Pts',(1.47631779800722,6.60626982961655,63.127218926172));
#24783=CARTESIAN_POINT('Ctrl Pts',(1.30657480222966,6.64192667751996,63.1353405817174));
#24784=CARTESIAN_POINT('Ctrl Pts',(1.13571641098715,6.67101470795969,63.1434622372628));
#24785=CARTESIAN_POINT('Ctrl Pts',(0.964853172710025,6.70010356358973,63.1515841232091));
#24786=CARTESIAN_POINT('Ctrl Pts',(0.792874836639891,6.72262316836435,63.1597060091555));
#24787=CARTESIAN_POINT('Ctrl Pts',(0.620330728893733,6.7385071630733,63.1678278951018));
#24788=CARTESIAN_POINT('Ctrl Pts',(0.447748870088166,6.7543946330538,63.1759515580419));
#24789=CARTESIAN_POINT('Ctrl Pts',(0.274601357510065,6.76364356823193,63.1840752209821));
#24790=CARTESIAN_POINT('Ctrl Pts',(0.101441073081922,6.76623962838237,63.1921988839222));
#24791=CARTESIAN_POINT('Ctrl Pts',(-0.0717900733916588,6.76883675091344,
63.200325871293));
#24792=CARTESIAN_POINT('Ctrl Pts',(-0.245033636566598,6.76477557157275,
63.2084528586638));
#24793=CARTESIAN_POINT('Ctrl Pts',(-0.417738348494154,6.75409384537981,
63.2165798460347));
#24794=CARTESIAN_POINT('Ctrl Pts',(-0.590646486797809,6.74339953733646,
63.2247164060661));
#24795=CARTESIAN_POINT('Ctrl Pts',(-0.763014140958481,6.72606913119763,
63.2328529660975));
#24796=CARTESIAN_POINT('Ctrl Pts',(-0.934295864837633,6.70219219635988,
63.240989526129));
#24797=CARTESIAN_POINT('Ctrl Pts',(-1.10568971810508,6.67829963051354,63.2491314127503));
#24798=CARTESIAN_POINT('Ctrl Pts',(-1.27599586574884,6.64785206168226,63.2572732993716));
#24799=CARTESIAN_POINT('Ctrl Pts',(-1.44468094551783,6.61098978713912,63.2654151859929));
#24800=CARTESIAN_POINT('Ctrl Pts',(-1.61361837281639,6.57407236780233,63.2735692526184));
#24801=CARTESIAN_POINT('Ctrl Pts',(-1.78092953606017,6.53072116885973,63.2817233192439));
#24802=CARTESIAN_POINT('Ctrl Pts',(-1.94609709820228,6.48112606607592,63.2898773858694));
#24803=CARTESIAN_POINT('Ctrl Pts',(-2.04168455420969,6.45242388240227,63.2945963904653));
#24804=CARTESIAN_POINT('Ctrl Pts',(-2.13655442647952,6.42163133589962,63.2993153950612));
#24805=CARTESIAN_POINT('Ctrl Pts',(-2.23060992106565,6.38879240389321,63.3040343996572));
#24806=CARTESIAN_POINT('Ctrl Pts',(-2.39467913819437,6.33150858555442,63.312266171688));
#24807=CARTESIAN_POINT('Ctrl Pts',(-2.55678115665872,6.26781647570823,63.3204979437188));
#24808=CARTESIAN_POINT('Ctrl Pts',(-2.71637917710084,6.19786843731076,63.3287297157497));
#24809=CARTESIAN_POINT('Ctrl Pts',(-2.87578662155742,6.12800392386127,63.3369516582221));
#24810=CARTESIAN_POINT('Ctrl Pts',(-3.03269569687596,6.05189849917589,63.3451736006945));
#24811=CARTESIAN_POINT('Ctrl Pts',(-3.18658507162592,5.96975414747465,63.3533955431669));
#24812=CARTESIAN_POINT('Ctrl Pts',(-3.340321520173,5.88769142599522,63.3616093151568));
#24813=CARTESIAN_POINT('Ctrl Pts',(-3.49104393031614,5.79960189629139,63.3698230871467));
#24814=CARTESIAN_POINT('Ctrl Pts',(-3.63825118030288,5.70573547836076,63.3780368591366));
#24815=CARTESIAN_POINT('Ctrl Pts',(-3.78534162794163,5.61194353922118,63.3862441138669));
#24816=CARTESIAN_POINT('Ctrl Pts',(-3.92892216999375,5.51238403337113,63.3944513685973));
#24817=CARTESIAN_POINT('Ctrl Pts',(-4.06851644748125,5.40735267174008,63.4026586233277));
#24818=CARTESIAN_POINT('Ctrl Pts',(-4.20802791466854,5.30238361695101,63.4108610093396));
#24819=CARTESIAN_POINT('Ctrl Pts',(-4.34355754257503,5.19194938769162,63.4190633953516));
#24820=CARTESIAN_POINT('Ctrl Pts',(-4.47465805488804,5.07638890273643,63.4272657813635));
#24821=CARTESIAN_POINT('Ctrl Pts',(-4.60571943687818,4.9608629097829,63.4354657191622));
#24822=CARTESIAN_POINT('Ctrl Pts',(-4.73235406559019,4.84021394268184,63.4436656569609));
#24823=CARTESIAN_POINT('Ctrl Pts',(-4.85414767600162,4.71482124152847,63.4518655947596));
#24824=CARTESIAN_POINT('Ctrl Pts',(-4.97592425652285,4.58944607351109,63.4600643859954));
#24825=CARTESIAN_POINT('Ctrl Pts',(-5.09286091665338,4.45932874893275,63.4682631772311));
#24826=CARTESIAN_POINT('Ctrl Pts',(-5.2045802034484,4.32488542112656,63.4764619684669));
#24827=CARTESIAN_POINT('Ctrl Pts',(-5.31630413546221,4.19043650325002,63.4846611006033));
#24828=CARTESIAN_POINT('Ctrl Pts',(-5.4228100328044,4.05166149943201,63.4928602327397));
#24829=CARTESIAN_POINT('Ctrl Pts',(-5.52376066847092,3.90900973105129,63.5010593648761));
#24830=CARTESIAN_POINT('Ctrl Pts',(-5.62473381450443,3.76632615362217,63.509260325287));
#24831=CARTESIAN_POINT('Ctrl Pts',(-5.72014902465459,3.61976438240121,63.517461285698));
#24832=CARTESIAN_POINT('Ctrl Pts',(-5.80971232107568,3.46980283969298,63.5256622461089));
#24833=CARTESIAN_POINT('Ctrl Pts',(-5.89935955986601,3.31970074691911,63.5338708927939));
#24834=CARTESIAN_POINT('Ctrl Pts',(-5.98314374290121,3.1661928245452,63.5420795394789));
#24835=CARTESIAN_POINT('Ctrl Pts',(-6.06081635948654,3.00978305805923,63.550288186164));
#24836=CARTESIAN_POINT('Ctrl Pts',(-6.13852605916045,2.85329861715798,63.5585007518875));
#24837=CARTESIAN_POINT('Ctrl Pts',(-6.21011822793787,2.69390989663681,63.566713317611));
#24838=CARTESIAN_POINT('Ctrl Pts',(-6.27539252680471,2.53214091916774,63.5749258833345));
#24839=CARTESIAN_POINT('Ctrl Pts',(-6.34075639142878,2.37014997131804,63.5831497178833));
#24840=CARTESIAN_POINT('Ctrl Pts',(-6.39978493946788,2.20577257659968,63.591373552432));
#24841=CARTESIAN_POINT('Ctrl Pts',(-6.45232735118248,2.03954915439232,63.5995973869808));
#24842=CARTESIAN_POINT('Ctrl Pts',(-6.50060394385643,1.88682109747779,63.6071535439552));
#24843=CARTESIAN_POINT('Ctrl Pts',(-6.54340536908842,1.73253496099723,63.6147097009296));
#24844=CARTESIAN_POINT('Ctrl Pts',(-6.58065285209234,1.57711668567957,63.622265857904));
#24845=CARTESIAN_POINT('Ctrl Pts',(-6.63190660814036,1.3632560506483,63.6326633772796));
#24846=CARTESIAN_POINT('Ctrl Pts',(-6.67274538650549,1.14683583986141,63.6430608966552));
#24847=CARTESIAN_POINT('Ctrl Pts',(-6.70296292886345,0.928750221686325,
63.6534584160308));
#24848=CARTESIAN_POINT('Ctrl Pts',(-6.732835253359,0.713156104972025,63.6637371497894));
#24849=CARTESIAN_POINT('Ctrl Pts',(-6.75232765311494,0.495934283327142,
63.674015883548));
#24850=CARTESIAN_POINT('Ctrl Pts',(-6.76128863461862,0.277965824116989,
63.6842946173066));
#24851=CARTESIAN_POINT('Ctrl Pts',(-6.76503305623774,0.186885867014341,
63.6885896728077));
#24852=CARTESIAN_POINT('Ctrl Pts',(-6.76693921015938,0.0956757623781489,
63.6928847283089));
#24853=CARTESIAN_POINT('Ctrl Pts',(-6.76699856901969,0.00440078236972949,
63.69717978381));
#24854=CARTESIAN_POINT('',(-6.76699754938808,0.00575904295465441,63.3028202162211));
#24855=CARTESIAN_POINT('Ctrl Pts',(3.09917575053255,6.01559628526641,62.6516502284592));
#24856=CARTESIAN_POINT('Ctrl Pts',(2.94565184939477,6.09469028176659,62.6597889318832));
#24857=CARTESIAN_POINT('Ctrl Pts',(2.78891768509697,6.16799628340453,62.6679276353073));
#24858=CARTESIAN_POINT('Ctrl Pts',(2.6294535729494,6.23524361253862,62.6760663387313));
#24859=CARTESIAN_POINT('Ctrl Pts',(2.47012263887975,6.30243477938065,62.6841982450343));
#24860=CARTESIAN_POINT('Ctrl Pts',(2.30806663153626,6.36357720714301,62.6923301513372));
#24861=CARTESIAN_POINT('Ctrl Pts',(2.1437899634967,6.418446353473,62.7004620576402));
#24862=CARTESIAN_POINT('Ctrl Pts',(1.97961598145489,6.47328120221768,62.7085888808542));
#24863=CARTESIAN_POINT('Ctrl Pts',(1.81322444865879,6.52185046297917,62.7167157040682));
#24864=CARTESIAN_POINT('Ctrl Pts',(1.6451392279764,6.56397790372372,62.7248425272822));
#24865=CARTESIAN_POINT('Ctrl Pts',(1.47262848185054,6.60721452027877,62.7331833220921));
#24866=CARTESIAN_POINT('Ctrl Pts',(1.29833399745046,6.64366528018179,62.7415241169019));
#24867=CARTESIAN_POINT('Ctrl Pts',(1.1228388075019,6.67319428852238,62.7498649117118));
#24868=CARTESIAN_POINT('Ctrl Pts',(0.951923374720132,6.70195270202436,62.7579880434916));
#24869=CARTESIAN_POINT('Ctrl Pts',(0.779869504139152,6.72414606989112,62.7661111752714));
#24870=CARTESIAN_POINT('Ctrl Pts',(0.607225751379997,6.73970072680242,62.7742343070512));
#24871=CARTESIAN_POINT('Ctrl Pts',(0.434573703316043,6.75525613109448,62.7823578291368));
#24872=CARTESIAN_POINT('Ctrl Pts',(0.261332080946672,6.76417215593664,62.7904813512224));
#24873=CARTESIAN_POINT('Ctrl Pts',(0.0880539029469755,6.76642708600158,
62.798604873308));
#24874=CARTESIAN_POINT('Ctrl Pts',(-0.0852655664839576,6.76868255340648,
62.8067303311933));
#24875=CARTESIAN_POINT('Ctrl Pts',(-0.258621243203989,6.76427376061019,
62.8148557890786));
#24876=CARTESIAN_POINT('Ctrl Pts',(-0.431460810487573,6.75323112065724,
62.8229812469639));
#24877=CARTESIAN_POINT('Ctrl Pts',(-0.612338934353396,6.74167490104499,
62.8314846099435));
#24878=CARTESIAN_POINT('Ctrl Pts',(-0.792651343496034,6.72285303507262,
62.8399879729232));
#24879=CARTESIAN_POINT('Ctrl Pts',(-0.97177279733705,6.69686095348826,62.8484913359028));
#24880=CARTESIAN_POINT('Ctrl Pts',(-1.14320331372459,6.67198489385139,62.8566295900056));
#24881=CARTESIAN_POINT('Ctrl Pts',(-1.31354266533925,6.64054162568567,62.8647678441084));
#24882=CARTESIAN_POINT('Ctrl Pts',(-1.4822551784215,6.60266677835878,62.8729060982112));
#24883=CARTESIAN_POINT('Ctrl Pts',(-1.65108271136965,6.56476610983,62.881049900574));
#24884=CARTESIAN_POINT('Ctrl Pts',(-1.81828084427154,6.52042522003151,62.8891937029369));
#24885=CARTESIAN_POINT('Ctrl Pts',(-1.98333029704277,6.46982920430147,62.8973375052997));
#24886=CARTESIAN_POINT('Ctrl Pts',(-2.14859502525585,6.4191671957465,62.9054919296951));
#24887=CARTESIAN_POINT('Ctrl Pts',(-2.31170513660626,6.36223389716979,62.9136463540905));
#24888=CARTESIAN_POINT('Ctrl Pts',(-2.47216188947549,6.29926222602496,62.9218007784858));
#24889=CARTESIAN_POINT('Ctrl Pts',(-2.49328755790541,6.29097140235257,62.9228743865636));
#24890=CARTESIAN_POINT('Ctrl Pts',(-2.51436726845114,6.28257597265725,62.9239479946414));
#24891=CARTESIAN_POINT('Ctrl Pts',(-2.53539991657681,6.27407652671071,62.9250216027191));
#24892=CARTESIAN_POINT('Ctrl Pts',(-2.69655645961628,6.20895199658447,62.9332478120561));
#24893=CARTESIAN_POINT('Ctrl Pts',(-2.85542747637427,6.13752321639356,62.9414740213931));
#24894=CARTESIAN_POINT('Ctrl Pts',(-3.01148497277787,6.05997089586519,62.94970023073));
#24895=CARTESIAN_POINT('Ctrl Pts',(-3.16736714526967,5.98250570204663,62.9579171982732));
#24896=CARTESIAN_POINT('Ctrl Pts',(-3.32044177330885,5.89893082506714,62.9661341658164));
#24897=CARTESIAN_POINT('Ctrl Pts',(-3.47019900586617,5.80947569576511,62.9743511333596));
#24898=CARTESIAN_POINT('Ctrl Pts',(-3.61981805006439,5.72010311110763,62.982560518703));
#24899=CARTESIAN_POINT('Ctrl Pts',(-3.76612548916819,5.62486126296155,62.9907699040464));
#24900=CARTESIAN_POINT('Ctrl Pts',(-3.90863426053248,5.52402635922311,62.9989792893898));
#24901=CARTESIAN_POINT('Ctrl Pts',(-4.05104012552073,5.42326426892922,63.0071827466903));
#24902=CARTESIAN_POINT('Ctrl Pts',(-4.18965249485716,5.31691737390216,63.0153862039909));
#24903=CARTESIAN_POINT('Ctrl Pts',(-4.32401152580629,5.20530626617631,63.0235896612915));
#24904=CARTESIAN_POINT('Ctrl Pts',(-4.45830048744434,5.09375336453734,63.0317888404233));
#24905=CARTESIAN_POINT('Ctrl Pts',(-4.58834025443122,4.97694194800198,63.0399880195552));
#24906=CARTESIAN_POINT('Ctrl Pts',(-4.7137023782453,4.85523417450947,63.0481871986871));
#24907=CARTESIAN_POINT('Ctrl Pts',(-4.8390408811333,4.73354933338466,63.0563848329169));
#24908=CARTESIAN_POINT('Ctrl Pts',(-4.95970323506052,4.6069702180812,63.0645824671467));
#24909=CARTESIAN_POINT('Ctrl Pts',(-5.07529610806809,4.47589749831572,63.0727801013765));
#24910=CARTESIAN_POINT('Ctrl Pts',(-5.19088063745551,4.34483423952268,63.0809771438921));
#24911=CARTESIAN_POINT('Ctrl Pts',(-5.30139617677094,4.20927829066182,63.0891741864077));
#24912=CARTESIAN_POINT('Ctrl Pts',(-5.40648817564024,4.06966517132089,63.0973712289233));
#24913=CARTESIAN_POINT('Ctrl Pts',(-5.5115916891486,3.9300367549574,63.1055691695661));
#24914=CARTESIAN_POINT('Ctrl Pts',(-5.61127026255347,3.78635056910221,63.1137671102089));
#24915=CARTESIAN_POINT('Ctrl Pts',(-5.70521133069505,3.63907305121907,63.1219650508518));
#24916=CARTESIAN_POINT('Ctrl Pts',(-5.79917976539459,3.49175262900442,63.1301653796878));
#24917=CARTESIAN_POINT('Ctrl Pts',(-5.88740717270984,3.34083909315635,63.1383657085238));
#24918=CARTESIAN_POINT('Ctrl Pts',(-5.96962576769131,3.18682556687935,63.1465660373598));
#24919=CARTESIAN_POINT('Ctrl Pts',(-6.05193003658202,3.0326515545119,63.1547749111512));
#24920=CARTESIAN_POINT('Ctrl Pts',(-6.12821281479293,2.87537141495665,63.1629837849426));
#24921=CARTESIAN_POINT('Ctrl Pts',(-6.19825309286485,2.71550135275079,63.171192658734));
#24922=CARTESIAN_POINT('Ctrl Pts',(-6.26833096078139,2.55554549004607,63.1794059381374));
#24923=CARTESIAN_POINT('Ctrl Pts',(-6.33215951868453,2.3929972672502,63.1876192175408));
#24924=CARTESIAN_POINT('Ctrl Pts',(-6.38956696334292,2.22839023085202,63.1958324969443));
#24925=CARTESIAN_POINT('Ctrl Pts',(-6.44705837541194,2.06354243079159,63.2040577895597));
#24926=CARTESIAN_POINT('Ctrl Pts',(-6.49810980025971,1.8966301421379,63.2122830821752));
#24927=CARTESIAN_POINT('Ctrl Pts',(-6.54259976850742,1.7282005870635,63.2205083747906));
#24928=CARTESIAN_POINT('Ctrl Pts',(-6.5828356004554,1.57587628700304,63.2279471639027));
#24929=CARTESIAN_POINT('Ctrl Pts',(-6.61770542251439,1.42231133974596,63.2353859530148));
#24930=CARTESIAN_POINT('Ctrl Pts',(-6.64715585439012,1.26791484234833,63.2428247421268));
#24931=CARTESIAN_POINT('Ctrl Pts',(-6.69446442975949,1.01989544607171,63.2547742618096));
#24932=CARTESIAN_POINT('Ctrl Pts',(-6.7279021089193,0.769153761022326,63.2667237814924));
#24933=CARTESIAN_POINT('Ctrl Pts',(-6.74722475137883,0.516959528765004,
63.2786733011752));
#24934=CARTESIAN_POINT('Ctrl Pts',(-6.76024011985427,0.347086238034466,
63.2867222728467));
#24935=CARTESIAN_POINT('Ctrl Pts',(-6.76685219440396,0.176554210769674,
63.2947712445183));
#24936=CARTESIAN_POINT('Ctrl Pts',(-6.76699754938751,0.00575904361896699,
63.3028202161898));
#24937=CARTESIAN_POINT('Ctrl Pts',(-6.76699754938808,0.00575904295474457,
63.3028202162211));
#24938=CARTESIAN_POINT('Ctrl Pts',(-6.76714384492322,-0.166141311942916,
63.3109212714791));
#24939=CARTESIAN_POINT('Ctrl Pts',(-6.76073587822894,-0.338250077316013,
63.3190223267372));
#24940=CARTESIAN_POINT('Ctrl Pts',(-6.74775279763134,-0.510020766301218,
63.3271233819952));
#24941=CARTESIAN_POINT('Ctrl Pts',(-6.73478004839695,-0.681654767744205,
63.3352179907906));
#24942=CARTESIAN_POINT('Ctrl Pts',(-6.71524262925384,-0.852950861782448,
63.343312599586));
#24943=CARTESIAN_POINT('Ctrl Pts',(-6.68917174575775,-1.02336227981893,
63.3514072083814));
#24944=CARTESIAN_POINT('Ctrl Pts',(-6.66311601068548,-1.19367468071303,
63.3594971138239));
#24945=CARTESIAN_POINT('Ctrl Pts',(-6.63053442608599,-1.36310306491456,
63.3675870192664));
#24946=CARTESIAN_POINT('Ctrl Pts',(-6.5915100512617,-1.53110556269516,63.3756769247089));
#24947=CARTESIAN_POINT('Ctrl Pts',(-6.55249553017716,-1.69906563947865,
63.3837647874327));
#24948=CARTESIAN_POINT('Ctrl Pts',(-6.50704153611983,-1.86560018592668,
63.3918526501564));
#24949=CARTESIAN_POINT('Ctrl Pts',(-6.45528230229601,-2.03017718381032,
63.3999405128801));
#24950=CARTESIAN_POINT('Ctrl Pts',(-6.40352824864249,-2.19473771049037,
63.408027566154));
#24951=CARTESIAN_POINT('Ctrl Pts',(-6.34547032152564,-2.3573407257823,63.4161146194278));
#24952=CARTESIAN_POINT('Ctrl Pts',(-6.28129268559602,-2.51746920495126,
63.4242016727017));
#24953=CARTESIAN_POINT('Ctrl Pts',(-6.21710899763722,-2.67761278443071,
63.4322894885945));
#24954=CARTESIAN_POINT('Ctrl Pts',(-6.14680458952733,-2.83528102006325,
63.4403773044873));
#24955=CARTESIAN_POINT('Ctrl Pts',(-6.07061180844132,-2.98997680111615,
63.4484651203801));
#24956=CARTESIAN_POINT('Ctrl Pts',(-5.99439703007437,-3.14471724370401,
63.4565552712705));
#24957=CARTESIAN_POINT('Ctrl Pts',(-5.91229065799742,-3.29648319201542,
63.4646454221609));
#24958=CARTESIAN_POINT('Ctrl Pts',(-5.82457097603429,-3.44480216342521,
63.4727355730513));
#24959=CARTESIAN_POINT('Ctrl Pts',(-5.7367623042207,-3.59327160144396,63.4808339312368));
#24960=CARTESIAN_POINT('Ctrl Pts',(-5.643329138574,-3.73828676081582,63.4889322894223));
#24961=CARTESIAN_POINT('Ctrl Pts',(-5.54459350453892,-3.87940354557564,
63.4970306476078));
#24962=CARTESIAN_POINT('Ctrl Pts',(-5.44580282713146,-4.02059900045095,
63.505133520485));
#24963=CARTESIAN_POINT('Ctrl Pts',(-5.34170401533324,-4.15789145744062,
63.5132363933622));
#24964=CARTESIAN_POINT('Ctrl Pts',(-5.23265910186198,-4.29087027579499,
63.5213392662394));
#24965=CARTESIAN_POINT('Ctrl Pts',(-5.12346411066267,-4.42403211193811,
63.529453291042));
#24966=CARTESIAN_POINT('Ctrl Pts',(-5.00930966717568,-4.55286817695293,
63.5375673158447));
#24967=CARTESIAN_POINT('Ctrl Pts',(-4.89059495869637,-4.67700437780142,
63.5456813406474));
#24968=CARTESIAN_POINT('Ctrl Pts',(-4.81770165410644,-4.75322659167025,
63.5506635209431));
#24969=CARTESIAN_POINT('Ctrl Pts',(-4.74308971382623,-4.82767762154433,
63.5556457012388));
#24970=CARTESIAN_POINT('Ctrl Pts',(-4.66685749085739,-4.90027857983893,
63.5606278815345));
#24971=CARTESIAN_POINT('Ctrl Pts',(-4.54211542089365,-5.01907865500823,
63.5687804377477));
#24972=CARTESIAN_POINT('Ctrl Pts',(-4.41263899382622,-5.13329826570113,
63.576932993961));
#24973=CARTESIAN_POINT('Ctrl Pts',(-4.27880063039264,-5.24253318209352,
63.5850855501743));
#24974=CARTESIAN_POINT('Ctrl Pts',(-4.14511732192962,-5.35164154720187,
63.5932286614546));
#24975=CARTESIAN_POINT('Ctrl Pts',(-4.00708241670659,-5.4557764846935,63.601371772735));
#24976=CARTESIAN_POINT('Ctrl Pts',(-3.86510566326265,-5.5545699394116,63.6095148840153));
#24977=CARTESIAN_POINT('Ctrl Pts',(-3.72326354446627,-5.65326970962408,
63.6176502732927));
#24978=CARTESIAN_POINT('Ctrl Pts',(-3.57748731733342,-5.74663787397875,
63.62578566257));
#24979=CARTESIAN_POINT('Ctrl Pts',(-3.42822034345906,-5.83434608818276,
63.6339210518474));
#24980=CARTESIAN_POINT('Ctrl Pts',(-3.27906355285734,-5.92198955947796,
63.642050435886));
#24981=CARTESIAN_POINT('Ctrl Pts',(-3.12642146010185,-6.0039812152636,63.6501798199246));
#24982=CARTESIAN_POINT('Ctrl Pts',(-2.97076698739765,-6.08003556787198,
63.6583092039632));
#24983=CARTESIAN_POINT('Ctrl Pts',(-2.81519471809391,-6.15604975506593,
63.6664342947553));
#24984=CARTESIAN_POINT('Ctrl Pts',(-2.65661356486749,-6.22613272358849,
63.6745593855475));
#24985=CARTESIAN_POINT('Ctrl Pts',(-2.495521661768,-6.29004456547382,63.6826844763396));
#24986=CARTESIAN_POINT('Ctrl Pts',(-2.33381483595205,-6.35420037271475,
63.6908405823647));
#24987=CARTESIAN_POINT('Ctrl Pts',(-2.16957837914399,-6.41213766546459,
63.6989966883899));
#24988=CARTESIAN_POINT('Ctrl Pts',(-2.00333753862448,-6.46366209716582,
63.707152794415));
#24989=CARTESIAN_POINT('Ctrl Pts',(-1.83776578742289,-6.5149791523478,63.7152760735884));
#24990=CARTESIAN_POINT('Ctrl Pts',(-1.6702061153167,-6.55993478338896,63.7233993527618));
#24991=CARTESIAN_POINT('Ctrl Pts',(-1.50119345572939,-6.59838671255901,
63.7315226319352));
#24992=CARTESIAN_POINT('Ctrl Pts',(-1.33215829067814,-6.63684376192838,
63.7396469927919));
#24993=CARTESIAN_POINT('Ctrl Pts',(-1.16167010952075,-6.6687953033068,63.7477713536486));
#24994=CARTESIAN_POINT('Ctrl Pts',(-0.990274726559195,-6.69415005552894,
63.7558957145053));
#24995=CARTESIAN_POINT('Ctrl Pts',(-0.818823912000534,-6.71951300782267,
63.7640227028907));
#24996=CARTESIAN_POINT('Ctrl Pts',(-0.646465673081908,-6.73827486899703,
63.7721496912762));
#24997=CARTESIAN_POINT('Ctrl Pts',(-0.473751600845935,-6.75039616768497,
63.7802766796616));
#24998=CARTESIAN_POINT('Ctrl Pts',(-0.299920951797434,-6.76259582918885,
63.7884562081016));
#24999=CARTESIAN_POINT('Ctrl Pts',(-0.125730227538434,-6.76806874325794,
63.7966357365417));
#25000=CARTESIAN_POINT('Ctrl Pts',(0.0482584615871252,-6.76682792162511,
63.8048152649818));
#25001=CARTESIAN_POINT('Ctrl Pts',(0.221427781884395,-6.76559294342138,
63.8129562733854));
#25002=CARTESIAN_POINT('Ctrl Pts',(0.394396603800965,-6.75770740860602,
63.8210972817891));
#25003=CARTESIAN_POINT('Ctrl Pts',(0.566616481323942,-6.74323622329013,
63.8292382901928));
#25004=CARTESIAN_POINT('Ctrl Pts',(0.740058673507064,-6.72866233007421,
63.837437078651));
#25005=CARTESIAN_POINT('Ctrl Pts',(0.912740876396846,-6.70740900676458,
63.8456358671093));
#25006=CARTESIAN_POINT('Ctrl Pts',(1.08411431358517,-6.67959468494008,63.8538346555675));
#25007=CARTESIAN_POINT('Ctrl Pts',(1.25548775077344,-6.65178036311559,63.8620334440257));
#25008=CARTESIAN_POINT('Ctrl Pts',(1.42555207109027,-6.61740517985191,63.870232232484));
#25009=CARTESIAN_POINT('Ctrl Pts',(1.59377534453279,-6.57663813442396,63.8784310209422));
#25010=CARTESIAN_POINT('Ctrl Pts',(1.76270160122032,-6.53570072879971,63.8866640710742));
#25011=CARTESIAN_POINT('Ctrl Pts',(1.93029653364513,-6.48819078895483,63.8948971212062));
#25012=CARTESIAN_POINT('Ctrl Pts',(2.09601085815659,-6.4342076033098,63.9031301713382));
#25013=CARTESIAN_POINT('Ctrl Pts',(2.26152784238033,-6.38028870334086,63.9113534171731));
#25014=CARTESIAN_POINT('Ctrl Pts',(2.42516834089234,-6.31991201723672,63.9195766630079));
#25015=CARTESIAN_POINT('Ctrl Pts',(2.58639362657619,-6.25322772721465,63.9277999088428));
#25016=CARTESIAN_POINT('Ctrl Pts',(2.74745918731633,-6.18660950092709,63.9360150079563));
#25017=CARTESIAN_POINT('Ctrl Pts',(2.90611397168133,-6.11369625145372,63.9442301070697));
#25018=CARTESIAN_POINT('Ctrl Pts',(3.06183469079249,-6.03468784000131,63.9524452061832));
#25019=CARTESIAN_POINT('Ctrl Pts',(3.21743229488071,-5.95574189372658,63.9606538103221));
#25020=CARTESIAN_POINT('Ctrl Pts',(3.37010013613797,-5.87071054513674,63.968862414461));
#25021=CARTESIAN_POINT('Ctrl Pts',(3.51933510274833,-5.77984164441928,63.9770710185999));
#25022=CARTESIAN_POINT('Ctrl Pts',(3.6684819332182,-5.68902640963805,63.9852747748489));
#25023=CARTESIAN_POINT('Ctrl Pts',(3.81419962280484,-5.59238067655634,63.9934785310979));
#25024=CARTESIAN_POINT('Ctrl Pts',(3.95600978636036,-5.49019813578901,64.0016822873468));
#25025=CARTESIAN_POINT('Ctrl Pts',(4.09777799186268,-5.38804582826007,64.0098836163111));
#25026=CARTESIAN_POINT('Ctrl Pts',(4.23564068183212,-5.28036018228064,64.0180849452754));
#25027=CARTESIAN_POINT('Ctrl Pts',(4.36914838749145,-5.16747824069738,64.0262862742397));
#25028=CARTESIAN_POINT('Ctrl Pts',(4.50263768116362,-5.05461186661151,64.0344864721624));
#25029=CARTESIAN_POINT('Ctrl Pts',(4.63177291268134,-4.93655085481184,64.0426866700851));
#25030=CARTESIAN_POINT('Ctrl Pts',(4.75613764415157,-4.8136725802535,64.0508868680079));
#25031=CARTESIAN_POINT('Ctrl Pts',(4.88050776195783,-4.69078898373876,64.0590874210877));
#25032=CARTESIAN_POINT('Ctrl Pts',(5.00010671317036,-4.5630879605937,64.0672879741675));
#25033=CARTESIAN_POINT('Ctrl Pts',(5.11455485263038,-4.43098382522832,64.0754885272474));
#25034=CARTESIAN_POINT('Ctrl Pts',(5.22902868917564,-4.29885002847009,64.0836909216006));
#25035=CARTESIAN_POINT('Ctrl Pts',(5.3383491759655,-4.16231142115327,64.0918933159538));
#25036=CARTESIAN_POINT('Ctrl Pts',(5.44217686535818,-4.02181550623102,64.100095710307));
#25037=CARTESIAN_POINT('Ctrl Pts',(5.54610165189218,-3.88118820293071,64.1083057753409));
#25038=CARTESIAN_POINT('Ctrl Pts',(5.64452316505465,-3.73659648669212,64.1165158403747));
#25039=CARTESIAN_POINT('Ctrl Pts',(5.73714470946154,-3.58851774172812,64.1247259054086));
#25040=CARTESIAN_POINT('Ctrl Pts',(5.82981058089664,-3.44036812890343,64.1329398996339));
#25041=CARTESIAN_POINT('Ctrl Pts',(5.91667077117707,-3.28872847070018,64.1411538938592));
#25042=CARTESIAN_POINT('Ctrl Pts',(5.99747456463078,-3.13410080351715,64.1493678880845));
#25043=CARTESIAN_POINT('Ctrl Pts',(6.0783885205673,-2.9792623273238,64.1575930807197));
#25044=CARTESIAN_POINT('Ctrl Pts',(6.15322942463203,-2.82142802472799,64.1658182733549));
#25045=CARTESIAN_POINT('Ctrl Pts',(6.22179424272042,-2.6611210797803,64.1740434659901));
#25046=CARTESIAN_POINT('Ctrl Pts',(6.28345443677379,-2.51695738753749,64.18144036411));
#25047=CARTESIAN_POINT('Ctrl Pts',(6.34003952089641,-2.37079440267211,64.18883726223));
#25048=CARTESIAN_POINT('Ctrl Pts',(6.39143650395114,-2.22302236065245,64.1962341603499));
#25049=CARTESIAN_POINT('Ctrl Pts',(6.45151257719412,-2.05029696916043,64.2048801268408));
#25050=CARTESIAN_POINT('Ctrl Pts',(6.50463635311451,-1.8749810263893,64.2135260933317));
#25051=CARTESIAN_POINT('Ctrl Pts',(6.55059377604674,-1.69764842685927,64.2221720598226));
#25052=CARTESIAN_POINT('Ctrl Pts',(6.59649241318722,-1.52054265983203,64.230806966947));
#25053=CARTESIAN_POINT('Ctrl Pts',(6.63524290022221,-1.34142567366235,64.2394418740713));
#25054=CARTESIAN_POINT('Ctrl Pts',(6.66668044306123,-1.16088796621593,64.2480767811957));
#25055=CARTESIAN_POINT('Ctrl Pts',(6.69916168694868,-0.97435655259756,64.2569983602672));
#25056=CARTESIAN_POINT('Ctrl Pts',(6.72383594159697,-0.786308756225134,
64.2659199393387));
#25057=CARTESIAN_POINT('Ctrl Pts',(6.74057770307013,-0.597412109748195,
64.2748415184102));
#25058=CARTESIAN_POINT('Ctrl Pts',(6.75673675902284,-0.415090107096774,
64.2834525773859));
#25059=CARTESIAN_POINT('Ctrl Pts',(6.76550613345692,-0.231977688015453,
64.2920636363616));
#25060=CARTESIAN_POINT('Ctrl Pts',(6.76682486511335,-0.0486851608162831,
64.3006746953373));
#25061=CARTESIAN_POINT('Ctrl Pts',(6.76814235314494,0.134434513067053,64.3092776336868));
#25062=CARTESIAN_POINT('Ctrl Pts',(6.76202320481354,0.317733652485977,64.3178805720363));
#25063=CARTESIAN_POINT('Ctrl Pts',(6.74845836533785,0.500598333298885,64.3264835103859));
#25064=CARTESIAN_POINT('Ctrl Pts',(6.73490871534439,0.683258247971745,64.3350768154346));
#25065=CARTESIAN_POINT('Ctrl Pts',(6.71393002970185,0.865484371104247,64.3436701204833));
#25066=CARTESIAN_POINT('Ctrl Pts',(6.68556529626049,1.04666406713776,64.352263425532));
#25067=CARTESIAN_POINT('Ctrl Pts',(6.68240500067162,1.06685045088618,64.3532208603725));
#25068=CARTESIAN_POINT('Ctrl Pts',(6.6791530708192,1.08702384669509,64.3541782952131));
#25069=CARTESIAN_POINT('Ctrl Pts',(6.67580960620645,1.10718340923342,64.3551357300536));
#25070=CARTESIAN_POINT('Ctrl Pts',(6.64579230376101,1.28817401507749,64.3637314876012));
#25071=CARTESIAN_POINT('Ctrl Pts',(6.60842798813331,1.46783697545944,64.3723272451488));
#25072=CARTESIAN_POINT('Ctrl Pts',(6.5638683233526,1.64557638342566,64.3809230026964));
#25073=CARTESIAN_POINT('Ctrl Pts',(6.51926708288994,1.82348162830142,64.389526780378));
#25074=CARTESIAN_POINT('Ctrl Pts',(6.46745716711604,1.99945944225569,64.3981305580596));
#25075=CARTESIAN_POINT('Ctrl Pts',(6.40864002585188,2.17292936356644,64.4067343357411));
#25076=CARTESIAN_POINT('Ctrl Pts',(6.34751131950341,2.3532168044754,64.4156762494092));
#25077=CARTESIAN_POINT('Ctrl Pts',(6.2788136026702,2.53079488917563,64.4246181630772));
#25078=CARTESIAN_POINT('Ctrl Pts',(6.20282733183092,2.70503643071425,64.4335600767453));
#25079=CARTESIAN_POINT('Ctrl Pts',(6.12951540362112,2.87314552783606,64.442187279076));
#25080=CARTESIAN_POINT('Ctrl Pts',(6.04941939341233,3.0381486933052,64.4508144814067));
#25081=CARTESIAN_POINT('Ctrl Pts',(5.96283762682577,3.19950878043972,64.4594416837375));
#25082=CARTESIAN_POINT('Ctrl Pts',(5.87617340435945,3.36102253835813,64.4680771021579));
#25083=CARTESIAN_POINT('Ctrl Pts',(5.78301124854136,3.51888602852593,64.4767125205783));
#25084=CARTESIAN_POINT('Ctrl Pts',(5.68369340940687,3.67259012522021,64.4853479389987));
#25085=CARTESIAN_POINT('Ctrl Pts',(5.58422884231159,3.82652129782419,64.4939961150199));
#25086=CARTESIAN_POINT('Ctrl Pts',(5.47859059093992,3.97628054571561,64.502644291041));
#25087=CARTESIAN_POINT('Ctrl Pts',(5.36716272913405,4.12138972180433,64.5112924670621));
#25088=CARTESIAN_POINT('Ctrl Pts',(5.35537408385509,4.13674172242525,64.512207411294));
#25089=CARTESIAN_POINT('Ctrl Pts',(5.34352067183579,4.15204170803573,64.5131223555258));
#25090=CARTESIAN_POINT('Ctrl Pts',(5.33160297273055,4.16728913577769,64.5140372997576));
#25091=CARTESIAN_POINT('Ctrl Pts',(5.22444543830568,4.30438579753439,64.5222639857271));
#25092=CARTESIAN_POINT('Ctrl Pts',(5.11185590415505,4.43752659099536,64.5304906716966));
#25093=CARTESIAN_POINT('Ctrl Pts',(4.99415701639361,4.56625499677871,64.5387173576661));
#25094=CARTESIAN_POINT('Ctrl Pts',(4.87657886026313,4.69485135721585,64.5469356049729));
#25095=CARTESIAN_POINT('Ctrl Pts',(4.753902026276,4.81904407991842,64.5551538522797));
#25096=CARTESIAN_POINT('Ctrl Pts',(4.62649081119084,4.93840781770468,64.5633720995865));
#25097=CARTESIAN_POINT('Ctrl Pts',(4.49920926513555,5.05765007654524,64.571581983013));
#25098=CARTESIAN_POINT('Ctrl Pts',(4.36720320055242,5.172072901194,64.5797918664394));
#25099=CARTESIAN_POINT('Ctrl Pts',(4.23087515662351,5.28128624570435,64.5880017498659));
#25100=CARTESIAN_POINT('Ctrl Pts',(4.09462761950288,5.39043509565046,64.5962067850492));
#25101=CARTESIAN_POINT('Ctrl Pts',(3.95406346356247,5.49438036780918,64.6044118202325));
#25102=CARTESIAN_POINT('Ctrl Pts',(3.80962018394378,5.5927706062459,64.6126168554158));
#25103=CARTESIAN_POINT('Ctrl Pts',(3.66523880839847,5.69111867756653,64.6208183741661));
#25104=CARTESIAN_POINT('Ctrl Pts',(3.5169819162023,5.78391625608548,64.6290198929165));
#25105=CARTESIAN_POINT('Ctrl Pts',(3.36531803745911,5.87085372895224,64.6372214116669));
#25106=CARTESIAN_POINT('Ctrl Pts',(3.27770872470274,5.92107354604876,64.6419590553777));
#25107=CARTESIAN_POINT('Ctrl Pts',(3.18896311695826,5.96933872150464,64.6466966990885));
#25108=CARTESIAN_POINT('Ctrl Pts',(3.09917575053261,6.01559628526638,64.6514343427993));
#25109=CARTESIAN_POINT('Origin',(0.,0.,-3.69717978381041));
#25110=CARTESIAN_POINT('',(3.09917575053263,6.01559628526637,67.0455611218465));
#25111=CARTESIAN_POINT('',(3.09917575053252,6.01559628526643,66.6513920151221));
#25112=CARTESIAN_POINT('',(3.09917575053259,6.01559628526639,-3.69717978381041));
#25113=CARTESIAN_POINT('',(-6.76699996591071,0.000679238137944715,65.6971797933975));
#25114=CARTESIAN_POINT('Ctrl Pts',(-6.76699996593128,0.000679033234083034,
65.6971798029849));
#25115=CARTESIAN_POINT('Ctrl Pts',(-6.76701829841272,-0.182015855690237,
65.7057280919095));
#25116=CARTESIAN_POINT('Ctrl Pts',(-6.75963373113655,-0.364585292346518,
65.7142763808342));
#25117=CARTESIAN_POINT('Ctrl Pts',(-6.74490266290975,-0.546422060199833,
65.7228246697588));
#25118=CARTESIAN_POINT('Ctrl Pts',(-6.73015592228546,-0.72845228436326,
65.7313820532162));
#25119=CARTESIAN_POINT('Ctrl Pts',(-6.70804710543446,-0.909747974781611,
65.7399394366735));
#25120=CARTESIAN_POINT('Ctrl Pts',(-6.67868416120356,-1.08970953693578,
65.7484968201309));
#25121=CARTESIAN_POINT('Ctrl Pts',(-6.64926242066203,-1.27003145382223,
65.7570713388786));
#25122=CARTESIAN_POINT('Ctrl Pts',(-6.6125575580926,-1.44901359345539,65.7656458576263));
#25123=CARTESIAN_POINT('Ctrl Pts',(-6.56872859973054,-1.62606690609029,
65.774220376374));
#25124=CARTESIAN_POINT('Ctrl Pts',(-6.52485489609184,-1.80330097363587,
65.7828036489053));
#25125=CARTESIAN_POINT('Ctrl Pts',(-6.47384266484309,-1.97860198551847,
65.7913869214366));
#25126=CARTESIAN_POINT('Ctrl Pts',(-6.41590032842197,-2.15139767959224,
65.7999701939678));
#25127=CARTESIAN_POINT('Ctrl Pts',(-6.35783972036346,-2.32454608346221,
65.8085709866365));
#25128=CARTESIAN_POINT('Ctrl Pts',(-6.29282082746695,-2.49517865135353,
65.8171717793051));
#25129=CARTESIAN_POINT('Ctrl Pts',(-6.22110047482245,-2.6627425489829,65.8257725719738));
#25130=CARTESIAN_POINT('Ctrl Pts',(-6.15407454921833,-2.8193386186106,65.8338104031931));
#25131=CARTESIAN_POINT('Ctrl Pts',(-6.08119628993791,-2.97325463338034,
65.8418482344124));
#25132=CARTESIAN_POINT('Ctrl Pts',(-6.00271060372069,-3.12406056407029,
65.8498860656317));
#25133=CARTESIAN_POINT('Ctrl Pts',(-5.91828918509872,-3.28627167821175,
65.8585317836841));
#25134=CARTESIAN_POINT('Ctrl Pts',(-5.82721329346294,-3.44520389241049,
65.8671775017364));
#25135=CARTESIAN_POINT('Ctrl Pts',(-5.72975335653186,-3.60030769147747,
65.8758232197888));
#25136=CARTESIAN_POINT('Ctrl Pts',(-5.63241853829777,-3.75521236887612,
65.8844578385011));
#25137=CARTESIAN_POINT('Ctrl Pts',(-5.52871617912909,-3.90629817472001,
65.8930924572134));
#25138=CARTESIAN_POINT('Ctrl Pts',(-5.41896259311802,-4.05304002131581,
65.9017270759257));
#25139=CARTESIAN_POINT('Ctrl Pts',(-5.3053329368074,-4.20496421988718,65.9106666358282));
#25140=CARTESIAN_POINT('Ctrl Pts',(-5.18521696388412,-4.35223173770641,
65.9196061957307));
#25141=CARTESIAN_POINT('Ctrl Pts',(-5.05901649420365,-4.49428983393098,
65.9285457556331));
#25142=CARTESIAN_POINT('Ctrl Pts',(-4.9374592252949,-4.63112129142999,65.9371564089036));
#25143=CARTESIAN_POINT('Ctrl Pts',(-4.81025739461192,-4.76311953171593,
65.945767062174));
#25144=CARTESIAN_POINT('Ctrl Pts',(-4.6778130723278,-4.88982145485488,65.9543777154445));
#25145=CARTESIAN_POINT('Ctrl Pts',(-4.54549411745622,-5.0164034461463,65.9629802181555));
#25146=CARTESIAN_POINT('Ctrl Pts',(-4.40794278427344,-5.13769890536457,
65.9715827208666));
#25147=CARTESIAN_POINT('Ctrl Pts',(-4.26559939339094,-5.2532800053969,65.9801852235776));
#25148=CARTESIAN_POINT('Ctrl Pts',(-4.1234162071291,-5.36873102122812,65.988778044345));
#25149=CARTESIAN_POINT('Ctrl Pts',(-3.97645195903324,-5.47848031647352,
65.9973708651125));
#25150=CARTESIAN_POINT('Ctrl Pts',(-3.82518174281441,-5.58213880465537,
66.0059636858799));
#25151=CARTESIAN_POINT('Ctrl Pts',(-3.80735386072118,-5.59435542833359,
66.0069763888383));
#25152=CARTESIAN_POINT('Ctrl Pts',(-3.78946620925084,-5.60648749735201,
66.0079890917968));
#25153=CARTESIAN_POINT('Ctrl Pts',(-3.77151959710279,-5.61853441109597,
66.0090017947552));
#25154=CARTESIAN_POINT('Ctrl Pts',(-3.61919876497134,-5.72078189440697,
66.0175970525153));
#25155=CARTESIAN_POINT('Ctrl Pts',(-3.4628073215774,-5.81677131581846,66.0261923102754));
#25156=CARTESIAN_POINT('Ctrl Pts',(-3.30288303748162,-5.90620458845748,
66.0347875680355));
#25157=CARTESIAN_POINT('Ctrl Pts',(-3.14280899107559,-5.99572161156379,
66.04339087489));
#25158=CARTESIAN_POINT('Ctrl Pts',(-2.97919576686916,-6.07867008207256,
66.0519941817445));
#25159=CARTESIAN_POINT('Ctrl Pts',(-2.81260401966386,-6.1547987480153,66.060597488599));
#25160=CARTESIAN_POINT('Ctrl Pts',(-2.63910532085218,-6.23408373484635,
66.0695574915389));
#25161=CARTESIAN_POINT('Ctrl Pts',(-2.4623762072421,-6.30597121789813,66.0785174944789));
#25162=CARTESIAN_POINT('Ctrl Pts',(-2.28306956927753,-6.3702340884648,66.0874774974189));
#25163=CARTESIAN_POINT('Ctrl Pts',(-2.11043008894921,-6.43210747310339,
66.0961043406236));
#25164=CARTESIAN_POINT('Ctrl Pts',(-1.93540160429527,-6.48691298856344,
66.1047311838284));
#25165=CARTESIAN_POINT('Ctrl Pts',(-1.7585796753181,-6.53449971501707,66.1133580270332));
#25166=CARTESIAN_POINT('Ctrl Pts',(-1.58158874927383,-6.58213192235222,
66.1219931153193));
#25167=CARTESIAN_POINT('Ctrl Pts',(-1.40280125409471,-6.62253149882609,
66.1306282036055));
#25168=CARTESIAN_POINT('Ctrl Pts',(-1.22282244806186,-6.65559871540615,
66.1392632918917));
#25169=CARTESIAN_POINT('Ctrl Pts',(-1.04257633738337,-6.68871504343887,
66.1479112050169));
#25170=CARTESIAN_POINT('Ctrl Pts',(-0.861135681401127,-6.71447720235611,
66.1565591181421));
#25171=CARTESIAN_POINT('Ctrl Pts',(-0.679111850412633,-6.7328371504611,
66.1652070312673));
#25172=CARTESIAN_POINT('Ctrl Pts',(-0.658691547561236,-6.73489685714129,
66.166177195471));
#25173=CARTESIAN_POINT('Ctrl Pts',(-0.638263905900065,-6.73686345783071,
66.1671473596747));
#25174=CARTESIAN_POINT('Ctrl Pts',(-0.617829788642748,-6.7387369255867,
66.1681175238785));
#25175=CARTESIAN_POINT('Ctrl Pts',(-0.444597190442899,-6.75461946569974,
66.1763422033973));
#25176=CARTESIAN_POINT('Ctrl Pts',(-0.270523469771335,-6.76383871484805,
66.184566882916));
#25177=CARTESIAN_POINT('Ctrl Pts',(-0.0961618693914154,-6.76631671553107,
66.1927915624348));
#25178=CARTESIAN_POINT('Ctrl Pts',(0.0780164572205188,-6.76879211155503,
66.201007596885));
#25179=CARTESIAN_POINT('Ctrl Pts',(0.252481705538154,-6.76454036442842,
66.2092236313352));
#25180=CARTESIAN_POINT('Ctrl Pts',(0.426674816227314,-6.75353519285991,
66.2174396657853));
#25181=CARTESIAN_POINT('Ctrl Pts',(0.600719721436524,-6.74253938461656,
66.2256487099399));
#25182=CARTESIAN_POINT('Ctrl Pts',(0.774492594459042,-6.72480161802293,
66.2338577540945));
#25183=CARTESIAN_POINT('Ctrl Pts',(0.947433578676589,-6.70034764874153,
66.242066798249));
#25184=CARTESIAN_POINT('Ctrl Pts',(1.1202620533378,-6.67590958838562,66.2502705018771));
#25185=CARTESIAN_POINT('Ctrl Pts',(1.29225936359367,-6.64476407866937,66.2584742055051));
#25186=CARTESIAN_POINT('Ctrl Pts',(1.46286988650982,-6.60698877667752,66.2666779091332));
#25187=CARTESIAN_POINT('Ctrl Pts',(1.63340357297601,-6.56923048723597,66.2748779181271));
#25188=CARTESIAN_POINT('Ctrl Pts',(1.80255136717255,-6.52484843138451,66.283077927121));
#25189=CARTESIAN_POINT('Ctrl Pts',(1.96976687326738,-6.47397153723883,66.2912779361149));
#25190=CARTESIAN_POINT('Ctrl Pts',(2.13696900845895,-6.42309871131652,66.2994772894188));
#25191=CARTESIAN_POINT('Ctrl Pts',(2.30223881813281,-6.36573217743598,66.3076766427228));
#25192=CARTESIAN_POINT('Ctrl Pts',(2.46504377013428,-6.30205111144953,66.3158759960267));
#25193=CARTESIAN_POINT('Ctrl Pts',(2.62784766069578,-6.23837046064472,66.3240752958733));
#25194=CARTESIAN_POINT('Ctrl Pts',(2.78818639131588,-6.16837548932268,66.3322745957199));
#25195=CARTESIAN_POINT('Ctrl Pts',(2.94554628395755,-6.09229399233687,66.3404738955665));
#25196=CARTESIAN_POINT('Ctrl Pts',(3.10293369728779,-6.01619918944986,66.3486746293895));
#25197=CARTESIAN_POINT('Ctrl Pts',(3.25734091191964,-5.93401589617232,66.3568753632126));
#25198=CARTESIAN_POINT('Ctrl Pts',(3.4082777346436,-5.84601846417993,66.3650760970356));
#25199=CARTESIAN_POINT('Ctrl Pts',(3.55926833644244,-5.7579896785364,66.3732797527956));
#25200=CARTESIAN_POINT('Ctrl Pts',(3.70678577361999,-5.66414280792534,66.3814834085556));
#25201=CARTESIAN_POINT('Ctrl Pts',(3.8503677394768,-5.56479624701537,66.3896870643155));
#25202=CARTESIAN_POINT('Ctrl Pts',(3.99411418770588,-5.46533587823322,66.3979001178906));
#25203=CARTESIAN_POINT('Ctrl Pts',(4.13391586253542,-5.36036343644528,66.4061131714656));
#25204=CARTESIAN_POINT('Ctrl Pts',(4.2693416978793,-5.2502390866273,66.4143262250406));
#25205=CARTESIAN_POINT('Ctrl Pts',(4.40484766772839,-5.14004957376077,66.4225441384637));
#25206=CARTESIAN_POINT('Ctrl Pts',(4.53597236794302,-5.02470231247019,66.4307620518868));
#25207=CARTESIAN_POINT('Ctrl Pts',(4.66232079823274,-4.90459516926387,66.4389799653099));
#25208=CARTESIAN_POINT('Ctrl Pts',(4.78886628945417,-4.78430069942839,66.4472106959059));
#25209=CARTESIAN_POINT('Ctrl Pts',(4.91062037379979,-4.6592317684667,66.4554414265019));
#25210=CARTESIAN_POINT('Ctrl Pts',(5.02722672795302,-4.52982123551855,66.4636721570979));
#25211=CARTESIAN_POINT('Ctrl Pts',(5.1343157183893,-4.41097313820966,66.4712310987738));
#25212=CARTESIAN_POINT('Ctrl Pts',(5.23706333941518,-4.28846378288316,66.4787900404496));
#25213=CARTESIAN_POINT('Ctrl Pts',(5.3352258976235,-4.16264983169706,66.4863489821254));
#25214=CARTESIAN_POINT('Ctrl Pts',(5.4411146514679,-4.02693329424635,66.4945028742922));
#25215=CARTESIAN_POINT('Ctrl Pts',(5.54199497742943,-3.88695143604734,66.5026567664589));
#25216=CARTESIAN_POINT('Ctrl Pts',(5.63749939601689,-3.74311228256771,66.5108106586256));
#25217=CARTESIAN_POINT('Ctrl Pts',(5.73288727253146,-3.59944865304139,66.5189546007658));
#25218=CARTESIAN_POINT('Ctrl Pts',(5.82291209971961,-3.45193739885122,66.527098542906));
#25219=CARTESIAN_POINT('Ctrl Pts',(5.90724584281413,-3.30102038051194,66.5352424850462));
#25220=CARTESIAN_POINT('Ctrl Pts',(5.99149442575089,-3.15025575807753,66.5433782034391));
#25221=CARTESIAN_POINT('Ctrl Pts',(6.07006318842045,-2.99609253493669,66.5515139218319));
#25222=CARTESIAN_POINT('Ctrl Pts',(6.14266672326913,-2.83900238232413,66.5596496402248));
#25223=CARTESIAN_POINT('Ctrl Pts',(6.2152122152883,-2.68203781529036,66.567778854525));
#25224=CARTESIAN_POINT('Ctrl Pts',(6.28180182217059,-2.52215130819603,66.5759080688252));
#25225=CARTESIAN_POINT('Ctrl Pts',(6.34219552603449,-2.35984001778683,66.5840372831254));
#25226=CARTESIAN_POINT('Ctrl Pts',(6.40255364673221,-2.19762435902875,66.5921617078008));
#25227=CARTESIAN_POINT('Ctrl Pts',(6.45672300712941,-2.03298710389042,66.6002861324763));
#25228=CARTESIAN_POINT('Ctrl Pts',(6.50451129305998,-1.86644631277065,66.6084105571517));
#25229=CARTESIAN_POINT('Ctrl Pts',(6.55258968447877,-1.69889451243442,66.6165843022858));
#25230=CARTESIAN_POINT('Ctrl Pts',(6.5942091160322,-1.52941632984027,66.62475804742));
#25231=CARTESIAN_POINT('Ctrl Pts',(6.62922420344981,-1.35855638837528,66.6329317925542));
#25232=CARTESIAN_POINT('Ctrl Pts',(6.66401506449367,-1.18879058397854,66.6410531954163));
#25233=CARTESIAN_POINT('Ctrl Pts',(6.69228586697066,-1.01766103306341,66.6491745982785));
#25234=CARTESIAN_POINT('Ctrl Pts',(6.7139450268928,-0.845713412369381,66.6572960011407));
#25235=CARTESIAN_POINT('Ctrl Pts',(6.73560586138712,-0.673752497590899,
66.6654180319069));
#25236=CARTESIAN_POINT('Ctrl Pts',(6.75065398932149,-0.500973750163868,
66.6735400626732));
#25237=CARTESIAN_POINT('Ctrl Pts',(6.75904960699328,-0.327928971278944,
66.6816620934394));
#25238=CARTESIAN_POINT('Ctrl Pts',(6.7674474724895,-0.154837861760821,66.6897862987805));
#25239=CARTESIAN_POINT('Ctrl Pts',(6.7691892634495,0.018519055636335,66.6979105041216));
#25240=CARTESIAN_POINT('Ctrl Pts',(6.76428729798188,0.191589014197034,66.7060347094628));
#25241=CARTESIAN_POINT('Ctrl Pts',(6.75933227212995,0.366532335304846,66.7142468537052));
#25242=CARTESIAN_POINT('Ctrl Pts',(6.74758883146797,0.541182065489069,66.7224589979477));
#25243=CARTESIAN_POINT('Ctrl Pts',(6.72912352322345,0.714972453455995,66.7306711421901));
#25244=CARTESIAN_POINT('Ctrl Pts',(6.71082678289187,0.887176326721829,66.7388083186066));
#25245=CARTESIAN_POINT('Ctrl Pts',(6.68593050572258,1.0585361294244,66.746945495023));
#25246=CARTESIAN_POINT('Ctrl Pts',(6.65455087594178,1.22851196148125,66.7550826714394));
#25247=CARTESIAN_POINT('Ctrl Pts',(6.62273759525332,1.40083677516617,66.7633322995949));
#25248=CARTESIAN_POINT('Ctrl Pts',(6.58426054248535,1.57173870365354,66.7715819277504));
#25249=CARTESIAN_POINT('Ctrl Pts',(6.53929285886129,1.74067168243922,66.7798315559058));
#25250=CARTESIAN_POINT('Ctrl Pts',(6.49432517523723,1.9096046612249,66.7880811840613));
#25251=CARTESIAN_POINT('Ctrl Pts',(6.44286703453955,2.07656834123183,66.7963308122168));
#25252=CARTESIAN_POINT('Ctrl Pts',(6.3851417130851,2.24103866629308,66.8045804403722));
#25253=CARTESIAN_POINT('Ctrl Pts',(6.32757961941145,2.40504392462987,66.8128067413558));
#25254=CARTESIAN_POINT('Ctrl Pts',(6.2636138135267,2.56706028210118,66.8210330423394));
#25255=CARTESIAN_POINT('Ctrl Pts',(6.19340007997293,2.7265517507268,66.8292593433229));
#25256=CARTESIAN_POINT('Ctrl Pts',(6.1232678698591,2.885858037729,66.8374760929507));
#25257=CARTESIAN_POINT('Ctrl Pts',(6.04690232226855,3.0426449484445,66.8456928425784));
#25258=CARTESIAN_POINT('Ctrl Pts',(5.9645087528244,3.19639239416582,66.8539095922061));
#25259=CARTESIAN_POINT('Ctrl Pts',(5.88221116536148,3.34996073629267,66.8621167699715));
#25260=CARTESIAN_POINT('Ctrl Pts',(5.7938997203715,3.50049635610298,66.8703239477368));
#25261=CARTESIAN_POINT('Ctrl Pts',(5.69982736677687,3.64750010129424,66.8785311255021));
#25262=CARTESIAN_POINT('Ctrl Pts',(5.60581794891072,3.79440549891113,66.88673281255));
#25263=CARTESIAN_POINT('Ctrl Pts',(5.50605548906791,3.93778342587172,66.894934499598));
#25264=CARTESIAN_POINT('Ctrl Pts',(5.40083858019566,4.07715975044763,66.9031361866459));
#25265=CARTESIAN_POINT('Ctrl Pts',(5.29567291839555,4.21646819022595,66.9113338789704));
#25266=CARTESIAN_POINT('Ctrl Pts',(5.18505831402604,4.35177862356726,66.9195315712949));
#25267=CARTESIAN_POINT('Ctrl Pts',(5.06933638185038,4.48264627732861,66.9277292636194));
#25268=CARTESIAN_POINT('Ctrl Pts',(4.95364975869858,4.61347400081037,66.9359244546677));
#25269=CARTESIAN_POINT('Ctrl Pts',(4.8328591496575,4.73986137687093,66.944119645716));
#25270=CARTESIAN_POINT('Ctrl Pts',(4.70734614836208,4.86139704606615,66.9523148367643));
#25271=CARTESIAN_POINT('Ctrl Pts',(4.58182083059437,4.98294464144183,66.960510831999));
#25272=CARTESIAN_POINT('Ctrl Pts',(4.45157244688807,5.09963932339206,66.9687068272336));
#25273=CARTESIAN_POINT('Ctrl Pts',(4.31701941844626,5.21110663302508,66.9769028224683));
#25274=CARTESIAN_POINT('Ctrl Pts',(4.18246280969302,5.32257690868336,66.9850990357896));
#25275=CARTESIAN_POINT('Ctrl Pts',(4.0436016075609,5.42881930982883,66.9932952491109));
#25276=CARTESIAN_POINT('Ctrl Pts',(3.90088697555653,5.52949995966484,67.0014914624322));
#25277=CARTESIAN_POINT('Ctrl Pts',(3.75808854046217,5.63023972992486,67.0096924886307));
#25278=CARTESIAN_POINT('Ctrl Pts',(3.61143245004889,5.72541101959315,67.0178935148293));
#25279=CARTESIAN_POINT('Ctrl Pts',(3.46139904487163,5.81472317932348,67.0260945410278));
#25280=CARTESIAN_POINT('Ctrl Pts',(3.34268880314117,5.88538922905108,67.0325834013007));
#25281=CARTESIAN_POINT('Ctrl Pts',(3.22186484807763,5.95238807481889,67.0390722615736));
#25282=CARTESIAN_POINT('Ctrl Pts',(3.09917575053264,6.01559628526636,67.0455611218465));
#25283=CARTESIAN_POINT('Ctrl Pts',(3.09917575053256,6.01559628526641,65.0457972463573));
#25284=CARTESIAN_POINT('Ctrl Pts',(2.94385221859564,6.09561743376751,65.0539928534118));
#25285=CARTESIAN_POINT('Ctrl Pts',(2.78541612683539,6.16962484631762,65.0621884604664));
#25286=CARTESIAN_POINT('Ctrl Pts',(2.62437670962481,6.23738213403499,65.0703840675209));
#25287=CARTESIAN_POINT('Ctrl Pts',(2.46331642498624,6.30514820171659,65.0785807365591));
#25288=CARTESIAN_POINT('Ctrl Pts',(2.29965247367174,6.36666239194464,65.0867774055974));
#25289=CARTESIAN_POINT('Ctrl Pts',(2.13391369978768,6.42173662819167,65.0949740746356));
#25290=CARTESIAN_POINT('Ctrl Pts',(1.96812329517018,6.47682802109519,65.1031732970898));
#25291=CARTESIAN_POINT('Ctrl Pts',(1.80025712095075,6.5254753508844,65.1113725195441));
#25292=CARTESIAN_POINT('Ctrl Pts',(1.6308588379582,6.56754051762558,65.1195717419983));
#25293=CARTESIAN_POINT('Ctrl Pts',(1.46128209771362,6.60964999906659,65.1277796021476));
#25294=CARTESIAN_POINT('Ctrl Pts',(1.29017037295865,6.64516337844948,65.1359874622968));
#25295=CARTESIAN_POINT('Ctrl Pts',(1.11807813852233,6.67399357777324,65.1441953224461));
#25296=CARTESIAN_POINT('Ctrl Pts',(0.94589038704666,6.70283977883754,65.1524077382367));
#25297=CARTESIAN_POINT('Ctrl Pts',(0.772721396489648,6.72499535991473,65.1606201540273));
#25298=CARTESIAN_POINT('Ctrl Pts',(0.59913030369686,6.74042520017781,65.1688325698179));
#25299=CARTESIAN_POINT('Ctrl Pts',(0.425289102472883,6.75587727161117,65.1770568179808));
#25300=CARTESIAN_POINT('Ctrl Pts',(0.251024941923443,6.76458422105991,65.1852810661437));
#25301=CARTESIAN_POINT('Ctrl Pts',(0.0768977199021893,6.76656306707281,
65.1935053143066));
#25302=CARTESIAN_POINT('Ctrl Pts',(-0.0636718567609128,6.76816055161938,
65.2001445925837));
#25303=CARTESIAN_POINT('Ctrl Pts',(-0.204152146911855,6.76537432336689,
65.2067838708609));
#25304=CARTESIAN_POINT('Ctrl Pts',(-0.34425177587415,6.75823791493075,65.2134231491381));
#25305=CARTESIAN_POINT('Ctrl Pts',(-0.516250829178352,6.74947661053544,
65.2215741313123));
#25306=CARTESIAN_POINT('Ctrl Pts',(-0.688185389881194,6.73413111849514,
65.2297251134866));
#25307=CARTESIAN_POINT('Ctrl Pts',(-0.859506089281795,6.71219325425658,
65.2378760956609));
#25308=CARTESIAN_POINT('Ctrl Pts',(-1.0306277838118,6.69028087288057,65.2460176097139));
#25309=CARTESIAN_POINT('Ctrl Pts',(-1.20113667741297,6.66179140841808,65.254159123767));
#25310=CARTESIAN_POINT('Ctrl Pts',(-1.37048393519505,6.62676865322551,65.26230063782));
#25311=CARTESIAN_POINT('Ctrl Pts',(-1.53967011731522,6.59177921013702,65.270434408023));
#25312=CARTESIAN_POINT('Ctrl Pts',(-1.70769650764706,6.55026892138597,65.278568178226));
#25313=CARTESIAN_POINT('Ctrl Pts',(-1.87401992936699,6.50233329692775,65.286701948429));
#25314=CARTESIAN_POINT('Ctrl Pts',(-2.04022013280626,6.45443318487764,65.2948296928471));
#25315=CARTESIAN_POINT('Ctrl Pts',(-2.20471952979505,6.40011731610231,65.3029574372651));
#25316=CARTESIAN_POINT('Ctrl Pts',(-2.3669856751762,6.33953214468629,65.3110851816831));
#25317=CARTESIAN_POINT('Ctrl Pts',(-2.52916572328387,6.27897911933535,65.3192086135772));
#25318=CARTESIAN_POINT('Ctrl Pts',(-2.68911453778835,6.21216354366818,65.3273320454713));
#25319=CARTESIAN_POINT('Ctrl Pts',(-2.84631537619127,6.13928153608036,65.3354554773654));
#25320=CARTESIAN_POINT('Ctrl Pts',(-3.00451343488078,6.06593719370327,65.3436304411162));
#25321=CARTESIAN_POINT('Ctrl Pts',(-3.15992817398629,5.9864492971089,65.351805404867));
#25322=CARTESIAN_POINT('Ctrl Pts',(-3.31205345963695,5.9010669273028,65.3599803686178));
#25323=CARTESIAN_POINT('Ctrl Pts',(-3.46318551484137,5.81624202149028,65.3681019577908));
#25324=CARTESIAN_POINT('Ctrl Pts',(-3.61107063285668,5.72559958800872,65.3762235469639));
#25325=CARTESIAN_POINT('Ctrl Pts',(-3.7552376238199,5.62942975696895,65.3843451361369));
#25326=CARTESIAN_POINT('Ctrl Pts',(-3.8994236477821,5.5332472295395,65.3924677975262));
#25327=CARTESIAN_POINT('Ctrl Pts',(-4.03989026247573,5.43153605417728,65.4005904589155));
#25328=CARTESIAN_POINT('Ctrl Pts',(-4.17619579140123,5.32462934971841,65.4087131203049));
#25329=CARTESIAN_POINT('Ctrl Pts',(-4.312545272057,5.2176881731829,65.4168384008471));
#25330=CARTESIAN_POINT('Ctrl Pts',(-4.44473070729526,5.10554835726461,65.4249636813893));
#25331=CARTESIAN_POINT('Ctrl Pts',(-4.5723440382569,4.98858286448332,65.4330889619315));
#25332=CARTESIAN_POINT('Ctrl Pts',(-4.70134768998026,4.87034305692792,65.4413027657193));
#25333=CARTESIAN_POINT('Ctrl Pts',(-4.8256787463408,4.74717206650763,65.4495165695071));
#25334=CARTESIAN_POINT('Ctrl Pts',(-4.94495508350294,4.61949220392658,65.4577303732949));
#25335=CARTESIAN_POINT('Ctrl Pts',(-5.06315011094663,4.49296983393413,65.46586971415));
#25336=CARTESIAN_POINT('Ctrl Pts',(-5.17638150033589,4.36202032483429,65.4740090550052));
#25337=CARTESIAN_POINT('Ctrl Pts',(-5.28431928187561,4.22708631650664,65.4821483958603));
#25338=CARTESIAN_POINT('Ctrl Pts',(-5.39373827004506,4.09030063821819,65.4903994311144));
#25339=CARTESIAN_POINT('Ctrl Pts',(-5.49771707765679,3.94942062669911,65.4986504663685));
#25340=CARTESIAN_POINT('Ctrl Pts',(-5.59595874013158,3.80493558141856,65.5069015016226));
#25341=CARTESIAN_POINT('Ctrl Pts',(-5.69420040260637,3.66045053613801,65.5151525368767));
#25342=CARTESIAN_POINT('Ctrl Pts',(-5.78670477345048,3.51236081820523,65.5234035721308));
#25343=CARTESIAN_POINT('Ctrl Pts',(-5.87322448394943,3.3611788350424,65.531654607385));
#25344=CARTESIAN_POINT('Ctrl Pts',(-5.96439181895416,3.20187573027931,65.540348867812));
#25345=CARTESIAN_POINT('Ctrl Pts',(-6.0491723615721,3.03868961436006,65.549043128239));
#25346=CARTESIAN_POINT('Ctrl Pts',(-6.12724033271902,2.87214465253778,65.557737388666));
#25347=CARTESIAN_POINT('Ctrl Pts',(-6.20517873351879,2.70587610738423,65.5664172191248));
#25348=CARTESIAN_POINT('Ctrl Pts',(-6.27642665120116,2.53626009983261,65.5750970495836));
#25349=CARTESIAN_POINT('Ctrl Pts',(-6.34070319849406,2.36384685388186,65.5837768800424));
#25350=CARTESIAN_POINT('Ctrl Pts',(-6.40487649698476,2.19171055904124,65.5924427679026));
#25351=CARTESIAN_POINT('Ctrl Pts',(-6.46210065051034,2.01678626298182,65.6011086557628));
#25352=CARTESIAN_POINT('Ctrl Pts',(-6.51214175033427,1.83964638546469,65.609774543623));
#25353=CARTESIAN_POINT('Ctrl Pts',(-6.56207425720522,1.66289091481427,65.6184216258543));
#25354=CARTESIAN_POINT('Ctrl Pts',(-6.60485472726086,1.48392974022276,65.6270687080857));
#25355=CARTESIAN_POINT('Ctrl Pts',(-6.64029831080929,1.3033523481635,65.635715790317));
#25356=CARTESIAN_POINT('Ctrl Pts',(-6.67569497199666,1.12301401538497,65.6443514250175));
#25357=CARTESIAN_POINT('Ctrl Pts',(-6.70377405277301,0.941064021336169,
65.652987059718));
#25358=CARTESIAN_POINT('Ctrl Pts',(-6.72440064845059,0.758106139743788,
65.6616226944185));
#25359=CARTESIAN_POINT('Ctrl Pts',(-6.74499123012988,0.57546770227781,65.6702432513166));
#25360=CARTESIAN_POINT('Ctrl Pts',(-6.75815524987472,0.391825182658888,
65.6788638082147));
#25361=CARTESIAN_POINT('Ctrl Pts',(-6.76380896286626,0.207791515346705,
65.6874843651129));
#25362=CARTESIAN_POINT('Ctrl Pts',(-6.76592851327327,0.138798159115133,
65.6907161713452));
#25363=CARTESIAN_POINT('Ctrl Pts',(-6.76699303084327,0.0697499303004344,
65.6939479775776));
#25364=CARTESIAN_POINT('Ctrl Pts',(-6.76699996589014,0.000679443041806397,
65.69717978381));
#25365=CARTESIAN_POINT('',(-6.767,2.89194517400122E-12,65.3028202161898));
#25366=CARTESIAN_POINT('Ctrl Pts',(3.09917575053261,6.01559628526638,64.6514343427993));
#25367=CARTESIAN_POINT('Ctrl Pts',(2.94375971393036,6.09566509125678,64.6596348930289));
#25368=CARTESIAN_POINT('Ctrl Pts',(2.78522125750516,6.16971616999855,64.6678354432586));
#25369=CARTESIAN_POINT('Ctrl Pts',(2.62406952193042,6.23751137426425,64.6760359934882));
#25370=CARTESIAN_POINT('Ctrl Pts',(2.46290172942686,6.30531333354729,64.684237360809));
#25371=CARTESIAN_POINT('Ctrl Pts',(2.29912046921022,6.36685803712996,64.6924387281298));
#25372=CARTESIAN_POINT('Ctrl Pts',(2.13325468635921,6.42195557779143,64.7006400954506));
#25373=CARTESIAN_POINT('Ctrl Pts',(1.96734231772071,6.47706859338858,64.7088437662431));
#25374=CARTESIAN_POINT('Ctrl Pts',(1.79934460013952,6.52573072586477,64.7170474370357));
#25375=CARTESIAN_POINT('Ctrl Pts',(1.62980550425163,6.56780199292816,64.7252511078283));
#25376=CARTESIAN_POINT('Ctrl Pts',(1.46018806547383,6.60989270084456,64.7334585694827));
#25377=CARTESIAN_POINT('Ctrl Pts',(1.28902817689152,6.64538639014321,64.741666031137));
#25378=CARTESIAN_POINT('Ctrl Pts',(1.11687991222064,6.67419420317375,64.7498734927914));
#25379=CARTESIAN_POINT('Ctrl Pts',(0.944529275986097,6.70303588167589,64.7580906028546));
#25380=CARTESIAN_POINT('Ctrl Pts',(0.771188296612574,6.72517592828298,64.7663077129179));
#25381=CARTESIAN_POINT('Ctrl Pts',(0.597417027559221,6.74057726720659,64.7745248229812));
#25382=CARTESIAN_POINT('Ctrl Pts',(0.423526475807104,6.75598917814986,64.7827475735572));
#25383=CARTESIAN_POINT('Ctrl Pts',(0.249205402286185,6.76465314425268,64.7909703241333));
#25384=CARTESIAN_POINT('Ctrl Pts',(0.075013652945595,6.76658421597424,64.7991930747093));
#25385=CARTESIAN_POINT('Ctrl Pts',(-0.0994197767091728,6.76851796693878,
64.8074272338449));
#25386=CARTESIAN_POINT('Ctrl Pts',(-0.273723167262516,6.76370017898385,
64.8156613929804));
#25387=CARTESIAN_POINT('Ctrl Pts',(-0.447341076683874,6.75219778746975,
64.823895552116));
#25388=CARTESIAN_POINT('Ctrl Pts',(-0.503180604735224,6.74849835279881,
64.8265438477991));
#25389=CARTESIAN_POINT('Ctrl Pts',(-0.558949299836695,6.74410784974981,
64.8291921434822));
#25390=CARTESIAN_POINT('Ctrl Pts',(-0.614628923382891,6.73902962499359,
64.8318404391653));
#25391=CARTESIAN_POINT('Ctrl Pts',(-0.786094993744047,6.72339117078174,
64.8399958975721));
#25392=CARTESIAN_POINT('Ctrl Pts',(-0.957243499080527,6.70117883226029,
64.8481513559789));
#25393=CARTESIAN_POINT('Ctrl Pts',(-1.12752523770424,6.67240405238921,64.8563068143857));
#25394=CARTESIAN_POINT('Ctrl Pts',(-1.297599721069,6.6436642952076,64.8644523465276));
#25395=CARTESIAN_POINT('Ctrl Pts',(-1.46680918125153,6.60837805610042,64.8725978786695));
#25396=CARTESIAN_POINT('Ctrl Pts',(-1.63460675862359,6.56660869434612,64.8807434108113));
#25397=CARTESIAN_POINT('Ctrl Pts',(-1.80223538875119,6.52488138813686,64.8888807416119));
#25398=CARTESIAN_POINT('Ctrl Pts',(-1.96845461410872,6.4766840420883,64.8970180724124));
#25399=CARTESIAN_POINT('Ctrl Pts',(-2.13272502719967,6.42213149650147,64.905155403213));
#25400=CARTESIAN_POINT('Ctrl Pts',(-2.29686456631296,6.36762241284122,64.913286251015));
#25401=CARTESIAN_POINT('Ctrl Pts',(-2.45905803934959,6.30676832571617,64.9214170988169));
#25402=CARTESIAN_POINT('Ctrl Pts',(-2.61877853279932,6.23973460943248,64.9295479466189));
#25403=CARTESIAN_POINT('Ctrl Pts',(-2.77840532923954,6.17274021721181,64.9376740246127));
#25404=CARTESIAN_POINT('Ctrl Pts',(-2.93556169900813,6.0995735563644,64.9458001026065));
#25405=CARTESIAN_POINT('Ctrl Pts',(-3.08973814461677,6.02044908604833,64.9539261806002));
#25406=CARTESIAN_POINT('Ctrl Pts',(-3.24446127174295,5.94104405481171,64.9620810721824));
#25407=CARTESIAN_POINT('Ctrl Pts',(-3.39618295244663,5.85563900897581,64.9702359637646));
#25408=CARTESIAN_POINT('Ctrl Pts',(-3.54441014670346,5.76449873900112,64.9783908553468));
#25409=CARTESIAN_POINT('Ctrl Pts',(-3.69205930672856,5.67371388421324,64.9865139457031));
#25410=CARTESIAN_POINT('Ctrl Pts',(-3.83624088114111,5.57723866324328,64.9946370360593));
#25411=CARTESIAN_POINT('Ctrl Pts',(-3.97649411459707,5.47537976368533,65.0027601264156));
#25412=CARTESIAN_POINT('Ctrl Pts',(-4.11675836137747,5.3735128657014,65.0108838546341));
#25413=CARTESIAN_POINT('Ctrl Pts',(-4.25309335673059,5.26626166199667,65.0190075828525));
#25414=CARTESIAN_POINT('Ctrl Pts',(-4.38506931010397,5.15397479093411,65.0271313110709));
#25415=CARTESIAN_POINT('Ctrl Pts',(-4.51708073509931,5.04165774015062,65.0352572227312));
#25416=CARTESIAN_POINT('Ctrl Pts',(-4.64473050674262,4.92430256398938,65.0433831343915));
#25417=CARTESIAN_POINT('Ctrl Pts',(-4.76762379333834,4.8022965719741,65.0515090460517));
#25418=CARTESIAN_POINT('Ctrl Pts',(-4.89130299527776,4.67951033895619,65.0596869237618));
#25419=CARTESIAN_POINT('Ctrl Pts',(-5.01016439802514,4.55201386333625,65.0678648014719));
#25420=CARTESIAN_POINT('Ctrl Pts',(-5.12384551322782,4.42023711542436,65.076042679182));
#25421=CARTESIAN_POINT('Ctrl Pts',(-5.23698405312371,4.28908930934948,65.0841815256555));
#25422=CARTESIAN_POINT('Ctrl Pts',(-5.34499146583222,4.15370232343359,65.0923203721289));
#25423=CARTESIAN_POINT('Ctrl Pts',(-5.44755317658133,4.0145302824015,65.1004592186024));
#25424=CARTESIAN_POINT('Ctrl Pts',(-5.55085266578855,3.87435710621776,65.1086566119308));
#25425=CARTESIAN_POINT('Ctrl Pts',(-5.64862759806098,3.73034452649665,65.1168540052592));
#25426=CARTESIAN_POINT('Ctrl Pts',(-5.74060314250142,3.58298263466387,65.1250513985876));
#25427=CARTESIAN_POINT('Ctrl Pts',(-5.83257868694183,3.43562074283113,65.133248791916));
#25428=CARTESIAN_POINT('Ctrl Pts',(-5.91875471183224,3.2849098923583,65.1414461852444));
#25429=CARTESIAN_POINT('Ctrl Pts',(-5.99890541045201,3.13136118588221,65.1496435785728));
#25430=CARTESIAN_POINT('Ctrl Pts',(-6.08459861006928,2.96719443273324,65.1584078298511));
#25431=CARTESIAN_POINT('Ctrl Pts',(-6.16363353114575,2.79934626405396,65.1671720811293));
#25432=CARTESIAN_POINT('Ctrl Pts',(-6.23570284825551,2.6283643180233,65.1759363324076));
#25433=CARTESIAN_POINT('Ctrl Pts',(-6.30764909610388,2.45767434953112,65.184685617401));
#25434=CARTESIAN_POINT('Ctrl Pts',(-6.37265335096421,2.28386153835232,65.1934349023943));
#25435=CARTESIAN_POINT('Ctrl Pts',(-6.4304543836683,2.10749743049929,65.2021841873877));
#25436=CARTESIAN_POINT('Ctrl Pts',(-6.48811187486979,1.93157130044463,65.2109117446462));
#25437=CARTESIAN_POINT('Ctrl Pts',(-6.53860174470766,1.75310678554235,65.2196393019047));
#25438=CARTESIAN_POINT('Ctrl Pts',(-6.58171120573811,1.57269405933302,65.2283668591632));
#25439=CARTESIAN_POINT('Ctrl Pts',(-6.62475642100836,1.39255020108145,65.2370814097977));
#25440=CARTESIAN_POINT('Ctrl Pts',(-6.66044309148477,1.21046419699874,65.2457959604321));
#25441=CARTESIAN_POINT('Ctrl Pts',(-6.68860767397279,1.02704254228941,65.2545105110666));
#25442=CARTESIAN_POINT('Ctrl Pts',(-6.71670982045616,0.844027501641936,
65.2632057430507));
#25443=CARTESIAN_POINT('Ctrl Pts',(-6.73732310326782,0.659682999136313,
65.2719009750348));
#25444=CARTESIAN_POINT('Ctrl Pts',(-6.75033471810914,0.4746263725189,65.2805962070188));
#25445=CARTESIAN_POINT('Ctrl Pts',(-6.76142011326569,0.316965247638418,
65.2880042100758));
#25446=CARTESIAN_POINT('Ctrl Pts',(-6.76698872150269,0.158787577000224,
65.2954122131328));
#25447=CARTESIAN_POINT('Ctrl Pts',(-6.76699998287805,0.00048138183613871,
65.3028202161898));
#25448=CARTESIAN_POINT('Ctrl Pts',(-6.767,2.89194522689237E-12,65.3028202161898));
#25449=CARTESIAN_POINT('Ctrl Pts',(-6.76700000000008,-0.186007249412905,
65.3115697279958));
#25450=CARTESIAN_POINT('Ctrl Pts',(-6.75932637295453,-0.372014355524879,
65.3203192398017));
#25451=CARTESIAN_POINT('Ctrl Pts',(-6.74400518266949,-0.557389537152518,
65.3290687516077));
#25452=CARTESIAN_POINT('Ctrl Pts',(-6.72868405709673,-0.742763935808937,
65.3378182264582));
#25453=CARTESIAN_POINT('Ctrl Pts',(-6.70571545653024,-0.92750612969265,
65.3465677013087));
#25454=CARTESIAN_POINT('Ctrl Pts',(-6.67517739415689,-1.11098863924745,
65.3553171761593));
#25455=CARTESIAN_POINT('Ctrl Pts',(-6.6446394582311,-1.29447038906452,65.3640666147813));
#25456=CARTESIAN_POINT('Ctrl Pts',(-6.60653217027165,-1.47669218228184,
65.3728160534033));
#25457=CARTESIAN_POINT('Ctrl Pts',(-6.56098496116716,-1.65703510504105,
65.3815654920253));
#25458=CARTESIAN_POINT('Ctrl Pts',(-6.51543793687516,-1.83737729604025,
65.3903148951455));
#25459=CARTESIAN_POINT('Ctrl Pts',(-6.46245112202632,-2.01584035397077,
65.3990642982658));
#25460=CARTESIAN_POINT('Ctrl Pts',(-6.40220448416228,-2.19181813638186,
65.407813701386));
#25461=CARTESIAN_POINT('Ctrl Pts',(-6.34195808575169,-2.36779521935993,
65.4165630697313));
#25462=CARTESIAN_POINT('Ctrl Pts',(-6.27445201489212,-2.54128677544883,
65.4253124380765));
#25463=CARTESIAN_POINT('Ctrl Pts',(-6.19991555136157,-2.71170355237903,
65.4340618064218));
#25464=CARTESIAN_POINT('Ctrl Pts',(-6.1253793778901,-2.88211966613133,65.4428111407189));
#25465=CARTESIAN_POINT('Ctrl Pts',(-6.04381298133587,-3.04946076210504,
65.4515604750159));
#25466=CARTESIAN_POINT('Ctrl Pts',(-5.95549339426275,-3.21315848206912,
65.460309809313));
#25467=CARTESIAN_POINT('Ctrl Pts',(-5.86717414355121,-3.37685557859705,
65.4690591102886));
#25468=CARTESIAN_POINT('Ctrl Pts',(-5.7721018898619,-3.53690907467391,65.4778084112641));
#25469=CARTESIAN_POINT('Ctrl Pts',(-5.6705995346701,-3.69277536784994,65.4865577122397));
#25470=CARTESIAN_POINT('Ctrl Pts',(-5.56909755761702,-3.84864108035885,
65.4953069806205));
#25471=CARTESIAN_POINT('Ctrl Pts',(-5.46116568338001,-4.00031938104373,
65.5040562490012));
#25472=CARTESIAN_POINT('Ctrl Pts',(-5.3471704868604,-4.14729511663314,65.512805517382));
#25473=CARTESIAN_POINT('Ctrl Pts',(-5.23317570555443,-4.29427031688131,
65.5215547538946));
#25474=CARTESIAN_POINT('Ctrl Pts',(-5.1131178217873,-4.43654275987216,65.5303039904072));
#25475=CARTESIAN_POINT('Ctrl Pts',(-4.98740459171939,-4.57362924147732,
65.5390532269198));
#25476=CARTESIAN_POINT('Ctrl Pts',(-4.86169180910754,-4.71071523514514,
65.547802432291));
#25477=CARTESIAN_POINT('Ctrl Pts',(-4.73032391415356,-4.84261509316597,
65.5565516376621));
#25478=CARTESIAN_POINT('Ctrl Pts',(-4.59374707237218,-4.96888084331593,
65.5653008430332));
#25479=CARTESIAN_POINT('Ctrl Pts',(-4.45717070537329,-5.09514615452788,
65.5740500179894));
#25480=CARTESIAN_POINT('Ctrl Pts',(-4.31538563819439,-5.21577720253691,
65.5827991929457));
#25481=CARTESIAN_POINT('Ctrl Pts',(-4.1688734129058,-5.33036429028703,65.5915483679019));
#25482=CARTESIAN_POINT('Ctrl Pts',(-4.02236168477266,-5.4449509892123,65.6002975131698));
#25483=CARTESIAN_POINT('Ctrl Pts',(-3.87112305634363,-5.55349359238812,
65.6090466584377));
#25484=CARTESIAN_POINT('Ctrl Pts',(-3.71567117316652,-5.65562346102526,
65.6177958037056));
#25485=CARTESIAN_POINT('Ctrl Pts',(-3.56021980457219,-5.7577529915882,65.6265449200118));
#25486=CARTESIAN_POINT('Ctrl Pts',(-3.40055544862305,-5.85346967275401,
65.635294036318));
#25487=CARTESIAN_POINT('Ctrl Pts',(-3.23722036323319,-5.94244842803607,
65.6440431526241));
#25488=CARTESIAN_POINT('Ctrl Pts',(-3.07388580495966,-6.03142689616516,
65.6527922406951));
#25489=CARTESIAN_POINT('Ctrl Pts',(-2.90688079257629,-6.11366734484859,
65.661541328766));
#25490=CARTESIAN_POINT('Ctrl Pts',(-2.7367725109454,-6.18889046787335,65.670290416837));
#25491=CARTESIAN_POINT('Ctrl Pts',(-2.5666647641658,-6.26411335438297,65.6790394773992));
#25492=CARTESIAN_POINT('Ctrl Pts',(-2.39345402972038,-6.33231884350311,
65.6877885379614));
#25493=CARTESIAN_POINT('Ctrl Pts',(-2.21772856473993,-6.39327529621059,
65.6965375985236));
#25494=CARTESIAN_POINT('Ctrl Pts',(-2.04200363768215,-6.45423156232099,
65.7052866323036));
#25495=CARTESIAN_POINT('Ctrl Pts',(-1.86376426620028,-6.50793874252075,
65.7140356660836));
#25496=CARTESIAN_POINT('Ctrl Pts',(-1.68361578194613,-6.55421443796142,
65.7227846998636));
#25497=CARTESIAN_POINT('Ctrl Pts',(-1.50346783419786,-6.60048999558698,
65.7315337075879));
#25498=CARTESIAN_POINT('Ctrl Pts',(-1.32141106257158,-6.63933404145513,
65.7402827153121));
#25499=CARTESIAN_POINT('Ctrl Pts',(-1.13806375958949,-6.67061465527046,
65.7490317230363));
#25500=CARTESIAN_POINT('Ctrl Pts',(-0.954716987417697,-6.70189517852503,
65.7577807054312));
#25501=CARTESIAN_POINT('Ctrl Pts',(-0.770079973807906,-6.72561226535852,
65.7665296878262));
#25502=CARTESIAN_POINT('Ctrl Pts',(-0.584779770549973,-6.74168536939804,
65.7752786702211));
#25503=CARTESIAN_POINT('Ctrl Pts',(-0.391490647551475,-6.75845143942408,
65.7844048508971));
#25504=CARTESIAN_POINT('Ctrl Pts',(-0.197480213101951,-6.76689975924033,
65.7935310315732));
#25505=CARTESIAN_POINT('Ctrl Pts',(-0.00346532629546626,-6.76699911271708,
65.8026572122492));
#25506=CARTESIAN_POINT('Ctrl Pts',(0.184486595298346,-6.76709536139767,
65.8114981997791));
#25507=CARTESIAN_POINT('Ctrl Pts',(0.37244237818748,-6.75935659726758,65.8203391873091));
#25508=CARTESIAN_POINT('Ctrl Pts',(0.559750217724292,-6.74380965728998,
65.829180174839));
#25509=CARTESIAN_POINT('Ctrl Pts',(0.745129914459954,-6.72842275717229,
65.8379301534367));
#25510=CARTESIAN_POINT('Ctrl Pts',(0.929874656316376,-6.70538772273442,
65.8466801320345));
#25511=CARTESIAN_POINT('Ctrl Pts',(1.11335688289995,-6.67478280180706,65.8554301106323));
#25512=CARTESIAN_POINT('Ctrl Pts',(1.29683723119073,-6.64417819417981,65.8641799996572));
#25513=CARTESIAN_POINT('Ctrl Pts',(1.4790548073045,-6.60600390230027,65.8729298886822));
#25514=CARTESIAN_POINT('Ctrl Pts',(1.6593906480502,-6.56038959797081,65.8816797777071));
#25515=CARTESIAN_POINT('Ctrl Pts',(1.83972470264481,-6.51477574543195,65.8904295800681));
#25516=CARTESIAN_POINT('Ctrl Pts',(2.01817678126068,-6.46172209820031,65.899179382429));
#25517=CARTESIAN_POINT('Ctrl Pts',(2.19414072347902,-6.40140886723938,65.90792918479));
#25518=CARTESIAN_POINT('Ctrl Pts',(2.37010298132325,-6.34109621361289,65.9166789033955));
#25519=CARTESIAN_POINT('Ctrl Pts',(2.54357687927145,-6.27352420825877,65.925428622001));
#25520=CARTESIAN_POINT('Ctrl Pts',(2.71397317790207,-6.19892237325393,65.9341783406065));
#25521=CARTESIAN_POINT('Ctrl Pts',(2.88436790207433,-6.12432122756854,65.9429279783647));
#25522=CARTESIAN_POINT('Ctrl Pts',(3.05168482126484,-6.04269049717302,65.951677616123));
#25523=CARTESIAN_POINT('Ctrl Pts',(3.21535561997612,-5.95430745234809,65.9604272538812));
#25524=CARTESIAN_POINT('Ctrl Pts',(3.37902496075494,-5.86592519481394,65.9691768137002));
#25525=CARTESIAN_POINT('Ctrl Pts',(3.53904799385078,-5.77079087940107,65.9779263735193));
#25526=CARTESIAN_POINT('Ctrl Pts',(3.69488118815177,-5.66922763746898,65.9866759333383));
#25527=CARTESIAN_POINT('Ctrl Pts',(3.85071304611019,-5.56766526648923,65.9954254181257));
#25528=CARTESIAN_POINT('Ctrl Pts',(4.00235489706147,-5.45967423580582,66.0041749029131));
#25529=CARTESIAN_POINT('Ctrl Pts',(4.14929168607827,-5.34562133936195,66.0129243877006));
#25530=CARTESIAN_POINT('Ctrl Pts',(4.29622726385921,-5.23156938308396,66.0216738003639));
#25531=CARTESIAN_POINT('Ctrl Pts',(4.43845763092223,-5.11145583677067,66.0304232130272));
#25532=CARTESIAN_POINT('Ctrl Pts',(4.5754997066111,-4.98568866204076,66.0391726256905));
#25533=CARTESIAN_POINT('Ctrl Pts',(4.71254069815441,-4.85992248226019,66.0479219691368));
#25534=CARTESIAN_POINT('Ctrl Pts',(4.84439326931459,-4.72850295733854,66.0566713125831));
#25535=CARTESIAN_POINT('Ctrl Pts',(4.97060959434841,-4.59187644221527,66.0654206560294));
#25536=CARTESIAN_POINT('Ctrl Pts',(5.0968249628065,-4.45525096256509,66.0741699331657));
#25537=CARTESIAN_POINT('Ctrl Pts',(5.21740397615966,-4.31341878218172,66.082919210302));
#25538=CARTESIAN_POINT('Ctrl Pts',(5.33193710452053,-4.16686161438525,66.0916684874383));
#25539=CARTESIAN_POINT('Ctrl Pts',(5.44646940289506,-4.02030550864347,66.1004177011713));
#25540=CARTESIAN_POINT('Ctrl Pts',(5.55495572749791,-3.86902470979953,66.1091669149043));
#25541=CARTESIAN_POINT('Ctrl Pts',(5.65702762491584,-3.71353301465586,66.1179161286372));
#25542=CARTESIAN_POINT('Ctrl Pts',(5.75909881655278,-3.55804239466692,66.1266652818733));
#25543=CARTESIAN_POINT('Ctrl Pts',(5.85475551250903,-3.39834117619345,66.1354144351095));
#25544=CARTESIAN_POINT('Ctrl Pts',(5.94367283728211,-3.23497174691756,66.1441635883456));
#25545=CARTESIAN_POINT('Ctrl Pts',(6.0325895767643,-3.07160339300735,66.1529126839911));
#25546=CARTESIAN_POINT('Ctrl Pts',(6.11476689685403,-2.90456712829255,66.1616617796367));
#25547=CARTESIAN_POINT('Ctrl Pts',(6.18992570525379,-2.73443024475636,66.1704108752822));
#25548=CARTESIAN_POINT('Ctrl Pts',(6.26508404388814,-2.56429442462746,66.1791599162432));
#25549=CARTESIAN_POINT('Ctrl Pts',(6.33322384283428,-2.39105828655694,66.1879089572043));
#25550=CARTESIAN_POINT('Ctrl Pts',(6.39411368720141,-2.21531017131767,66.1966579981653));
#25551=CARTESIAN_POINT('Ctrl Pts',(6.45500317120987,-2.03956309619208,66.2054069873477));
#25552=CARTESIAN_POINT('Ctrl Pts',(6.50864269270159,-1.86130434438333,66.2141559765301));
#25553=CARTESIAN_POINT('Ctrl Pts',(6.55485008446409,-1.68113930719652,66.2229049657125));
#25554=CARTESIAN_POINT('Ctrl Pts',(6.60199664749469,-1.49731239211552,66.2318317792419));
#25555=CARTESIAN_POINT('Ctrl Pts',(6.64140563640962,-1.31150116499389,66.2407585927712));
#25556=CARTESIAN_POINT('Ctrl Pts',(6.67293772282219,-1.12436255155384,66.2496854063006));
#25557=CARTESIAN_POINT('Ctrl Pts',(6.7038449494991,-0.940932395048565,66.2584353204561));
#25558=CARTESIAN_POINT('Ctrl Pts',(6.72718449348962,-0.756227260503922,
66.2671852346117));
#25559=CARTESIAN_POINT('Ctrl Pts',(6.74287707373956,-0.570874564538889,
66.2759351487672));
#25560=CARTESIAN_POINT('Ctrl Pts',(6.75856934538687,-0.385525513629619,
66.2846848908512));
#25561=CARTESIAN_POINT('Ctrl Pts',(6.76661493004112,-0.199529212415323,
66.2934346329351));
#25562=CARTESIAN_POINT('Ctrl Pts',(6.76698649908907,-0.0135174385974741,
66.3021843750191));
#25563=CARTESIAN_POINT('Ctrl Pts',(6.76735806132382,0.172490924448746,66.310933956665));
#25564=CARTESIAN_POINT('Ctrl Pts',(6.76005588896273,0.358514472904385,66.3196835383109));
#25565=CARTESIAN_POINT('Ctrl Pts',(6.7451047845456,0.543921359665198,66.3284331199568));
#25566=CARTESIAN_POINT('Ctrl Pts',(6.73015393440655,0.72932509315348,66.3371825527959));
#25567=CARTESIAN_POINT('Ctrl Pts',(6.70755443556855,0.914111900259432,66.3459319856349));
#25568=CARTESIAN_POINT('Ctrl Pts',(6.67738304682267,1.0976541559185,66.3546814184739));
#25569=CARTESIAN_POINT('Ctrl Pts',(6.647212131118,1.28119353391585,66.3634307141353));
#25570=CARTESIAN_POINT('Ctrl Pts',(6.60946960955425,1.46348811672965,66.3721800097966));
#25571=CARTESIAN_POINT('Ctrl Pts',(6.56428366991105,1.64391876348533,66.3809293054579));
#25572=CARTESIAN_POINT('Ctrl Pts',(6.51909837867631,1.82434682110023,66.3896784755687));
#25573=CARTESIAN_POINT('Ctrl Pts',(6.46646995271828,2.00291071820747,66.3984276456796));
#25574=CARTESIAN_POINT('Ctrl Pts',(6.40657713281448,2.17900400213,66.4071768157904));
#25575=CARTESIAN_POINT('Ctrl Pts',(6.34668509278951,2.35509499309951,66.4159258719762));
#25576=CARTESIAN_POINT('Ctrl Pts',(6.27952894037409,2.52871516398412,66.424674928162));
#25577=CARTESIAN_POINT('Ctrl Pts',(6.20533675061323,2.69927486771705,66.4334239843477));
#25578=CARTESIAN_POINT('Ctrl Pts',(6.12832117907792,2.87632521636188,66.44250598563));
#25579=CARTESIAN_POINT('Ctrl Pts',(6.04372366625955,3.05007728920243,66.4515879869122));
#25580=CARTESIAN_POINT('Ctrl Pts',(5.95185378007745,3.21989527478422,66.4606699881945));
#25581=CARTESIAN_POINT('Ctrl Pts',(5.86334450817242,3.38350129286976,66.4694197685016));
#25582=CARTESIAN_POINT('Ctrl Pts',(5.76808562057119,3.54345567125184,66.4781695488088));
#25583=CARTESIAN_POINT('Ctrl Pts',(5.6664006880434,3.69921508465529,66.4869193291159));
#25584=CARTESIAN_POINT('Ctrl Pts',(5.56471941107771,3.85496889852504,66.4956687948694));
#25585=CARTESIAN_POINT('Ctrl Pts',(5.45661270814951,4.00652780919858,66.5044182606229));
#25586=CARTESIAN_POINT('Ctrl Pts',(5.34244776448942,4.15337704569451,66.5131677263764));
#25587=CARTESIAN_POINT('Ctrl Pts',(5.22828631819414,4.3002217835647,66.5219169240959));
#25588=CARTESIAN_POINT('Ctrl Pts',(5.10806717843878,4.44235690972898,66.5306661218155));
#25589=CARTESIAN_POINT('Ctrl Pts',(4.98219864544519,4.57929969070863,66.5394153195351));
#25590=CARTESIAN_POINT('Ctrl Pts',(4.85633329943824,4.71623900430207,66.5481642957254));
#25591=CARTESIAN_POINT('Ctrl Pts',(4.72481904033448,4.84798602483812,66.5569132719156));
#25592=CARTESIAN_POINT('Ctrl Pts',(4.58810250736999,4.97409332259309,66.5656622481058));
#25593=CARTESIAN_POINT('Ctrl Pts',(4.45137708685437,5.10020881822314,66.574411793042));
#25594=CARTESIAN_POINT('Ctrl Pts',(4.30944892635841,5.22068366308107,66.5831613379782));
#25595=CARTESIAN_POINT('Ctrl Pts',(4.16280009466445,5.33510865605019,66.5919108829144));
#25596=CARTESIAN_POINT('Ctrl Pts',(4.0161598834857,5.44952692273053,66.6006599135227));
#25597=CARTESIAN_POINT('Ctrl Pts',(3.86479978232009,5.5578958728878,66.6094089441309));
#25598=CARTESIAN_POINT('Ctrl Pts',(3.70923383580844,5.65984746714024,66.6181579747392));
#25599=CARTESIAN_POINT('Ctrl Pts',(3.55366577799305,5.76180044505528,66.6269071240872));
#25600=CARTESIAN_POINT('Ctrl Pts',(3.39389200026593,5.85733573571203,66.6356562734353));
#25601=CARTESIAN_POINT('Ctrl Pts',(3.23045513625782,5.94612887622069,66.6444054227833));
#25602=CARTESIAN_POINT('Ctrl Pts',(3.18695122151402,5.96976399206781,66.6467342868962));
#25603=CARTESIAN_POINT('Ctrl Pts',(3.14318791262572,5.9929216543538,66.6490631510091));
#25604=CARTESIAN_POINT('Ctrl Pts',(3.09917575053252,6.01559628526643,66.6513920151221));
#25605=CARTESIAN_POINT('Origin',(0.,0.,-3.69717978381041));
#25606=CARTESIAN_POINT('',(3.09917575053257,6.0155962852664,69.0457515827422));
#25607=CARTESIAN_POINT('',(3.09917575053259,6.01559628526639,68.6513920151221));
#25608=CARTESIAN_POINT('',(3.09917575053259,6.01559628526639,-3.69717978381041));
#25609=CARTESIAN_POINT('',(-6.767,3.21349643130162E-12,67.6971797838099));
#25610=CARTESIAN_POINT('Ctrl Pts',(-6.767,3.2134964569793E-12,67.6971797838099));
#25611=CARTESIAN_POINT('Ctrl Pts',(-6.76700000000009,-0.186007249412519,
67.7059292956159));
#25612=CARTESIAN_POINT('Ctrl Pts',(-6.75932637295455,-0.37201435552443,
67.7146788074218));
#25613=CARTESIAN_POINT('Ctrl Pts',(-6.74400518266953,-0.557389537152005,
67.7234283192278));
#25614=CARTESIAN_POINT('Ctrl Pts',(-6.72868405709677,-0.742763935808616,
67.7321777940783));
#25615=CARTESIAN_POINT('Ctrl Pts',(-6.70571545653027,-0.927506129692518,
67.7409272689289));
#25616=CARTESIAN_POINT('Ctrl Pts',(-6.67517739415688,-1.1109886392475,67.7496767437794));
#25617=CARTESIAN_POINT('Ctrl Pts',(-6.64463945823111,-1.29447038906445,
67.7584261824014));
#25618=CARTESIAN_POINT('Ctrl Pts',(-6.60653217027169,-1.47669218228164,
67.7671756210234));
#25619=CARTESIAN_POINT('Ctrl Pts',(-6.56098496116724,-1.65703510504073,
67.7759250596454));
#25620=CARTESIAN_POINT('Ctrl Pts',(-6.51543793687527,-1.83737729603987,
67.7846744627656));
#25621=CARTESIAN_POINT('Ctrl Pts',(-6.46245112202646,-2.01584035397033,
67.7934238658859));
#25622=CARTESIAN_POINT('Ctrl Pts',(-6.40220448416245,-2.19181813638136,
67.8021732690061));
#25623=CARTESIAN_POINT('Ctrl Pts',(-6.34195808575187,-2.36779521935944,
67.8109226373514));
#25624=CARTESIAN_POINT('Ctrl Pts',(-6.27445201489232,-2.54128677544834,
67.8196720056966));
#25625=CARTESIAN_POINT('Ctrl Pts',(-6.19991555136178,-2.71170355237854,
67.8284213740419));
#25626=CARTESIAN_POINT('Ctrl Pts',(-6.12537937789035,-2.88211966613079,
67.837170708339));
#25627=CARTESIAN_POINT('Ctrl Pts',(-6.04381298133617,-3.04946076210445,
67.845920042636));
#25628=CARTESIAN_POINT('Ctrl Pts',(-5.9554933942631,-3.21315848206848,67.8546693769331));
#25629=CARTESIAN_POINT('Ctrl Pts',(-5.86717414355173,-3.37685557859614,
67.8634186779086));
#25630=CARTESIAN_POINT('Ctrl Pts',(-5.77210188986261,-3.53690907467274,
67.8721679788842));
#25631=CARTESIAN_POINT('Ctrl Pts',(-5.67059953467102,-3.69277536784853,
67.8809172798597));
#25632=CARTESIAN_POINT('Ctrl Pts',(-5.56909755761809,-3.84864108035729,
67.8896665482405));
#25633=CARTESIAN_POINT('Ctrl Pts',(-5.46116568338124,-4.00031938104206,
67.8984158166213));
#25634=CARTESIAN_POINT('Ctrl Pts',(-5.34717048686179,-4.14729511663135,
67.907165085002));
#25635=CARTESIAN_POINT('Ctrl Pts',(-5.23317570555586,-4.29427031687956,
67.9159143215146));
#25636=CARTESIAN_POINT('Ctrl Pts',(-5.11311782178878,-4.43654275987045,
67.9246635580272));
#25637=CARTESIAN_POINT('Ctrl Pts',(-4.98740459172092,-4.57362924147565,
67.9334127945399));
#25638=CARTESIAN_POINT('Ctrl Pts',(-4.86169180910908,-4.71071523514356,
67.942161999911));
#25639=CARTESIAN_POINT('Ctrl Pts',(-4.73032391415509,-4.84261509316448,
67.9509112052821));
#25640=CARTESIAN_POINT('Ctrl Pts',(-4.59374707237371,-4.96888084331452,
67.9596604106532));
#25641=CARTESIAN_POINT('Ctrl Pts',(-4.457170705375,-5.09514615452638,67.9684095856094));
#25642=CARTESIAN_POINT('Ctrl Pts',(-4.31538563819628,-5.21577720253533,
67.9771587605656));
#25643=CARTESIAN_POINT('Ctrl Pts',(-4.1688734129079,-5.33036429028539,67.9859079355219));
#25644=CARTESIAN_POINT('Ctrl Pts',(-4.02236168477485,-5.44495098921068,
67.9946570807898));
#25645=CARTESIAN_POINT('Ctrl Pts',(-3.87112305634591,-5.55349359238653,
68.0034062260577));
#25646=CARTESIAN_POINT('Ctrl Pts',(-3.7156711731689,-5.6556234610237,68.0121553713256));
#25647=CARTESIAN_POINT('Ctrl Pts',(-3.56021980457478,-5.75775299158659,
68.0209044876318));
#25648=CARTESIAN_POINT('Ctrl Pts',(-3.40055544862585,-5.85346967275238,
68.0296536039379));
#25649=CARTESIAN_POINT('Ctrl Pts',(-3.2372203632362,-5.94244842803443,68.0384027202441));
#25650=CARTESIAN_POINT('Ctrl Pts',(-3.07388580496283,-6.03142689616354,
68.047151808315));
#25651=CARTESIAN_POINT('Ctrl Pts',(-2.90688079257962,-6.11366734484701,
68.0559008963859));
#25652=CARTESIAN_POINT('Ctrl Pts',(-2.73677251094889,-6.18889046787181,
68.0646499844569));
#25653=CARTESIAN_POINT('Ctrl Pts',(-2.56666476416927,-6.26411335438154,
68.0733990450191));
#25654=CARTESIAN_POINT('Ctrl Pts',(-2.39345402972383,-6.33231884350181,
68.0821481055814));
#25655=CARTESIAN_POINT('Ctrl Pts',(-2.21772856474336,-6.3932752962094,68.0908971661436));
#25656=CARTESIAN_POINT('Ctrl Pts',(-2.04200363768561,-6.4542315623199,68.0996461999236));
#25657=CARTESIAN_POINT('Ctrl Pts',(-1.86376426620378,-6.50793874251975,
68.1083952337036));
#25658=CARTESIAN_POINT('Ctrl Pts',(-1.68361578194965,-6.55421443796052,
68.1171442674836));
#25659=CARTESIAN_POINT('Ctrl Pts',(-1.50346783420135,-6.60048999558619,
68.1258932752078));
#25660=CARTESIAN_POINT('Ctrl Pts',(-1.32141106257502,-6.63933404145445,
68.1346422829321));
#25661=CARTESIAN_POINT('Ctrl Pts',(-1.13806375959289,-6.67061465526988,
68.1433912906563));
#25662=CARTESIAN_POINT('Ctrl Pts',(-0.954716987421232,-6.70189517852452,
68.1521402730512));
#25663=CARTESIAN_POINT('Ctrl Pts',(-0.770079973811584,-6.72561226535809,
68.1608892554461));
#25664=CARTESIAN_POINT('Ctrl Pts',(-0.584779770553788,-6.74168536939771,
68.169638237841));
#25665=CARTESIAN_POINT('Ctrl Pts',(-0.391490647555237,-6.75845143942386,
68.178764418517));
#25666=CARTESIAN_POINT('Ctrl Pts',(-0.197480213105655,-6.76689975924023,
68.1878905991931));
#25667=CARTESIAN_POINT('Ctrl Pts',(-0.003465326299107,-6.76699911271707,
68.1970167798692));
#25668=CARTESIAN_POINT('Ctrl Pts',(0.184486595294705,-6.76709536139777,
68.2058577673991));
#25669=CARTESIAN_POINT('Ctrl Pts',(0.372442378183841,-6.75935659726778,
68.214698754929));
#25670=CARTESIAN_POINT('Ctrl Pts',(0.559750217720661,-6.74380965729028,
68.2235397424589));
#25671=CARTESIAN_POINT('Ctrl Pts',(0.745129914456266,-6.7284227571727,68.2322897210567));
#25672=CARTESIAN_POINT('Ctrl Pts',(0.929874656312636,-6.70538772273494,
68.2410396996545));
#25673=CARTESIAN_POINT('Ctrl Pts',(1.11335688289617,-6.67478280180769,68.2497896782522));
#25674=CARTESIAN_POINT('Ctrl Pts',(1.29683723118696,-6.64417819418055,68.2585395672772));
#25675=CARTESIAN_POINT('Ctrl Pts',(1.47905480730075,-6.60600390230111,68.2672894563021));
#25676=CARTESIAN_POINT('Ctrl Pts',(1.65939064804648,-6.56038959797175,68.2760393453271));
#25677=CARTESIAN_POINT('Ctrl Pts',(1.83972470264112,-6.51477574543299,68.284789147688));
#25678=CARTESIAN_POINT('Ctrl Pts',(2.01817678125701,-6.46172209820146,68.293538950049));
#25679=CARTESIAN_POINT('Ctrl Pts',(2.19414072347539,-6.40140886724063,68.3022887524099));
#25680=CARTESIAN_POINT('Ctrl Pts',(2.37010298131958,-6.34109621361426,68.3110384710154));
#25681=CARTESIAN_POINT('Ctrl Pts',(2.54357687926777,-6.27352420826026,68.3197881896209));
#25682=CARTESIAN_POINT('Ctrl Pts',(2.71397317789837,-6.19892237325555,68.3285379082264));
#25683=CARTESIAN_POINT('Ctrl Pts',(2.88436790207068,-6.12432122757026,68.3372875459847));
#25684=CARTESIAN_POINT('Ctrl Pts',(3.05168482126123,-6.04269049717484,68.3460371837429));
#25685=CARTESIAN_POINT('Ctrl Pts',(3.21535561997257,-5.95430745235001,68.3547868215012));
#25686=CARTESIAN_POINT('Ctrl Pts',(3.37902496075149,-5.86592519481592,68.3635363813202));
#25687=CARTESIAN_POINT('Ctrl Pts',(3.53904799384745,-5.77079087940312,68.3722859411392));
#25688=CARTESIAN_POINT('Ctrl Pts',(3.69488118814855,-5.66922763747109,68.3810355009582));
#25689=CARTESIAN_POINT('Ctrl Pts',(3.85071304610708,-5.56766526649138,68.3897849857456));
#25690=CARTESIAN_POINT('Ctrl Pts',(4.00235489705847,-5.45967423580802,68.3985344705331));
#25691=CARTESIAN_POINT('Ctrl Pts',(4.14929168607538,-5.34562133936419,68.4072839553205));
#25692=CARTESIAN_POINT('Ctrl Pts',(4.29622726385643,-5.23156938308624,68.4160333679838));
#25693=CARTESIAN_POINT('Ctrl Pts',(4.43845763091956,-5.11145583677299,68.4247827806471));
#25694=CARTESIAN_POINT('Ctrl Pts',(4.57549970660854,-4.98568866204311,68.4335321933104));
#25695=CARTESIAN_POINT('Ctrl Pts',(4.71254069815183,-4.8599224822627,68.4422815367568));
#25696=CARTESIAN_POINT('Ctrl Pts',(4.84439326931198,-4.72850295734121,68.4510308802031));
#25697=CARTESIAN_POINT('Ctrl Pts',(4.97060959434579,-4.5918764422181,68.4597802236494));
#25698=CARTESIAN_POINT('Ctrl Pts',(5.096824962804,-4.45525096256795,68.4685295007857));
#25699=CARTESIAN_POINT('Ctrl Pts',(5.21740397615728,-4.3134187821846,68.477278777922));
#25700=CARTESIAN_POINT('Ctrl Pts',(5.33193710451827,-4.16686161438814,68.4860280550583));
#25701=CARTESIAN_POINT('Ctrl Pts',(5.4464694028928,-4.02030550864653,68.4947772687912));
#25702=CARTESIAN_POINT('Ctrl Pts',(5.55495572749567,-3.86902470980275,68.5035264825242));
#25703=CARTESIAN_POINT('Ctrl Pts',(5.65702762491362,-3.71353301465925,68.5122756962572));
#25704=CARTESIAN_POINT('Ctrl Pts',(5.75909881655069,-3.55804239467031,68.5210248494933));
#25705=CARTESIAN_POINT('Ctrl Pts',(5.85475551250706,-3.39834117619685,68.5297740027294));
#25706=CARTESIAN_POINT('Ctrl Pts',(5.94367283728026,-3.23497174692096,68.5385231559655));
#25707=CARTESIAN_POINT('Ctrl Pts',(6.03258957676254,-3.07160339301079,68.5472722516111));
#25708=CARTESIAN_POINT('Ctrl Pts',(6.11476689685237,-2.90456712829604,68.5560213472566));
#25709=CARTESIAN_POINT('Ctrl Pts',(6.18992570525223,-2.7344302447599,68.5647704429021));
#25710=CARTESIAN_POINT('Ctrl Pts',(6.26508404388672,-2.56429442463093,68.5735194838632));
#25711=CARTESIAN_POINT('Ctrl Pts',(6.33322384283301,-2.39105828656032,68.5822685248242));
#25712=CARTESIAN_POINT('Ctrl Pts',(6.39411368720027,-2.21531017132097,68.5910175657853));
#25713=CARTESIAN_POINT('Ctrl Pts',(6.45500317120888,-2.03956309619522,68.5997665549677));
#25714=CARTESIAN_POINT('Ctrl Pts',(6.50864269270074,-1.86130434438631,68.6085155441501));
#25715=CARTESIAN_POINT('Ctrl Pts',(6.55485008446336,-1.68113930719934,68.6172645333325));
#25716=CARTESIAN_POINT('Ctrl Pts',(6.60199664749406,-1.4973123921183,68.6261913468619));
#25717=CARTESIAN_POINT('Ctrl Pts',(6.64140563640908,-1.31150116499662,68.6351181603912));
#25718=CARTESIAN_POINT('Ctrl Pts',(6.67293772282174,-1.12436255155652,68.6440449739206));
#25719=CARTESIAN_POINT('Ctrl Pts',(6.70384494949872,-0.940932395051262,
68.6527948880761));
#25720=CARTESIAN_POINT('Ctrl Pts',(6.72718449348931,-0.756227260506631,
68.6615448022316));
#25721=CARTESIAN_POINT('Ctrl Pts',(6.74287707373933,-0.570874564541605,
68.6702947163872));
#25722=CARTESIAN_POINT('Ctrl Pts',(6.7585693453867,-0.38552551363247,68.6790444584712));
#25723=CARTESIAN_POINT('Ctrl Pts',(6.76661493004103,-0.199529212418304,
68.6877942005551));
#25724=CARTESIAN_POINT('Ctrl Pts',(6.76698649908907,-0.0135174386005844,
68.6965439426391));
#25725=CARTESIAN_POINT('Ctrl Pts',(6.7673580613239,0.172490924445634,68.705293524285));
#25726=CARTESIAN_POINT('Ctrl Pts',(6.7600558889629,0.358514472901276,68.7140431059309));
#25727=CARTESIAN_POINT('Ctrl Pts',(6.74510478454585,0.543921359662094,68.7227926875768));
#25728=CARTESIAN_POINT('Ctrl Pts',(6.73015393440688,0.729325093150383,68.7315421204158));
#25729=CARTESIAN_POINT('Ctrl Pts',(6.70755443556897,0.914111900256345,68.7402915532549));
#25730=CARTESIAN_POINT('Ctrl Pts',(6.67738304682318,1.09765415591543,68.7490409860939));
#25731=CARTESIAN_POINT('Ctrl Pts',(6.64721213111858,1.28119353391286,68.7577902817552));
#25732=CARTESIAN_POINT('Ctrl Pts',(6.6094696095549,1.46348811672673,68.7665395774166));
#25733=CARTESIAN_POINT('Ctrl Pts',(6.56428366991176,1.6439187634825,68.7752888730779));
#25734=CARTESIAN_POINT('Ctrl Pts',(6.51909837867709,1.82434682109747,68.7840380431887));
#25735=CARTESIAN_POINT('Ctrl Pts',(6.46646995271911,2.00291071820479,68.7927872132996));
#25736=CARTESIAN_POINT('Ctrl Pts',(6.40657713281536,2.17900400212741,68.8015363834104));
#25737=CARTESIAN_POINT('Ctrl Pts',(6.34668509279046,2.35509499309694,68.8102854395962));
#25738=CARTESIAN_POINT('Ctrl Pts',(6.27952894037512,2.52871516398158,68.8190344957819));
#25739=CARTESIAN_POINT('Ctrl Pts',(6.20533675061432,2.69927486771453,68.8277835519677));
#25740=CARTESIAN_POINT('Ctrl Pts',(6.12832117907903,2.87632521635952,68.83686555325));
#25741=CARTESIAN_POINT('Ctrl Pts',(6.04372366626067,3.05007728920021,68.8459475545323));
#25742=CARTESIAN_POINT('Ctrl Pts',(5.95185378007858,3.21989527478214,68.8550295558145));
#25743=CARTESIAN_POINT('Ctrl Pts',(5.86334450817363,3.38350129286766,68.8637793361217));
#25744=CARTESIAN_POINT('Ctrl Pts',(5.76808562057249,3.54345567124972,68.8725291164288));
#25745=CARTESIAN_POINT('Ctrl Pts',(5.6664006880448,3.69921508465315,68.8812788967359));
#25746=CARTESIAN_POINT('Ctrl Pts',(5.5647194110792,3.85496889852289,68.8900283624894));
#25747=CARTESIAN_POINT('Ctrl Pts',(5.4566127081511,4.00652780919642,68.8987778282429));
#25748=CARTESIAN_POINT('Ctrl Pts',(5.34244776449111,4.15337704569234,68.9075272939964));
#25749=CARTESIAN_POINT('Ctrl Pts',(5.22828631819588,4.30022178356258,68.9162764917159));
#25750=CARTESIAN_POINT('Ctrl Pts',(5.10806717844059,4.44235690972691,68.9250256894355));
#25751=CARTESIAN_POINT('Ctrl Pts',(4.98219864544705,4.5792996907066,68.9337748871551));
#25752=CARTESIAN_POINT('Ctrl Pts',(4.85633329944003,4.71623900430024,68.9425238633454));
#25753=CARTESIAN_POINT('Ctrl Pts',(4.72481904033618,4.84798602483647,68.9512728395356));
#25754=CARTESIAN_POINT('Ctrl Pts',(4.58810250737159,4.97409332259162,68.9600218157259));
#25755=CARTESIAN_POINT('Ctrl Pts',(4.45137708685601,5.10020881822171,68.968771360662));
#25756=CARTESIAN_POINT('Ctrl Pts',(4.30944892636009,5.22068366307968,68.9775209055982));
#25757=CARTESIAN_POINT('Ctrl Pts',(4.16280009466617,5.33510865604885,68.9862704505344));
#25758=CARTESIAN_POINT('Ctrl Pts',(4.0161598834874,5.44952692272927,68.9950194811427));
#25759=CARTESIAN_POINT('Ctrl Pts',(3.86479978232178,5.55789587288663,69.003768511751));
#25760=CARTESIAN_POINT('Ctrl Pts',(3.7092338358101,5.65984746713915,69.0125175423592));
#25761=CARTESIAN_POINT('Ctrl Pts',(3.55366577799474,5.76180044505424,69.0212666917073));
#25762=CARTESIAN_POINT('Ctrl Pts',(3.39389200026765,5.85733573571103,69.0300158410553));
#25763=CARTESIAN_POINT('Ctrl Pts',(3.23045513625957,5.94612887621974,69.0387649904033));
#25764=CARTESIAN_POINT('Ctrl Pts',(3.18695122151521,5.96976399206718,69.0410938545163));
#25765=CARTESIAN_POINT('Ctrl Pts',(3.14318791262635,5.99292165435348,69.0434227186292));
#25766=CARTESIAN_POINT('Ctrl Pts',(3.09917575053258,6.0155962852664,69.0457515827422));
#25767=CARTESIAN_POINT('Ctrl Pts',(3.09917575053264,6.01559628526636,67.0455611218465));
#25768=CARTESIAN_POINT('Ctrl Pts',(2.94392938397932,6.09557767892451,67.0537718920013));
#25769=CARTESIAN_POINT('Ctrl Pts',(2.78569628280582,6.16948810613674,67.0619826621561));
#25770=CARTESIAN_POINT('Ctrl Pts',(2.62499755773111,6.23712087600567,67.0701934323109));
#25771=CARTESIAN_POINT('Ctrl Pts',(2.46419199460855,6.30479861046969,67.0784096612686));
#25772=CARTESIAN_POINT('Ctrl Pts',(2.30091787514996,6.36619024349981,67.0866258902262));
#25773=CARTESIAN_POINT('Ctrl Pts',(2.13571210467178,6.42113874682353,67.0948421191838));
#25774=CARTESIAN_POINT('Ctrl Pts',(1.97029709898946,6.47615684312379,67.1030687540997));
#25775=CARTESIAN_POINT('Ctrl Pts',(1.8029459010291,6.52471541889638,67.1112953890155));
#25776=CARTESIAN_POINT('Ctrl Pts',(1.63420697239288,6.5667081990433,67.1195220239313));
#25777=CARTESIAN_POINT('Ctrl Pts',(1.61171377658031,6.5723059104558,67.1206186488272));
#25778=CARTESIAN_POINT('Ctrl Pts',(1.58919593090922,6.57778702714842,67.121715273723));
#25779=CARTESIAN_POINT('Ctrl Pts',(1.5666547419559,6.58315136689922,67.1228118986189));
#25780=CARTESIAN_POINT('Ctrl Pts',(1.3975925030413,6.62338470554202,67.131036746941));
#25781=CARTESIAN_POINT('Ctrl Pts',(1.22674213922248,6.65715778207088,67.1392615952631));
#25782=CARTESIAN_POINT('Ctrl Pts',(1.05463850430982,6.68431197844828,67.1474864435852));
#25783=CARTESIAN_POINT('Ctrl Pts',(0.882728696248987,6.71143559317991,67.1557020289045));
#25784=CARTESIAN_POINT('Ctrl Pts',(0.709568778831039,6.73195511582117,67.1639176142237));
#25785=CARTESIAN_POINT('Ctrl Pts',(0.535707054474028,6.74576214758472,67.172133199543));
#25786=CARTESIAN_POINT('Ctrl Pts',(0.362006204685331,6.75955640367678,67.1803411829663));
#25787=CARTESIAN_POINT('Ctrl Pts',(0.187605196610105,6.76665051016176,67.1885491663896));
#25788=CARTESIAN_POINT('Ctrl Pts',(0.0130608670671646,6.76698739571395,
67.1967571498129));
#25789=CARTESIAN_POINT('Ctrl Pts',(-0.161357014407913,6.76732403721051,
67.2049591869895));
#25790=CARTESIAN_POINT('Ctrl Pts',(-0.335917653226478,6.76091320749244,
67.2131612241661));
#25791=CARTESIAN_POINT('Ctrl Pts',(-0.510060678331711,6.74774978080988,
67.2213632613427));
#25792=CARTESIAN_POINT('Ctrl Pts',(-0.684112515557719,6.73459324699577,
67.2295610036222));
#25793=CARTESIAN_POINT('Ctrl Pts',(-0.857746817808679,6.71469118730537,
67.2377587459017));
#25794=CARTESIAN_POINT('Ctrl Pts',(-1.03040471682381,6.68809054361163,67.2459564881812));
#25795=CARTESIAN_POINT('Ctrl Pts',(-1.20302978779612,6.66149495759017,67.2541526717956));
#25796=CARTESIAN_POINT('Ctrl Pts',(-1.37467847013956,6.62820337287994,67.2623488554101));
#25797=CARTESIAN_POINT('Ctrl Pts',(-1.54479820349252,6.58831446657537,67.2705450390245));
#25798=CARTESIAN_POINT('Ctrl Pts',(-1.71490541365946,6.54842849665086,67.2787406192854));
#25799=CARTESIAN_POINT('Ctrl Pts',(-1.88348354943207,6.50194625336897,67.2869361995464));
#25800=CARTESIAN_POINT('Ctrl Pts',(-2.04999146898421,6.44901728770299,67.2951317798074));
#25801=CARTESIAN_POINT('Ctrl Pts',(-2.21651742537692,6.39608258854806,67.3033282478482));
#25802=CARTESIAN_POINT('Ctrl Pts',(-2.38097237672716,6.33669988443642,67.3115247158889));
#25803=CARTESIAN_POINT('Ctrl Pts',(-2.5428314909209,6.27106825100644,67.3197211839297));
#25804=CARTESIAN_POINT('Ctrl Pts',(-2.70473758685117,6.20541756713173,67.3279200311032));
#25805=CARTESIAN_POINT('Ctrl Pts',(-2.86404601234771,6.13351447581643,67.3361188782766));
#25806=CARTESIAN_POINT('Ctrl Pts',(-3.02025297689143,6.05560574637901,67.3443177254501));
#25807=CARTESIAN_POINT('Ctrl Pts',(-3.17662319290361,5.97761559474301,67.3525251412161));
#25808=CARTESIAN_POINT('Ctrl Pts',(-3.32988515067514,5.89360742577439,67.3607325569822));
#25809=CARTESIAN_POINT('Ctrl Pts',(-3.47955981218855,5.80387392294168,67.3689399727482));
#25810=CARTESIAN_POINT('Ctrl Pts',(-3.62931469405645,5.71409232610739,67.3771517874004));
#25811=CARTESIAN_POINT('Ctrl Pts',(-3.77547814668973,5.61857947422762,67.3853636020527));
#25812=CARTESIAN_POINT('Ctrl Pts',(-3.91760119818977,5.51767069078448,67.3935754167049));
#25813=CARTESIAN_POINT('Ctrl Pts',(-4.059933547489,5.41661330381735,67.4017993245026));
#25814=CARTESIAN_POINT('Ctrl Pts',(-4.19821332021664,5.31014432368578,67.4100232323003));
#25815=CARTESIAN_POINT('Ctrl Pts',(-4.33202464246535,5.19863938902026,67.418247140098));
#25816=CARTESIAN_POINT('Ctrl Pts',(-4.4556638329424,5.09561088870684,67.4258458790206));
#25817=CARTESIAN_POINT('Ctrl Pts',(-4.57548834913575,4.98828355846426,67.4334446179433));
#25818=CARTESIAN_POINT('Ctrl Pts',(-4.69119948508499,4.87698025330617,67.441043356866));
#25819=CARTESIAN_POINT('Ctrl Pts',(-4.81349361404285,4.75934472373701,67.4490744002923));
#25820=CARTESIAN_POINT('Ctrl Pts',(-4.93157806935784,4.63689647249755,67.4571054437187));
#25821=CARTESIAN_POINT('Ctrl Pts',(-5.04503820716544,4.50997544208845,67.4651364871451));
#25822=CARTESIAN_POINT('Ctrl Pts',(-5.15836481398825,4.38320378475882,67.4731580788543));
#25823=CARTESIAN_POINT('Ctrl Pts',(-5.26707768355398,4.25197009973112,67.4811796705635));
#25824=CARTESIAN_POINT('Ctrl Pts',(-5.37079616114844,4.11665368902865,67.4892012622726));
#25825=CARTESIAN_POINT('Ctrl Pts',(-5.47441571004999,3.98146634573971,67.4972152028323));
#25826=CARTESIAN_POINT('Ctrl Pts',(-5.57305011945073,3.84220432322443,67.5052291433919));
#25827=CARTESIAN_POINT('Ctrl Pts',(-5.66635657107553,3.69928266146684,67.5132430839515));
#25828=CARTESIAN_POINT('Ctrl Pts',(-5.75958926685771,3.55647397482947,67.5212506897408));
#25829=CARTESIAN_POINT('Ctrl Pts',(-5.84750218570977,3.41001172319943,67.5292582955302));
#25830=CARTESIAN_POINT('Ctrl Pts',(-5.92979385145621,3.26034260151171,67.5372659013195));
#25831=CARTESIAN_POINT('Ctrl Pts',(-6.01204998303797,3.11073810808457,67.545270049364));
#25832=CARTESIAN_POINT('Ctrl Pts',(-6.08868950917054,2.95792982886514,67.5532741974085));
#25833=CARTESIAN_POINT('Ctrl Pts',(-6.15945519598822,2.8023919584194,67.561278345453));
#25834=CARTESIAN_POINT('Ctrl Pts',(-6.23020456345916,2.64688995671955,67.5692806476528));
#25835=CARTESIAN_POINT('Ctrl Pts',(-6.29508263136301,2.48865995930421,67.5772829498525));
#25836=CARTESIAN_POINT('Ctrl Pts',(-6.35387900112164,2.32819901192006,67.5852852520523));
#25837=CARTESIAN_POINT('Ctrl Pts',(-6.41267363960505,2.16774278935247,67.5932873186222));
#25838=CARTESIAN_POINT('Ctrl Pts',(-6.46538680803414,2.00505610189901,67.601289385192));
#25839=CARTESIAN_POINT('Ctrl Pts',(-6.51185703421414,1.8406539506262,67.6092914517618));
#25840=CARTESIAN_POINT('Ctrl Pts',(-6.55835314632055,1.67616022024263,67.6172979758289));
#25841=CARTESIAN_POINT('Ctrl Pts',(-6.59859926635847,1.50994948013485,67.625304499896));
#25842=CARTESIAN_POINT('Ctrl Pts',(-6.6324842955872,1.34255021090059,67.6333110239631));
#25843=CARTESIAN_POINT('Ctrl Pts',(-6.66637931588397,1.17510158365994,67.6413199087697));
#25844=CARTESIAN_POINT('Ctrl Pts',(-6.6939094467974,1.00646410080563,67.6493287935762));
#25845=CARTESIAN_POINT('Ctrl Pts',(-6.71501519550499,0.837173771768535,
67.6573376783828));
#25846=CARTESIAN_POINT('Ctrl Pts',(-6.73614212232804,0.667713571944716,
67.6653545995348));
#25847=CARTESIAN_POINT('Ctrl Pts',(-6.75083175893498,0.497599592758307,
67.6733715206868));
#25848=CARTESIAN_POINT('Ctrl Pts',(-6.75907666069919,0.327370882626328,
67.6813884418388));
#25849=CARTESIAN_POINT('Ctrl Pts',(-6.76436225982512,0.218241538552459,
67.686527888329));
#25850=CARTESIAN_POINT('Ctrl Pts',(-6.7670002793358,0.109065054824402,67.6916673348192));
#25851=CARTESIAN_POINT('Ctrl Pts',(-6.76699999997781,-1.73301632199464E-5,
67.6968067813093));
#25852=CARTESIAN_POINT('',(-6.767,7.47259830383148E-10,67.3028202161548));
#25853=CARTESIAN_POINT('Ctrl Pts',(3.09917575053252,6.01559628526643,66.6513920151221));
#25854=CARTESIAN_POINT('Ctrl Pts',(2.93382384459251,6.10078395293766,66.6601414630345));
#25855=CARTESIAN_POINT('Ctrl Pts',(2.76495772122964,6.17915010267058,66.6688909109469));
#25856=CARTESIAN_POINT('Ctrl Pts',(2.59315093316685,6.25042856433188,66.6776403588593));
#25857=CARTESIAN_POINT('Ctrl Pts',(2.42134553245595,6.3217064504146,66.6863897361193));
#25858=CARTESIAN_POINT('Ctrl Pts',(2.24659977927572,6.38589665313464,66.6951391133793));
#25859=CARTESIAN_POINT('Ctrl Pts',(2.06950718689904,6.4427811543908,66.7038884906393));
#25860=CARTESIAN_POINT('Ctrl Pts',(1.89241596572839,6.49966521519731,66.712637800154));
#25861=CARTESIAN_POINT('Ctrl Pts',(1.71297821457167,6.54924360009554,66.7213871096686));
#25862=CARTESIAN_POINT('Ctrl Pts',(1.53180337335805,6.59134792173565,66.7301364191833));
#25863=CARTESIAN_POINT('Ctrl Pts',(1.35062987477742,6.63345193135313,66.7388856638594));
#25864=CARTESIAN_POINT('Ctrl Pts',(1.1677195910291,6.66808192368245,66.7476349085355));
#25865=CARTESIAN_POINT('Ctrl Pts',(0.983693746906412,6.69512028363175,66.7563841532116));
#25866=CARTESIAN_POINT('Ctrl Pts',(0.799669205419417,6.72215845218872,66.7651333359558));
#25867=CARTESIAN_POINT('Ctrl Pts',(0.614529402873001,6.74160505424583,66.7738825187));
#25868=CARTESIAN_POINT('Ctrl Pts',(0.428903127362753,6.75339404354125,66.7826317014442));
#25869=CARTESIAN_POINT('Ctrl Pts',(0.243278104163323,6.76518295330332,66.7913808251628));
#25870=CARTESIAN_POINT('Ctrl Pts',(0.0571669005385001,6.76931433552276,
66.8001299488814));
#25871=CARTESIAN_POINT('Ctrl Pts',(-0.12879840477819,6.76577415902472,66.8088790726));
#25872=CARTESIAN_POINT('Ctrl Pts',(-0.314762517259757,6.76223400523438,
66.8176281401992));
#25873=CARTESIAN_POINT('Ctrl Pts',(-0.50058044682015,6.75102239665084,66.8263772077984));
#25874=CARTESIAN_POINT('Ctrl Pts',(-0.685621118843231,6.73217741012491,
66.8351262753976));
#25875=CARTESIAN_POINT('Ctrl Pts',(-0.870660665415269,6.71333253821762,
66.8438752897834));
#25876=CARTESIAN_POINT('Ctrl Pts',(-1.0549226788558,6.68685441030598,66.8526243041692));
#25877=CARTESIAN_POINT('Ctrl Pts',(-1.23778137635361,6.65283295028157,66.861373318555));
#25878=CARTESIAN_POINT('Ctrl Pts',(-1.42999922977429,6.61707018862126,66.8705701289217));
#25879=CARTESIAN_POINT('Ctrl Pts',(-1.62066601230776,6.57297172935087,66.8797669392883));
#25880=CARTESIAN_POINT('Ctrl Pts',(-1.80906628496005,6.52070304312509,66.888963749655));
#25881=CARTESIAN_POINT('Ctrl Pts',(-1.98831342541176,6.47097374916367,66.8977137473928));
#25882=CARTESIAN_POINT('Ctrl Pts',(-2.16550875892385,6.41384933990986,66.9064637451305));
#25883=CARTESIAN_POINT('Ctrl Pts',(-2.34005036709733,6.34952386242052,66.9152137428683));
#25884=CARTESIAN_POINT('Ctrl Pts',(-2.51458843542848,6.28519968950292,66.9239635631491));
#25885=CARTESIAN_POINT('Ctrl Pts',(-2.68647261713858,6.21367483972914,66.93271338343));
#25886=CARTESIAN_POINT('Ctrl Pts',(-2.85511905904581,6.13519226745775,66.9414632037109));
#25887=CARTESIAN_POINT('Ctrl Pts',(-3.02376230484788,6.05671118254982,66.9502128581694));
#25888=CARTESIAN_POINT('Ctrl Pts',(-3.18916767375867,5.97127275994789,66.9589625126279));
#25889=CARTESIAN_POINT('Ctrl Pts',(-3.35077334098813,5.87916720440262,66.9677121670865));
#25890=CARTESIAN_POINT('Ctrl Pts',(-3.51237616033454,5.78706327198018,66.9764616673549));
#25891=CARTESIAN_POINT('Ctrl Pts',(-3.67017916298451,5.68829258364782,66.9852111676233));
#25892=CARTESIAN_POINT('Ctrl Pts',(-3.82364636562683,5.5831906174363,66.9939606678918));
#25893=CARTESIAN_POINT('Ctrl Pts',(-3.97711106775081,5.478090363704,67.0027100256002));
#25894=CARTESIAN_POINT('Ctrl Pts',(-4.12623987478277,5.36665920046031,67.0114593833086));
#25895=CARTESIAN_POINT('Ctrl Pts',(-4.27052628210351,5.24927559515246,67.0202087410171));
#25896=CARTESIAN_POINT('Ctrl Pts',(-4.41481053021487,5.1318937464604,67.0289579677936));
#25897=CARTESIAN_POINT('Ctrl Pts',(-4.5542523013313,5.00855981480445,67.0377071945701));
#25898=CARTESIAN_POINT('Ctrl Pts',(-4.68837800627241,4.87969268195253,67.0464564213466));
#25899=CARTESIAN_POINT('Ctrl Pts',(-4.82250188225663,4.75082730635089,67.0552055288175));
#25900=CARTESIAN_POINT('Ctrl Pts',(-4.95130963049816,4.61642907906904,67.0639546362883));
#25901=CARTESIAN_POINT('Ctrl Pts',(-5.07436379030302,4.47695444735164,67.0727037437591));
#25902=CARTESIAN_POINT('Ctrl Pts',(-5.19741643559869,4.33748153224107,67.0814527435489));
#25903=CARTESIAN_POINT('Ctrl Pts',(-5.31471544459966,4.1929325525815,67.0902017433387));
#25904=CARTESIAN_POINT('Ctrl Pts',(-5.42586245272949,4.04379841783197,67.0989507431285));
#25905=CARTESIAN_POINT('Ctrl Pts',(-5.53702160016571,3.89464799488013,67.1077006984706));
#25906=CARTESIAN_POINT('Ctrl Pts',(-5.6420272307877,3.74091164447592,67.1164506538128));
#25907=CARTESIAN_POINT('Ctrl Pts',(-5.74052265230589,3.58311159167043,67.1252006091549));
#25908=CARTESIAN_POINT('Ctrl Pts',(-5.83901427064644,3.42531763195659,67.1339502266374));
#25909=CARTESIAN_POINT('Ctrl Pts',(-5.93099603113573,3.26346052699549,67.1426998441198));
#25910=CARTESIAN_POINT('Ctrl Pts',(-6.01615550620697,3.0980900447107,67.1514494616023));
#25911=CARTESIAN_POINT('Ctrl Pts',(-6.10131214576855,2.93272506867873,67.1601987877534));
#25912=CARTESIAN_POINT('Ctrl Pts',(-6.17964682326917,2.76384720420987,67.1689481139045));
#25913=CARTESIAN_POINT('Ctrl Pts',(-6.25089348286849,2.59203002795728,67.1776974400556));
#25914=CARTESIAN_POINT('Ctrl Pts',(-6.32213814887732,2.42021765941204,67.1864465213871));
#25915=CARTESIAN_POINT('Ctrl Pts',(-6.38629508411105,2.24546640836128,67.1951956027187));
#25916=CARTESIAN_POINT('Ctrl Pts',(-6.4431463981845,2.06836976664282,67.2039446840503));
#25917=CARTESIAN_POINT('Ctrl Pts',(-6.50000285282457,1.8912571116255,67.2126945564847));
#25918=CARTESIAN_POINT('Ctrl Pts',(-6.54955227672125,1.71179891444558,67.2214444289191));
#25919=CARTESIAN_POINT('Ctrl Pts',(-6.5916263592538,1.53060476282758,67.2301943013535));
#25920=CARTESIAN_POINT('Ctrl Pts',(-6.63369752054311,1.34942319169048,67.238943566276));
#25921=CARTESIAN_POINT('Ctrl Pts',(-6.66829431423489,1.16650618647076,67.2476928311985));
#25922=CARTESIAN_POINT('Ctrl Pts',(-6.69529923744774,0.982474997662425,
67.256442096121));
#25923=CARTESIAN_POINT('Ctrl Pts',(-6.72230554730919,0.798434359221862,
67.2651918103007));
#25924=CARTESIAN_POINT('Ctrl Pts',(-6.741719164963,0.613279706284663,67.2739415244804));
#25925=CARTESIAN_POINT('Ctrl Pts',(-6.75347414816993,0.427639953699858,
67.2826912386601));
#25926=CARTESIAN_POINT('Ctrl Pts',(-6.7624883775708,0.285283364476322,67.289400897825));
#25927=CARTESIAN_POINT('Ctrl Pts',(-6.76699999998425,0.142641701617036,
67.2961105569899));
#25928=CARTESIAN_POINT('Ctrl Pts',(-6.767,7.4716449424778E-10,67.3028202161548));
#25929=CARTESIAN_POINT('Ctrl Pts',(-6.767,3.03919765936208E-12,67.3028202161898));
#25930=CARTESIAN_POINT('Ctrl Pts',(-6.76700000000008,-0.186007249412693,
67.3115697279958));
#25931=CARTESIAN_POINT('Ctrl Pts',(-6.75932637295454,-0.372014355524604,
67.3203192398017));
#25932=CARTESIAN_POINT('Ctrl Pts',(-6.74400518266952,-0.557389537152179,
67.3290687516077));
#25933=CARTESIAN_POINT('Ctrl Pts',(-6.72868405709675,-0.74276393580879,
67.3378182264582));
#25934=CARTESIAN_POINT('Ctrl Pts',(-6.70571545653024,-0.927506129692694,
67.3465677013088));
#25935=CARTESIAN_POINT('Ctrl Pts',(-6.67517739415685,-1.11098863924768,
67.3553171761593));
#25936=CARTESIAN_POINT('Ctrl Pts',(-6.64463945823104,-1.29447038906488,
67.3640666147813));
#25937=CARTESIAN_POINT('Ctrl Pts',(-6.60653217027155,-1.47669218228232,
67.3728160534033));
#25938=CARTESIAN_POINT('Ctrl Pts',(-6.56098496116701,-1.65703510504165,
67.3815654920253));
#25939=CARTESIAN_POINT('Ctrl Pts',(-6.51543793687498,-1.8373772960409,67.3903148951456));
#25940=CARTESIAN_POINT('Ctrl Pts',(-6.4624511220261,-2.01584035397147,67.3990642982658));
#25941=CARTESIAN_POINT('Ctrl Pts',(-6.40220448416202,-2.19181813638262,
67.407813701386));
#25942=CARTESIAN_POINT('Ctrl Pts',(-6.34195808575139,-2.36779521936074,
67.4165630697313));
#25943=CARTESIAN_POINT('Ctrl Pts',(-6.27445201489178,-2.54128677544969,
67.4253124380766));
#25944=CARTESIAN_POINT('Ctrl Pts',(-6.19991555136117,-2.71170355237994,
67.4340618064219));
#25945=CARTESIAN_POINT('Ctrl Pts',(-6.1253793778897,-2.88211966613217,67.4428111407189));
#25946=CARTESIAN_POINT('Ctrl Pts',(-6.04381298133548,-3.04946076210581,
67.451560475016));
#25947=CARTESIAN_POINT('Ctrl Pts',(-5.95549339426237,-3.21315848206982,
67.460309809313));
#25948=CARTESIAN_POINT('Ctrl Pts',(-5.86717414355091,-3.37685557859757,
67.4690591102886));
#25949=CARTESIAN_POINT('Ctrl Pts',(-5.77210188986168,-3.53690907467426,
67.4778084112641));
#25950=CARTESIAN_POINT('Ctrl Pts',(-5.67059953466998,-3.69277536785013,
67.4865577122397));
#25951=CARTESIAN_POINT('Ctrl Pts',(-5.569097557617,-3.84864108035887,67.4953069806205));
#25952=CARTESIAN_POINT('Ctrl Pts',(-5.46116568338011,-4.00031938104359,
67.5040562490012));
#25953=CARTESIAN_POINT('Ctrl Pts',(-5.34717048686063,-4.14729511663285,
67.512805517382));
#25954=CARTESIAN_POINT('Ctrl Pts',(-5.23317570555466,-4.29427031688103,
67.5215547538946));
#25955=CARTESIAN_POINT('Ctrl Pts',(-5.11311782178753,-4.43654275987189,
67.5303039904072));
#25956=CARTESIAN_POINT('Ctrl Pts',(-4.98740459171963,-4.57362924147705,
67.5390532269198));
#25957=CARTESIAN_POINT('Ctrl Pts',(-4.86169180910784,-4.71071523514483,
67.547802432291));
#25958=CARTESIAN_POINT('Ctrl Pts',(-4.73032391415391,-4.84261509316563,
67.5565516376621));
#25959=CARTESIAN_POINT('Ctrl Pts',(-4.59374707237259,-4.96888084331555,
67.5653008430332));
#25960=CARTESIAN_POINT('Ctrl Pts',(-4.45717070537371,-5.09514615452751,
67.5740500179894));
#25961=CARTESIAN_POINT('Ctrl Pts',(-4.31538563819482,-5.21577720253655,
67.5827991929456));
#25962=CARTESIAN_POINT('Ctrl Pts',(-4.16887341290624,-5.33036429028668,
67.5915483679019));
#25963=CARTESIAN_POINT('Ctrl Pts',(-4.02236168477337,-5.44495098921177,
67.6002975131697));
#25964=CARTESIAN_POINT('Ctrl Pts',(-3.87112305634461,-5.55349359238743,
67.6090466584377));
#25965=CARTESIAN_POINT('Ctrl Pts',(-3.71567117316779,-5.65562346102443,
67.6177958037056));
#25966=CARTESIAN_POINT('Ctrl Pts',(-3.56021980457348,-5.7577529915874,67.6265449200117));
#25967=CARTESIAN_POINT('Ctrl Pts',(-3.40055544862437,-5.85346967275325,
67.6352940363179));
#25968=CARTESIAN_POINT('Ctrl Pts',(-3.23722036323453,-5.94244842803534,
67.6440431526241));
#25969=CARTESIAN_POINT('Ctrl Pts',(-3.07388580496107,-6.03142689616444,
67.652792240695));
#25970=CARTESIAN_POINT('Ctrl Pts',(-2.90688079257778,-6.11366734484788,
67.6615413287659));
#25971=CARTESIAN_POINT('Ctrl Pts',(-2.73677251094698,-6.18889046787265,
67.6702904168369));
#25972=CARTESIAN_POINT('Ctrl Pts',(-2.56666476416739,-6.26411335438231,
67.6790394773991));
#25973=CARTESIAN_POINT('Ctrl Pts',(-2.39345402972199,-6.3323188435025,67.6877885379613));
#25974=CARTESIAN_POINT('Ctrl Pts',(-2.21772856474156,-6.39327529621002,
67.6965375985235));
#25975=CARTESIAN_POINT('Ctrl Pts',(-2.04200363768404,-6.45423156232039,
67.7052866323035));
#25976=CARTESIAN_POINT('Ctrl Pts',(-1.86376426620244,-6.50793874252012,
67.7140356660835));
#25977=CARTESIAN_POINT('Ctrl Pts',(-1.68361578194855,-6.5542144379608,67.7227846998635));
#25978=CARTESIAN_POINT('Ctrl Pts',(-1.50346783420042,-6.6004899955864,67.7315337075878));
#25979=CARTESIAN_POINT('Ctrl Pts',(-1.32141106257428,-6.63933404145459,
67.740282715312));
#25980=CARTESIAN_POINT('Ctrl Pts',(-1.13806375959234,-6.67061465526997,
67.7490317230362));
#25981=CARTESIAN_POINT('Ctrl Pts',(-0.954716987421247,-6.7018951785245,
67.7577807054311));
#25982=CARTESIAN_POINT('Ctrl Pts',(-0.770079973812172,-6.72561226535801,
67.766529687826));
#25983=CARTESIAN_POINT('Ctrl Pts',(-0.584779770554954,-6.7416853693976,
67.7752786702208));
#25984=CARTESIAN_POINT('Ctrl Pts',(-0.391490647556406,-6.75845143942379,
67.7844048508969));
#25985=CARTESIAN_POINT('Ctrl Pts',(-0.197480213106823,-6.76689975924019,
67.793531031573));
#25986=CARTESIAN_POINT('Ctrl Pts',(-0.0034653263002745,-6.76699911271707,
67.802657212249));
#25987=CARTESIAN_POINT('Ctrl Pts',(0.184486595293601,-6.7670953613978,67.8114981997789));
#25988=CARTESIAN_POINT('Ctrl Pts',(0.3724423781828,-6.75935659726783,67.8203391873089));
#25989=CARTESIAN_POINT('Ctrl Pts',(0.559750217719686,-6.74380965729036,
67.8291801748388));
#25990=CARTESIAN_POINT('Ctrl Pts',(0.745129914455358,-6.7284227571728,67.8379301534365));
#25991=CARTESIAN_POINT('Ctrl Pts',(0.929874656311797,-6.70538772273506,
67.8466801320343));
#25992=CARTESIAN_POINT('Ctrl Pts',(1.1133568828954,-6.67478280180782,67.8554301106321));
#25993=CARTESIAN_POINT('Ctrl Pts',(1.29683723118625,-6.64417819418069,67.864179999657));
#25994=CARTESIAN_POINT('Ctrl Pts',(1.47905480730011,-6.60600390230125,67.872929888682));
#25995=CARTESIAN_POINT('Ctrl Pts',(1.65939064804591,-6.56038959797189,67.8816797777069));
#25996=CARTESIAN_POINT('Ctrl Pts',(1.83972470264048,-6.51477574543317,67.8904295800679));
#25997=CARTESIAN_POINT('Ctrl Pts',(2.01817678125632,-6.46172209820167,67.8991793824288));
#25998=CARTESIAN_POINT('Ctrl Pts',(2.19414072347464,-6.40140886724088,67.9079291847898));
#25999=CARTESIAN_POINT('Ctrl Pts',(2.37010298131884,-6.34109621361454,67.9166789033953));
#26000=CARTESIAN_POINT('Ctrl Pts',(2.54357687926704,-6.27352420826056,67.9254286220007));
#26001=CARTESIAN_POINT('Ctrl Pts',(2.71397317789765,-6.19892237325586,67.9341783406062));
#26002=CARTESIAN_POINT('Ctrl Pts',(2.88436790207003,-6.12432122757057,67.9429279783645));
#26003=CARTESIAN_POINT('Ctrl Pts',(3.05168482126065,-6.04269049717514,67.9516776161228));
#26004=CARTESIAN_POINT('Ctrl Pts',(3.21535561997204,-5.95430745235029,67.960427253881));
#26005=CARTESIAN_POINT('Ctrl Pts',(3.37902496075098,-5.86592519481622,67.9691768137));
#26006=CARTESIAN_POINT('Ctrl Pts',(3.53904799384694,-5.77079087940343,67.9779263735191));
#26007=CARTESIAN_POINT('Ctrl Pts',(3.69488118814805,-5.66922763747141,67.9866759333381));
#26008=CARTESIAN_POINT('Ctrl Pts',(3.85071304610654,-5.56766526649176,67.9954254181255));
#26009=CARTESIAN_POINT('Ctrl Pts',(4.00235489705789,-5.45967423580845,68.0041749029129));
#26010=CARTESIAN_POINT('Ctrl Pts',(4.14929168607475,-5.34562133936467,68.0129243877004));
#26011=CARTESIAN_POINT('Ctrl Pts',(4.29622726385583,-5.23156938308674,68.0216738003637));
#26012=CARTESIAN_POINT('Ctrl Pts',(4.43845763091897,-5.1114558367735,68.030423213027));
#26013=CARTESIAN_POINT('Ctrl Pts',(4.57549970660796,-4.98568866204364,68.0391726256903));
#26014=CARTESIAN_POINT('Ctrl Pts',(4.71254069815131,-4.8599224822632,68.0479219691366));
#26015=CARTESIAN_POINT('Ctrl Pts',(4.84439326931152,-4.72850295734168,68.0566713125829));
#26016=CARTESIAN_POINT('Ctrl Pts',(4.97060959434539,-4.59187644221853,68.0654206560292));
#26017=CARTESIAN_POINT('Ctrl Pts',(5.0968249628037,-4.4552509625683,68.0741699331655));
#26018=CARTESIAN_POINT('Ctrl Pts',(5.21740397615707,-4.31341878218486,68.0829192103018));
#26019=CARTESIAN_POINT('Ctrl Pts',(5.33193710451814,-4.1668616143883,68.0916684874381));
#26020=CARTESIAN_POINT('Ctrl Pts',(5.44646940289264,-4.02030550864675,68.1004177011711));
#26021=CARTESIAN_POINT('Ctrl Pts',(5.55495572749547,-3.86902470980302,68.1091669149041));
#26022=CARTESIAN_POINT('Ctrl Pts',(5.6570276249134,-3.71353301465958,68.117916128637));
#26023=CARTESIAN_POINT('Ctrl Pts',(5.75909881655048,-3.55804239467065,68.1266652818732));
#26024=CARTESIAN_POINT('Ctrl Pts',(5.85475551250685,-3.3983411761972,68.1354144351093));
#26025=CARTESIAN_POINT('Ctrl Pts',(5.94367283728007,-3.23497174692131,68.1441635883454));
#26026=CARTESIAN_POINT('Ctrl Pts',(6.0325895767623,-3.07160339301126,68.1529126839909));
#26027=CARTESIAN_POINT('Ctrl Pts',(6.11476689685209,-2.90456712829663,68.1616617796365));
#26028=CARTESIAN_POINT('Ctrl Pts',(6.18992570525191,-2.73443024476062,68.170410875282));
#26029=CARTESIAN_POINT('Ctrl Pts',(6.26508404388637,-2.56429442463177,68.179159916243));
#26030=CARTESIAN_POINT('Ctrl Pts',(6.33322384283264,-2.3910582865613,68.1879089572041));
#26031=CARTESIAN_POINT('Ctrl Pts',(6.39411368719989,-2.21531017132207,68.1966579981651));
#26032=CARTESIAN_POINT('Ctrl Pts',(6.45500317120842,-2.03956309619664,68.2054069873475));
#26033=CARTESIAN_POINT('Ctrl Pts',(6.50864269270023,-1.86130434438805,68.2141559765299));
#26034=CARTESIAN_POINT('Ctrl Pts',(6.55485008446283,-1.6811393072014,68.2229049657123));
#26035=CARTESIAN_POINT('Ctrl Pts',(6.60199664749361,-1.49731239212032,68.2318317792416));
#26036=CARTESIAN_POINT('Ctrl Pts',(6.6414056364087,-1.31150116499859,68.240758592771));
#26037=CARTESIAN_POINT('Ctrl Pts',(6.67293772282141,-1.12436255155843,68.2496854063004));
#26038=CARTESIAN_POINT('Ctrl Pts',(6.70384494949845,-0.940932395053181,
68.2584353204559));
#26039=CARTESIAN_POINT('Ctrl Pts',(6.7271844934891,-0.756227260508557,68.2671852346114));
#26040=CARTESIAN_POINT('Ctrl Pts',(6.74287707373917,-0.570874564543536,
68.275935148767));
#26041=CARTESIAN_POINT('Ctrl Pts',(6.7585693453866,-0.385525513634341,68.284684890851));
#26042=CARTESIAN_POINT('Ctrl Pts',(6.76661493004097,-0.199529212420114,
68.2934346329349));
#26043=CARTESIAN_POINT('Ctrl Pts',(6.76698649908906,-0.0135174386023304,
68.3021843750189));
#26044=CARTESIAN_POINT('Ctrl Pts',(6.76735806132394,0.172490924443888,68.3109339566648));
#26045=CARTESIAN_POINT('Ctrl Pts',(6.76005588896299,0.358514472899531,68.3196835383107));
#26046=CARTESIAN_POINT('Ctrl Pts',(6.74510478454599,0.543921359660353,68.3284331199566));
#26047=CARTESIAN_POINT('Ctrl Pts',(6.73015393440708,0.729325093148581,68.3371825527956));
#26048=CARTESIAN_POINT('Ctrl Pts',(6.70755443556923,0.914111900254487,68.3459319856347));
#26049=CARTESIAN_POINT('Ctrl Pts',(6.67738304682349,1.09765415591352,68.3546814184737));
#26050=CARTESIAN_POINT('Ctrl Pts',(6.64721213111896,1.28119353391089,68.3634307141351));
#26051=CARTESIAN_POINT('Ctrl Pts',(6.60946960955534,1.46348811672471,68.3721800097964));
#26052=CARTESIAN_POINT('Ctrl Pts',(6.56428366991228,1.64391876348043,68.3809293054577));
#26053=CARTESIAN_POINT('Ctrl Pts',(6.51909837867768,1.82434682109535,68.3896784755685));
#26054=CARTESIAN_POINT('Ctrl Pts',(6.46646995271977,2.00291071820264,68.3984276456794));
#26055=CARTESIAN_POINT('Ctrl Pts',(6.40657713281611,2.17900400212521,68.4071768157902));
#26056=CARTESIAN_POINT('Ctrl Pts',(6.34668509279127,2.35509499309477,68.415925871976));
#26057=CARTESIAN_POINT('Ctrl Pts',(6.27952894037599,2.52871516397942,68.4246749281617));
#26058=CARTESIAN_POINT('Ctrl Pts',(6.20533675061525,2.69927486771241,68.4334239843475));
#26059=CARTESIAN_POINT('Ctrl Pts',(6.12832117907997,2.87632521635753,68.4425059856298));
#26060=CARTESIAN_POINT('Ctrl Pts',(6.04372366626161,3.05007728919837,68.451587986912));
#26061=CARTESIAN_POINT('Ctrl Pts',(5.9518537800795,3.21989527478044,68.4606699881943));
#26062=CARTESIAN_POINT('Ctrl Pts',(5.86334450817457,3.38350129286604,68.4694197685015));
#26063=CARTESIAN_POINT('Ctrl Pts',(5.76808562057344,3.54345567124818,68.4781695488086));
#26064=CARTESIAN_POINT('Ctrl Pts',(5.66640068804575,3.69921508465169,68.4869193291157));
#26065=CARTESIAN_POINT('Ctrl Pts',(5.56471941108019,3.85496889852145,68.4956687948692));
#26066=CARTESIAN_POINT('Ctrl Pts',(5.45661270815213,4.00652780919501,68.5044182606227));
#26067=CARTESIAN_POINT('Ctrl Pts',(5.34244776449218,4.15337704569096,68.5131677263761));
#26068=CARTESIAN_POINT('Ctrl Pts',(5.22828631819699,4.30022178356123,68.5219169240957));
#26069=CARTESIAN_POINT('Ctrl Pts',(5.10806717844173,4.44235690972559,68.5306661218153));
#26070=CARTESIAN_POINT('Ctrl Pts',(4.98219864544823,4.57929969070532,68.5394153195349));
#26071=CARTESIAN_POINT('Ctrl Pts',(4.85633329944151,4.7162390042987,68.5481642957252));
#26072=CARTESIAN_POINT('Ctrl Pts',(4.72481904033797,4.8479860248347,68.5569132719154));
#26073=CARTESIAN_POINT('Ctrl Pts',(4.58810250737372,4.97409332258965,68.5656622481056));
#26074=CARTESIAN_POINT('Ctrl Pts',(4.4513770868582,5.1002088182198,68.5744117930418));
#26075=CARTESIAN_POINT('Ctrl Pts',(4.30944892636232,5.22068366307784,68.583161337978));
#26076=CARTESIAN_POINT('Ctrl Pts',(4.16280009466845,5.33510865604707,68.5919108829141));
#26077=CARTESIAN_POINT('Ctrl Pts',(4.01615988348994,5.44952692272739,68.6006599135224));
#26078=CARTESIAN_POINT('Ctrl Pts',(3.86479978232458,5.55789587288468,68.6094089441307));
#26079=CARTESIAN_POINT('Ctrl Pts',(3.70923383581317,5.65984746713714,68.6181579747389));
#26080=CARTESIAN_POINT('Ctrl Pts',(3.55366577799792,5.76180044505228,68.626907124087));
#26081=CARTESIAN_POINT('Ctrl Pts',(3.39389200027093,5.85733573570912,68.635656273435));
#26082=CARTESIAN_POINT('Ctrl Pts',(3.23045513626296,5.9461288762179,68.644405422783));
#26083=CARTESIAN_POINT('Ctrl Pts',(3.18695122151749,5.96976399206598,68.646734286896));
#26084=CARTESIAN_POINT('Ctrl Pts',(3.1431879126275,5.99292165435288,68.6490631510091));
#26085=CARTESIAN_POINT('Ctrl Pts',(3.09917575053259,6.01559628526639,68.6513920151221));
#26086=CARTESIAN_POINT('Origin',(0.,0.,-3.69717978381041));
#26087=CARTESIAN_POINT('',(3.09917575053257,6.0155962852664,71.0459800471047));
#26088=CARTESIAN_POINT('',(3.09917575053263,6.01559628526637,70.6515467266273));
#26089=CARTESIAN_POINT('',(3.09917575053259,6.01559628526639,-3.69717978381041));
#26090=CARTESIAN_POINT('',(-6.767,3.55173084953114E-12,69.6971797838099));
#26091=CARTESIAN_POINT('Ctrl Pts',(-6.76699999999339,9.45791233018501E-6,
69.6973826905095));
#26092=CARTESIAN_POINT('Ctrl Pts',(-6.76700023814962,-0.170387891941315,
69.7054353713839));
#26093=CARTESIAN_POINT('Ctrl Pts',(-6.76056010934896,-0.341058540649849,
69.7134880522583));
#26094=CARTESIAN_POINT('Ctrl Pts',(-6.7476435435305,-0.511464181982631,
69.7215407331328));
#26095=CARTESIAN_POINT('Ctrl Pts',(-6.7347406520964,-0.681689419927384,
69.7295848888733));
#26096=CARTESIAN_POINT('Ctrl Pts',(-6.71537499519369,-0.851649838935862,
69.7376290446138));
#26097=CARTESIAN_POINT('Ctrl Pts',(-6.68956246968668,-1.02080505688376,
69.7456732003543));
#26098=CARTESIAN_POINT('Ctrl Pts',(-6.66377158270051,-1.18981847279425,
69.7537106127162));
#26099=CARTESIAN_POINT('Ctrl Pts',(-6.63154463910887,-1.3580276630686,69.7617480250781));
#26100=CARTESIAN_POINT('Ctrl Pts',(-6.59294948837972,-1.52489542056944,
69.76978543744));
#26101=CARTESIAN_POINT('Ctrl Pts',(-6.55437819706301,-1.69166002089703,
69.7778178810965));
#26102=CARTESIAN_POINT('Ctrl Pts',(-6.50944661927347,-1.8570844755594,69.785850324753));
#26103=CARTESIAN_POINT('Ctrl Pts',(-6.45827400213015,-2.02063997619809,
69.7938827684094));
#26104=CARTESIAN_POINT('Ctrl Pts',(-6.40703937467019,-2.18439367128042,
69.8019249456774));
#26105=CARTESIAN_POINT('Ctrl Pts',(-6.34954865059723,-2.34627351135502,
69.8099671229453));
#26106=CARTESIAN_POINT('Ctrl Pts',(-6.28597224545374,-2.50576174633288,
69.8180093002133));
#26107=CARTESIAN_POINT('Ctrl Pts',(-6.22249789812155,-2.66499395833884,
69.8260385675501));
#26108=CARTESIAN_POINT('Ctrl Pts',(-6.15295753512077,-2.82184188993491,
69.834067834887));
#26109=CARTESIAN_POINT('Ctrl Pts',(-6.07756960555274,-2.97580857745615,
69.8420971022238));
#26110=CARTESIAN_POINT('Ctrl Pts',(-6.00217581822731,-3.12978722842443,
69.850126993447));
#26111=CARTESIAN_POINT('Ctrl Pts',(-5.92093372446528,-3.28088385300036,
69.8581568846703));
#26112=CARTESIAN_POINT('Ctrl Pts',(-5.83410840710039,-3.42862481094105,
69.8661867758935));
#26113=CARTESIAN_POINT('Ctrl Pts',(-5.74725905045123,-3.57640667385042,
69.8742188903488));
#26114=CARTESIAN_POINT('Ctrl Pts',(-5.65482358347639,-3.72083069817106,
69.8822510048042));
#26115=CARTESIAN_POINT('Ctrl Pts',(-5.55711110814656,-3.86145116914796,
69.8902831192596));
#26116=CARTESIAN_POINT('Ctrl Pts',(-5.45916898367373,-4.00240213395934,
69.8983341112246));
#26117=CARTESIAN_POINT('Ctrl Pts',(-5.35592524515943,-4.13953134509173,
69.9063851031897));
#26118=CARTESIAN_POINT('Ctrl Pts',(-5.24773194102639,-4.27242302155713,
69.9144360951548));
#26119=CARTESIAN_POINT('Ctrl Pts',(-5.13961422382154,-4.40522185610699,
69.9224814624672));
#26120=CARTESIAN_POINT('Ctrl Pts',(-5.02655413405461,-4.53378882241542,
69.9305268297797));
#26121=CARTESIAN_POINT('Ctrl Pts',(-4.90893979515681,-4.657746138158,69.9385721970921));
#26122=CARTESIAN_POINT('Ctrl Pts',(-4.79113743472779,-4.78190161548982,
69.946630425951));
#26123=CARTESIAN_POINT('Ctrl Pts',(-4.66876654729672,-4.90143245847534,
69.9546886548099));
#26124=CARTESIAN_POINT('Ctrl Pts',(-4.54224976776608,-5.01600000470784,
69.9627468836688));
#26125=CARTESIAN_POINT('Ctrl Pts',(-4.41587192249547,-5.13044173871749,
69.9707962633926));
#26126=CARTESIAN_POINT('Ctrl Pts',(-4.28535761607779,-5.23993089425125,
69.9788456431165));
#26127=CARTESIAN_POINT('Ctrl Pts',(-4.15115592680216,-5.34417378753492,
69.9868950228404));
#26128=CARTESIAN_POINT('Ctrl Pts',(-4.01391333858133,-5.45077873830045,
69.995126794831));
#26129=CARTESIAN_POINT('Ctrl Pts',(-3.87236008956517,-5.55225004774207,
70.0033585668217));
#26130=CARTESIAN_POINT('Ctrl Pts',(-3.72691577815881,-5.64821987731629,
70.0115903388123));
#26131=CARTESIAN_POINT('Ctrl Pts',(-3.58164514179658,-5.74407510932239,
70.0198122812445));
#26132=CARTESIAN_POINT('Ctrl Pts',(-3.43249299106102,-5.83444174709155,
70.0280342236766));
#26133=CARTESIAN_POINT('Ctrl Pts',(-3.27991217517725,-5.91899190091726,
70.0362561661088));
#26134=CARTESIAN_POINT('Ctrl Pts',(-3.12748298512894,-6.00345803377585,
70.0444699380585));
#26135=CARTESIAN_POINT('Ctrl Pts',(-2.97163222661652,-6.08211902122219,
70.0526837100081));
#26136=CARTESIAN_POINT('Ctrl Pts',(-2.81284200812162,-6.15468998710303,
70.0608974819577));
#26137=CARTESIAN_POINT('Ctrl Pts',(-2.65417778254027,-6.22720337117867,
70.0691047366479));
#26138=CARTESIAN_POINT('Ctrl Pts',(-2.49257906689244,-6.29363621003319,
70.077311991338));
#26139=CARTESIAN_POINT('Ctrl Pts',(-2.32855295424396,-6.35374929779904,
70.0855192460282));
#26140=CARTESIAN_POINT('Ctrl Pts',(-2.1646241453794,-6.41382672520076,70.093721632));
#26141=CARTESIAN_POINT('Ctrl Pts',(-1.99827114366252,-6.46759174702125,
70.1019240179719));
#26142=CARTESIAN_POINT('Ctrl Pts',(-1.83002151089933,-6.51485305050281,
70.1101264039437));
#26143=CARTESIAN_POINT('Ctrl Pts',(-1.66182209656591,-6.56210024763292,
70.1183263417025));
#26144=CARTESIAN_POINT('Ctrl Pts',(-1.49172752230965,-6.60284749270681,
70.1265262794613));
#26145=CARTESIAN_POINT('Ctrl Pts',(-1.32028126071456,-6.63695309555567,
70.1347262172201));
#26146=CARTESIAN_POINT('Ctrl Pts',(-1.14885897172868,-6.67105392956162,
70.1429250084162));
#26147=CARTESIAN_POINT('Ctrl Pts',(-0.97608572307747,-6.69851490021167,
70.1511237996122));
#26148=CARTESIAN_POINT('Ctrl Pts',(-0.802515971789543,-6.71924527867697,
70.1593225908082));
#26149=CARTESIAN_POINT('Ctrl Pts',(-0.628939003574673,-6.73997651909905,
70.1675217229051));
#26150=CARTESIAN_POINT('Ctrl Pts',(-0.45456582265216,-6.75397656721264,
70.175720855002));
#26151=CARTESIAN_POINT('Ctrl Pts',(-0.279956871417882,-6.76120648628231,
70.1839199870989));
#26152=CARTESIAN_POINT('Ctrl Pts',(-0.105308985192508,-6.76843801750778,
70.1921209474705));
#26153=CARTESIAN_POINT('Ctrl Pts',(0.0695744180061118,-6.76889639811614,
70.2003219078421));
#26154=CARTESIAN_POINT('Ctrl Pts',(0.244131967469593,-6.76259481134715,
70.2085228682137));
#26155=CARTESIAN_POINT('Ctrl Pts',(0.418853119391245,-6.75628731847391,
70.21673151486));
#26156=CARTESIAN_POINT('Ctrl Pts',(0.593247448734452,-6.74320721279566,
70.2249401615063));
#26157=CARTESIAN_POINT('Ctrl Pts',(0.766756831578491,-6.72341973710014,
70.2331488081527));
#26158=CARTESIAN_POINT('Ctrl Pts',(0.940349052680784,-6.70362281430732,
70.2413613738377));
#26159=CARTESIAN_POINT('Ctrl Pts',(1.11305513080198,-6.67711219103453,70.2495739395228));
#26160=CARTESIAN_POINT('Ctrl Pts',(1.28432629738894,-6.64400443722272,70.2577865052078));
#26161=CARTESIAN_POINT('Ctrl Pts',(1.45583247274901,-6.61085125479174,70.2660103397189));
#26162=CARTESIAN_POINT('Ctrl Pts',(1.62589945247983,-6.57108293215374,70.27423417423));
#26163=CARTESIAN_POINT('Ctrl Pts',(1.79399161177041,-6.52486651946976,70.2824580087412));
#26164=CARTESIAN_POINT('Ctrl Pts',(1.94843669693945,-6.48240232706894,70.2900141661898));
#26165=CARTESIAN_POINT('Ctrl Pts',(2.10121458872838,-6.43449519935904,70.2975703236385));
#26166=CARTESIAN_POINT('Ctrl Pts',(2.25192491332738,-6.38131045982998,70.3051264810871));
#26167=CARTESIAN_POINT('Ctrl Pts',(2.42436692962267,-6.32045674098269,70.3137721994834));
#26168=CARTESIAN_POINT('Ctrl Pts',(2.59449505643908,-6.2525546804886,70.3224179178797));
#26169=CARTESIAN_POINT('Ctrl Pts',(2.7617273009984,-6.17779502046807,70.3310636362759));
#26170=CARTESIAN_POINT('Ctrl Pts',(2.92874485337425,-6.10313133664333,70.3396982553285));
#26171=CARTESIAN_POINT('Ctrl Pts',(3.09287365973293,-6.02162773232303,70.348332874381));
#26172=CARTESIAN_POINT('Ctrl Pts',(3.25354948255545,-5.93352380669052,70.3569674934336));
#26173=CARTESIAN_POINT('Ctrl Pts',(3.41989974152747,-5.84230839800014,70.365907053165));
#26174=CARTESIAN_POINT('Ctrl Pts',(3.58254836182367,-5.74401804445167,70.3748466128964));
#26175=CARTESIAN_POINT('Ctrl Pts',(3.74089174189155,-5.63897313129329,70.3837861726279));
#26176=CARTESIAN_POINT('Ctrl Pts',(3.89340931949669,-5.53779305235478,70.3923968262245));
#26177=CARTESIAN_POINT('Ctrl Pts',(4.04193248917253,-5.43034673214416,70.4010074798212));
#26178=CARTESIAN_POINT('Ctrl Pts',(4.18594637031747,-5.31696736728993,70.4096181334179));
#26179=CARTESIAN_POINT('Ctrl Pts',(4.3298239325841,-5.2036953236725,70.4182206364486));
#26180=CARTESIAN_POINT('Ctrl Pts',(4.46920047740784,-5.08450162030227,70.4268231394793));
#26181=CARTESIAN_POINT('Ctrl Pts',(4.60359068792702,-4.95976227031414,70.43542564251));
#26182=CARTESIAN_POINT('Ctrl Pts',(4.7378296448132,-4.83516331209852,70.4440184635867));
#26183=CARTESIAN_POINT('Ctrl Pts',(4.86709324015349,-4.70503136595633,70.4526112846635));
#26184=CARTESIAN_POINT('Ctrl Pts',(4.99092964177323,-4.56978230453808,70.4612041057402));
#26185=CARTESIAN_POINT('Ctrl Pts',(5.00552430251826,-4.55384261199481,70.4622168072304));
#26186=CARTESIAN_POINT('Ctrl Pts',(5.02004362027724,-4.53783188958982,70.4632295087205));
#26187=CARTESIAN_POINT('Ctrl Pts',(5.03448688702477,-4.52175085385912,70.4642422102107));
#26188=CARTESIAN_POINT('Ctrl Pts',(5.15707344790452,-4.38526380421377,70.4728374674366));
#26189=CARTESIAN_POINT('Ctrl Pts',(5.27403422616259,-4.24386923268498,70.4814327246625));
#26190=CARTESIAN_POINT('Ctrl Pts',(5.38499870673418,-4.09805782395408,70.4900279818884));
#26191=CARTESIAN_POINT('Ctrl Pts',(5.49606710069976,-3.95210986920155,70.4986312881977));
#26192=CARTESIAN_POINT('Ctrl Pts',(5.60112780376439,-3.80173706426982,70.5072345945069));
#26193=CARTESIAN_POINT('Ctrl Pts',(5.69985346619164,-3.64745931628348,70.5158379008161));
#26194=CARTESIAN_POINT('Ctrl Pts',(5.80267233843029,-3.48678514434604,70.5247979040259));
#26195=CARTESIAN_POINT('Ctrl Pts',(5.89861947511329,-3.32187565648612,70.5337579072358));
#26196=CARTESIAN_POINT('Ctrl Pts',(5.98737850424075,-3.15334546901474,70.5427179104456));
#26197=CARTESIAN_POINT('Ctrl Pts',(6.07283719878345,-2.99108175394348,70.5513447530883));
#26198=CARTESIAN_POINT('Ctrl Pts',(6.15163261348022,-2.82546202870845,70.5599715957312));
#26199=CARTESIAN_POINT('Ctrl Pts',(6.22353184835703,-2.65705482301094,70.5685984383739));
#26200=CARTESIAN_POINT('Ctrl Pts',(6.29549980069985,-2.48848666265999,70.5772335260943));
#26201=CARTESIAN_POINT('Ctrl Pts',(6.36055830594989,-2.31712598789673,70.5858686138146));
#26202=CARTESIAN_POINT('Ctrl Pts',(6.4185237904181,-2.14355810554249,70.5945037015349));
#26203=CARTESIAN_POINT('Ctrl Pts',(6.47657536526006,-1.9697324400609,70.6031516140929));
#26204=CARTESIAN_POINT('Ctrl Pts',(6.5275127786828,-1.79369330782663,70.6117995266509));
#26205=CARTESIAN_POINT('Ctrl Pts',(6.57120277754873,-1.61603931150697,70.6204474392089));
#26206=CARTESIAN_POINT('Ctrl Pts',(6.57610414329484,-1.59610918482298,70.6214176059172));
#26207=CARTESIAN_POINT('Ctrl Pts',(6.58091435011396,-1.5761587425345,70.6223877726256));
#26208=CARTESIAN_POINT('Ctrl Pts',(6.58563325034586,-1.55618883556562,70.6233579393339));
#26209=CARTESIAN_POINT('Ctrl Pts',(6.62563817172745,-1.38689206745695,70.6315826190234));
#26210=CARTESIAN_POINT('Ctrl Pts',(6.65916345610177,-1.21582859578257,70.6398072987129));
#26211=CARTESIAN_POINT('Ctrl Pts',(6.68605437655763,-1.04353527669869,70.6480319784024));
#26212=CARTESIAN_POINT('Ctrl Pts',(6.71291703161691,-0.871423057365544,
70.6562480130241));
#26213=CARTESIAN_POINT('Ctrl Pts',(6.73315915458184,-0.698083916077889,
70.6644640476457));
#26214=CARTESIAN_POINT('Ctrl Pts',(6.74667636948375,-0.524067710748956,
70.6726800822673));
#26215=CARTESIAN_POINT('Ctrl Pts',(6.76018208378677,-0.350199560370123,
70.680889126594));
#26216=CARTESIAN_POINT('Ctrl Pts',(6.76697425772295,-0.175655848560904,
70.6890981709207));
#26217=CARTESIAN_POINT('Ctrl Pts',(6.76699992692022,-0.00099451580590046,
70.6973072152474));
#26218=CARTESIAN_POINT('Ctrl Pts',(6.76702557941799,0.173553188203546,70.705510919048));
#26219=CARTESIAN_POINT('Ctrl Pts',(6.76029349563374,0.348218003599608,70.7137146228486));
#26220=CARTESIAN_POINT('Ctrl Pts',(6.7468026937055,0.522438907632548,70.7219183266492));
#26221=CARTESIAN_POINT('Ctrl Pts',(6.73331796751756,0.696581349245336,70.7301183358159));
#26222=CARTESIAN_POINT('Ctrl Pts',(6.71308061502162,0.870279921184807,70.7383183449826));
#26223=CARTESIAN_POINT('Ctrl Pts',(6.68614171254121,1.04297555091983,70.7465183541493));
#26224=CARTESIAN_POINT('Ctrl Pts',(6.65920496415265,1.21565737154555,70.7547177076259));
#26225=CARTESIAN_POINT('Ctrl Pts',(6.62556777971534,1.3873360544997,70.7629170611024));
#26226=CARTESIAN_POINT('Ctrl Pts',(6.58533293037598,1.5574592116989,70.771116414579));
#26227=CARTESIAN_POINT('Ctrl Pts',(6.54509834335656,1.7275812597428,70.779315714598));
#26228=CARTESIAN_POINT('Ctrl Pts',(6.49826625857153,1.89614745309137,70.7875150146171));
#26229=CARTESIAN_POINT('Ctrl Pts',(6.44499022875867,2.06261725756509,70.7957143146362));
#26230=CARTESIAN_POINT('Ctrl Pts',(6.39170488149717,2.22911617595471,70.8039150486314));
#26231=CARTESIAN_POINT('Ctrl Pts',(6.33197345316412,2.39351763354346,70.8121157826267));
#26232=CARTESIAN_POINT('Ctrl Pts',(6.26599888527343,2.55529782408082,70.8203165166219));
#26233=CARTESIAN_POINT('Ctrl Pts',(6.20000081052336,2.71713565719636,70.8285201725537));
#26234=CARTESIAN_POINT('Ctrl Pts',(6.12775530030852,2.87635003099543,70.8367238284854));
#26235=CARTESIAN_POINT('Ctrl Pts',(6.04951281281268,3.03243857771517,70.8449274844172));
#26236=CARTESIAN_POINT('Ctrl Pts',(5.97118069353488,3.18870593386484,70.8531405381624));
#26237=CARTESIAN_POINT('Ctrl Pts',(5.8868380327729,3.34183998814974,70.8613535919076));
#26238=CARTESIAN_POINT('Ctrl Pts',(5.79678102521562,3.49136345081691,70.8695666456529));
#26239=CARTESIAN_POINT('Ctrl Pts',(5.70667072891441,3.64097538985842,70.8777845592455));
#26240=CARTESIAN_POINT('Ctrl Pts',(5.61083954201652,3.7869721792818,70.8860024728382));
#26241=CARTESIAN_POINT('Ctrl Pts',(5.5096260433671,3.92890695515317,70.8942203864308));
#26242=CARTESIAN_POINT('Ctrl Pts',(5.40825468583711,4.071063101347,70.9024511171937));
#26243=CARTESIAN_POINT('Ctrl Pts',(5.30148445975244,4.2091442897715,70.9106818479565));
#26244=CARTESIAN_POINT('Ctrl Pts',(5.18969401191639,4.34273704737913,70.9189125787194));
#26245=CARTESIAN_POINT('Ctrl Pts',(5.08702788545851,4.46542598200542,70.9264715183399));
#26246=CARTESIAN_POINT('Ctrl Pts',(4.98012818282313,4.58432953735254,70.9340304579604));
#26247=CARTESIAN_POINT('Ctrl Pts',(4.86931389109609,4.69915643812574,70.9415893975809));
#26248=CARTESIAN_POINT('Ctrl Pts',(4.74974381084406,4.82305617638663,70.9497455929863));
#26249=CARTESIAN_POINT('Ctrl Pts',(4.62524577628951,4.94259225461675,70.9579017883918));
#26250=CARTESIAN_POINT('Ctrl Pts',(4.49617258679411,5.05734328177959,70.9660579837973));
#26251=CARTESIAN_POINT('Ctrl Pts',(4.36729915372743,5.17191671779847,70.9742015565003));
#26252=CARTESIAN_POINT('Ctrl Pts',(4.23386494243849,5.28171961546955,70.9823451292033));
#26253=CARTESIAN_POINT('Ctrl Pts',(4.09626143376372,5.38636531125211,70.9904887019063));
#26254=CARTESIAN_POINT('Ctrl Pts',(3.9587811050275,5.49091733027817,70.9986249846441));
#26255=CARTESIAN_POINT('Ctrl Pts',(3.81713919384544,5.59032111347143,71.0067612673819));
#26256=CARTESIAN_POINT('Ctrl Pts',(3.67176281342898,5.68422790200394,71.0148975501198));
#26257=CARTESIAN_POINT('Ctrl Pts',(3.52651322166004,5.77805279061105,71.0230267368749));
#26258=CARTESIAN_POINT('Ctrl Pts',(3.37753595374531,5.86639003610613,71.03115592363));
#26259=CARTESIAN_POINT('Ctrl Pts',(3.2252896247094,5.94893232746364,71.0392851103851));
#26260=CARTESIAN_POINT('Ctrl Pts',(3.18349456494932,5.97159205280392,71.0415167559583));
#26261=CARTESIAN_POINT('Ctrl Pts',(3.14145331564828,5.99381530157255,71.0437484015315));
#26262=CARTESIAN_POINT('Ctrl Pts',(3.09917575053257,6.0155962852664,71.0459800471047));
#26263=CARTESIAN_POINT('Ctrl Pts',(3.09917575053258,6.0155962852664,69.0457515827422));
#26264=CARTESIAN_POINT('Ctrl Pts',(2.93382384459269,6.10078395293757,69.0545010306546));
#26265=CARTESIAN_POINT('Ctrl Pts',(2.76495772122994,6.17915010267045,69.063250478567));
#26266=CARTESIAN_POINT('Ctrl Pts',(2.59315093316727,6.25042856433171,69.0719999264794));
#26267=CARTESIAN_POINT('Ctrl Pts',(2.42134553245631,6.32170645041446,69.0807493037394));
#26268=CARTESIAN_POINT('Ctrl Pts',(2.24659977927603,6.38589665313453,69.0894986809994));
#26269=CARTESIAN_POINT('Ctrl Pts',(2.0695071868993,6.44278115439072,69.0982480582594));
#26270=CARTESIAN_POINT('Ctrl Pts',(1.89241596572864,6.49966521519723,69.1069973677741));
#26271=CARTESIAN_POINT('Ctrl Pts',(1.71297821457193,6.54924360009547,69.1157466772887));
#26272=CARTESIAN_POINT('Ctrl Pts',(1.53180337335832,6.59134792173559,69.1244959868034));
#26273=CARTESIAN_POINT('Ctrl Pts',(1.35062987477775,6.63345193135306,69.1332452314795));
#26274=CARTESIAN_POINT('Ctrl Pts',(1.16771959102949,6.66808192368238,69.1419944761556));
#26275=CARTESIAN_POINT('Ctrl Pts',(0.98369374690687,6.69512028363168,69.1507437208317));
#26276=CARTESIAN_POINT('Ctrl Pts',(0.799669205420005,6.72215845218865,69.1594929035759));
#26277=CARTESIAN_POINT('Ctrl Pts',(0.614529402873718,6.74160505424577,69.1682420863201));
#26278=CARTESIAN_POINT('Ctrl Pts',(0.4289031273636,6.7533940435412,69.1769912690643));
#26279=CARTESIAN_POINT('Ctrl Pts',(0.243278104164236,6.76518295330329,69.1857403927829));
#26280=CARTESIAN_POINT('Ctrl Pts',(0.0571669005394799,6.76931433552275,
69.1944895165015));
#26281=CARTESIAN_POINT('Ctrl Pts',(-0.128798404777146,6.76577415902474,
69.2032386402201));
#26282=CARTESIAN_POINT('Ctrl Pts',(-0.314762517258584,6.76223400523443,
69.2119877078193));
#26283=CARTESIAN_POINT('Ctrl Pts',(-0.500580446818851,6.75102239665093,
69.2207367754185));
#26284=CARTESIAN_POINT('Ctrl Pts',(-0.685621118841808,6.73217741012506,
69.2294858430177));
#26285=CARTESIAN_POINT('Ctrl Pts',(-0.870660665413722,6.71333253821782,
69.2382348574035));
#26286=CARTESIAN_POINT('Ctrl Pts',(-1.05492267885413,6.68685441030624,69.2469838717893));
#26287=CARTESIAN_POINT('Ctrl Pts',(-1.23778137635183,6.6528329502819,69.255732886175));
#26288=CARTESIAN_POINT('Ctrl Pts',(-1.42999922978777,6.6170701886188,69.2649296965424));
#26289=CARTESIAN_POINT('Ctrl Pts',(-1.62066601233625,6.5729717293443,69.2741265069098));
#26290=CARTESIAN_POINT('Ctrl Pts',(-1.80906628500315,6.52070304311314,69.2833233172772));
#26291=CARTESIAN_POINT('Ctrl Pts',(-1.98831342545459,6.47097374915052,69.292073315015));
#26292=CARTESIAN_POINT('Ctrl Pts',(-2.16550875896636,6.41384933989551,69.3008233127528));
#26293=CARTESIAN_POINT('Ctrl Pts',(-2.34005036713947,6.34952386240499,69.3095733104905));
#26294=CARTESIAN_POINT('Ctrl Pts',(-2.51458843547026,6.28519968948621,69.3183231307714));
#26295=CARTESIAN_POINT('Ctrl Pts',(-2.68647261717993,6.21367483971126,69.3270729510522));
#26296=CARTESIAN_POINT('Ctrl Pts',(-2.8551190590867,6.13519226743872,69.3358227713331));
#26297=CARTESIAN_POINT('Ctrl Pts',(-3.02376230488813,6.05671118252972,69.3445724257916));
#26298=CARTESIAN_POINT('Ctrl Pts',(-3.18916767379823,5.97127275992676,69.3533220802502));
#26299=CARTESIAN_POINT('Ctrl Pts',(-3.35077334102697,5.87916720438048,69.3620717347087));
#26300=CARTESIAN_POINT('Ctrl Pts',(-3.51237616037272,5.78706327195701,69.3708212349771));
#26301=CARTESIAN_POINT('Ctrl Pts',(-3.67017916302199,5.68829258362363,69.3795707352456));
#26302=CARTESIAN_POINT('Ctrl Pts',(-3.82364636566356,5.58319061741115,69.388320235514));
#26303=CARTESIAN_POINT('Ctrl Pts',(-3.97711106778701,5.47809036367773,69.3970695932224));
#26304=CARTESIAN_POINT('Ctrl Pts',(-4.12623987481839,5.36665920043293,69.4058189509309));
#26305=CARTESIAN_POINT('Ctrl Pts',(-4.27052628213849,5.249275595124,69.4145683086393));
#26306=CARTESIAN_POINT('Ctrl Pts',(-4.41481053024907,5.13189374643098,69.4233175354158));
#26307=CARTESIAN_POINT('Ctrl Pts',(-4.55425230136467,5.0085598147741,69.4320667621924));
#26308=CARTESIAN_POINT('Ctrl Pts',(-4.68837800630493,4.87969268192129,69.4408159889689));
#26309=CARTESIAN_POINT('Ctrl Pts',(-4.82250188228843,4.75082730631862,69.4495650964397));
#26310=CARTESIAN_POINT('Ctrl Pts',(-4.95130963052918,4.61642907903577,69.4583142039106));
#26311=CARTESIAN_POINT('Ctrl Pts',(-5.07436379033323,4.4769544473174,69.4670633113814));
#26312=CARTESIAN_POINT('Ctrl Pts',(-5.19741643562771,4.33748153220628,69.4758123111712));
#26313=CARTESIAN_POINT('Ctrl Pts',(-5.31471544462747,4.19293255254623,69.4845613109609));
#26314=CARTESIAN_POINT('Ctrl Pts',(-5.42586245275609,4.04379841779628,69.4933103107507));
#26315=CARTESIAN_POINT('Ctrl Pts',(-5.53702160019133,3.89464799484371,69.5020602660928));
#26316=CARTESIAN_POINT('Ctrl Pts',(-5.64202723081231,3.74091164443881,69.510810221435));
#26317=CARTESIAN_POINT('Ctrl Pts',(-5.74052265232945,3.58311159163267,69.5195601767771));
#26318=CARTESIAN_POINT('Ctrl Pts',(-5.83901427066901,3.42531763191813,69.5283097942596));
#26319=CARTESIAN_POINT('Ctrl Pts',(-5.93099603115726,3.26346052695637,69.537059411742));
#26320=CARTESIAN_POINT('Ctrl Pts',(-6.01615550622744,3.09809004467095,69.5458090292245));
#26321=CARTESIAN_POINT('Ctrl Pts',(-6.10131214578792,2.93272506863843,69.5545583553756));
#26322=CARTESIAN_POINT('Ctrl Pts',(-6.17964682328743,2.76384720416905,69.5633076815267));
#26323=CARTESIAN_POINT('Ctrl Pts',(-6.25089348288561,2.59203002791599,69.5720570076778));
#26324=CARTESIAN_POINT('Ctrl Pts',(-6.32213814889331,2.42021765937028,69.5808060890094));
#26325=CARTESIAN_POINT('Ctrl Pts',(-6.38629508412588,2.2454664083191,69.5895551703409));
#26326=CARTESIAN_POINT('Ctrl Pts',(-6.44314639819816,2.06836976660027,69.5983042516725));
#26327=CARTESIAN_POINT('Ctrl Pts',(-6.50000285283706,1.89125711158257,69.6070541241069));
#26328=CARTESIAN_POINT('Ctrl Pts',(-6.54955227673255,1.71179891440232,69.6158039965413));
#26329=CARTESIAN_POINT('Ctrl Pts',(-6.59162635926391,1.53060476278405,69.6245538689757));
#26330=CARTESIAN_POINT('Ctrl Pts',(-6.633697520552,1.34942319164679,69.6333031338982));
#26331=CARTESIAN_POINT('Ctrl Pts',(-6.66829431424255,1.16650618642697,69.6420523988207));
#26332=CARTESIAN_POINT('Ctrl Pts',(-6.69529923745417,0.98247499761859,69.6508016637432));
#26333=CARTESIAN_POINT('Ctrl Pts',(-6.72230554731443,0.798434359177787,
69.6595513779229));
#26334=CARTESIAN_POINT('Ctrl Pts',(-6.74171916496702,0.613279706240395,
69.6683010921026));
#26335=CARTESIAN_POINT('Ctrl Pts',(-6.75347414817274,0.427639953655449,
69.6770508062823));
#26336=CARTESIAN_POINT('Ctrl Pts',(-6.7624883775874,0.285283364199281,69.6837604654581));
#26337=CARTESIAN_POINT('Ctrl Pts',(-6.76699999999993,0.142641701106463,
69.690470124634));
#26338=CARTESIAN_POINT('Ctrl Pts',(-6.767,3.55173088245946E-12,69.6971797838099));
#26339=CARTESIAN_POINT('',(-6.767,3.37743206882749E-12,69.3028202161898));
#26340=CARTESIAN_POINT('Ctrl Pts',(3.09917575053259,6.01559628526639,68.6513920151221));
#26341=CARTESIAN_POINT('Ctrl Pts',(2.93382384459265,6.1007839529376,68.6601414630345));
#26342=CARTESIAN_POINT('Ctrl Pts',(2.76495772122983,6.1791501026705,68.6688909109469));
#26343=CARTESIAN_POINT('Ctrl Pts',(2.5931509331671,6.25042856433178,68.6776403588593));
#26344=CARTESIAN_POINT('Ctrl Pts',(2.42134553245614,6.32170645041452,68.6863897361193));
#26345=CARTESIAN_POINT('Ctrl Pts',(2.24659977927586,6.38589665313459,68.6951391133793));
#26346=CARTESIAN_POINT('Ctrl Pts',(2.06950718689913,6.44278115439077,68.7038884906393));
#26347=CARTESIAN_POINT('Ctrl Pts',(1.89241596572853,6.49966521519726,68.712637800154));
#26348=CARTESIAN_POINT('Ctrl Pts',(1.71297821457188,6.54924360009549,68.7213871096686));
#26349=CARTESIAN_POINT('Ctrl Pts',(1.53180337335833,6.59134792173559,68.7301364191833));
#26350=CARTESIAN_POINT('Ctrl Pts',(1.3506298747777,6.63345193135307,68.7388856638594));
#26351=CARTESIAN_POINT('Ctrl Pts',(1.16771959102938,6.6680819236824,68.7476349085355));
#26352=CARTESIAN_POINT('Ctrl Pts',(0.983693746906693,6.69512028363171,68.7563841532117));
#26353=CARTESIAN_POINT('Ctrl Pts',(0.7996692054197,6.72215845218869,68.7651333359558));
#26354=CARTESIAN_POINT('Ctrl Pts',(0.614529402873285,6.74160505424581,68.7738825187));
#26355=CARTESIAN_POINT('Ctrl Pts',(0.428903127363038,6.75339404354123,68.7826317014442));
#26356=CARTESIAN_POINT('Ctrl Pts',(0.243278104163609,6.76518295330331,68.7913808251628));
#26357=CARTESIAN_POINT('Ctrl Pts',(0.0571669005387894,6.76931433552276,
68.8001299488814));
#26358=CARTESIAN_POINT('Ctrl Pts',(-0.1287984047779,6.76577415902472,68.8088790726));
#26359=CARTESIAN_POINT('Ctrl Pts',(-0.31476251725921,6.7622340052344,68.8176281401992));
#26360=CARTESIAN_POINT('Ctrl Pts',(-0.500580446819348,6.75102239665089,
68.8263772077984));
#26361=CARTESIAN_POINT('Ctrl Pts',(-0.685621118842176,6.73217741012502,
68.8351262753976));
#26362=CARTESIAN_POINT('Ctrl Pts',(-0.870660665414088,6.71333253821777,
68.8438752897834));
#26363=CARTESIAN_POINT('Ctrl Pts',(-1.0549226788545,6.68685441030618,68.8526243041692));
#26364=CARTESIAN_POINT('Ctrl Pts',(-1.23778137635219,6.65283295028183,68.861373318555));
#26365=CARTESIAN_POINT('Ctrl Pts',(-1.42999922978813,6.61707018861873,68.8705701289224));
#26366=CARTESIAN_POINT('Ctrl Pts',(-1.62066601233661,6.57297172934421,68.8797669392897));
#26367=CARTESIAN_POINT('Ctrl Pts',(-1.8090662850035,6.52070304311304,68.8889637496571));
#26368=CARTESIAN_POINT('Ctrl Pts',(-1.98831342545488,6.47097374915043,68.8977137473949));
#26369=CARTESIAN_POINT('Ctrl Pts',(-2.16550875896658,6.41384933989543,68.9064637451326));
#26370=CARTESIAN_POINT('Ctrl Pts',(-2.34005036713964,6.34952386240493,68.9152137428704));
#26371=CARTESIAN_POINT('Ctrl Pts',(-2.51458843547036,6.28519968948617,68.9239635631513));
#26372=CARTESIAN_POINT('Ctrl Pts',(-2.68647261717998,6.21367483971124,68.9327133834321));
#26373=CARTESIAN_POINT('Ctrl Pts',(-2.85511905908669,6.13519226743873,68.941463203713));
#26374=CARTESIAN_POINT('Ctrl Pts',(-3.02376230488824,6.05671118252967,68.9502128581715));
#26375=CARTESIAN_POINT('Ctrl Pts',(-3.18916767379845,5.97127275992665,68.9589625126301));
#26376=CARTESIAN_POINT('Ctrl Pts',(-3.3507733410273,5.87916720438029,68.9677121670886));
#26377=CARTESIAN_POINT('Ctrl Pts',(-3.51237616037321,5.78706327195672,68.9764616673571));
#26378=CARTESIAN_POINT('Ctrl Pts',(-3.67017916302262,5.68829258362323,68.9852111676255));
#26379=CARTESIAN_POINT('Ctrl Pts',(-3.82364636566434,5.58319061741061,68.9939606678939));
#26380=CARTESIAN_POINT('Ctrl Pts',(-3.97711106778762,5.47809036367728,69.0027100256024));
#26381=CARTESIAN_POINT('Ctrl Pts',(-4.12623987481883,5.36665920043258,69.0114593833108));
#26382=CARTESIAN_POINT('Ctrl Pts',(-4.27052628213878,5.24927559512376,69.0202087410192));
#26383=CARTESIAN_POINT('Ctrl Pts',(-4.41481053024945,5.13189374643065,69.0289579677958));
#26384=CARTESIAN_POINT('Ctrl Pts',(-4.55425230136514,5.00855981477369,69.0377071945723));
#26385=CARTESIAN_POINT('Ctrl Pts',(-4.68837800630548,4.87969268192077,69.0464564213488));
#26386=CARTESIAN_POINT('Ctrl Pts',(-4.82250188228901,4.75082730631804,69.0552055288197));
#26387=CARTESIAN_POINT('Ctrl Pts',(-4.95130963052979,4.61642907903513,69.0639546362905));
#26388=CARTESIAN_POINT('Ctrl Pts',(-5.07436379033386,4.47695444731669,69.0727037437614));
#26389=CARTESIAN_POINT('Ctrl Pts',(-5.19741643562836,4.33748153220551,69.0814527435511));
#26390=CARTESIAN_POINT('Ctrl Pts',(-5.31471544462814,4.19293255254539,69.0902017433409));
#26391=CARTESIAN_POINT('Ctrl Pts',(-5.42586245275677,4.04379841779537,69.0989507431306));
#26392=CARTESIAN_POINT('Ctrl Pts',(-5.53702160019199,3.89464799484278,69.1077006984728));
#26393=CARTESIAN_POINT('Ctrl Pts',(-5.64202723081294,3.74091164443786,69.1164506538149));
#26394=CARTESIAN_POINT('Ctrl Pts',(-5.74052265233006,3.58311159163171,69.1252006091571));
#26395=CARTESIAN_POINT('Ctrl Pts',(-5.83901427066959,3.42531763191715,69.1339502266395));
#26396=CARTESIAN_POINT('Ctrl Pts',(-5.93099603115781,3.26346052695537,69.142699844122));
#26397=CARTESIAN_POINT('Ctrl Pts',(-6.01615550622796,3.09809004466994,69.1514494616044));
#26398=CARTESIAN_POINT('Ctrl Pts',(-6.10131214578848,2.93272506863729,69.1601987877555));
#26399=CARTESIAN_POINT('Ctrl Pts',(-6.179646823288,2.76384720416778,69.1689481139067));
#26400=CARTESIAN_POINT('Ctrl Pts',(-6.2508934828862,2.59203002791459,69.1776974400578));
#26401=CARTESIAN_POINT('Ctrl Pts',(-6.32213814889385,2.42021765936886,69.1864465213893));
#26402=CARTESIAN_POINT('Ctrl Pts',(-6.38629508412638,2.24546640831767,69.1951956027209));
#26403=CARTESIAN_POINT('Ctrl Pts',(-6.44314639819863,2.06836976659882,69.2039446840525));
#26404=CARTESIAN_POINT('Ctrl Pts',(-6.50000285283748,1.89125711158111,69.2126945564869));
#26405=CARTESIAN_POINT('Ctrl Pts',(-6.54955227673294,1.71179891440085,69.2214444289213));
#26406=CARTESIAN_POINT('Ctrl Pts',(-6.59162635926426,1.53060476278256,69.2301943013557));
#26407=CARTESIAN_POINT('Ctrl Pts',(-6.63369752055237,1.34942319164499,69.2389435662782));
#26408=CARTESIAN_POINT('Ctrl Pts',(-6.66829431424293,1.16650618642484,69.2476928312007));
#26409=CARTESIAN_POINT('Ctrl Pts',(-6.69529923745453,0.982474997616134,
69.2564420961232));
#26410=CARTESIAN_POINT('Ctrl Pts',(-6.72230554731471,0.798434359175384,
69.2651918103029));
#26411=CARTESIAN_POINT('Ctrl Pts',(-6.74171916496724,0.61327970623805,69.2739415244826));
#26412=CARTESIAN_POINT('Ctrl Pts',(-6.75347414817289,0.427639953653164,
69.2826912386623));
#26413=CARTESIAN_POINT('Ctrl Pts',(-6.76248837758745,0.285283364197696,
69.2894008978381));
#26414=CARTESIAN_POINT('Ctrl Pts',(-6.76699999999993,0.142641701105583,
69.296110557014));
#26415=CARTESIAN_POINT('Ctrl Pts',(-6.767,3.37743208484225E-12,69.3028202161898));
#26416=CARTESIAN_POINT('Ctrl Pts',(-6.76699999999291,9.79885374254829E-6,
69.3030322358393));
#26417=CARTESIAN_POINT('Ctrl Pts',(-6.76700024703085,-0.170592373230755,
69.3111047379646));
#26418=CARTESIAN_POINT('Ctrl Pts',(-6.76054465261952,-0.34148283825778,
69.3191772400899));
#26419=CARTESIAN_POINT('Ctrl Pts',(-6.74759363237739,-0.512122223985705,
69.3272497422151));
#26420=CARTESIAN_POINT('Ctrl Pts',(-6.73465748998322,-0.682565582930617,
69.3353129708271));
#26421=CARTESIAN_POINT('Ctrl Pts',(-6.71524079823711,-0.852758068662661,
69.343376199439));
#26422=CARTESIAN_POINT('Ctrl Pts',(-6.68935590325772,-1.02215781538423,
69.3514394280509));
#26423=CARTESIAN_POINT('Ctrl Pts',(-6.66349507694572,-1.19140004838353,
69.359495159195));
#26424=CARTESIAN_POINT('Ctrl Pts',(-6.63117807340899,-1.35985064332614,
69.3675508903391));
#26425=CARTESIAN_POINT('Ctrl Pts',(-6.59246920217326,-1.5269704707024,69.3756066214832));
#26426=CARTESIAN_POINT('Ctrl Pts',(-6.55378785924245,-1.69397144869297,
69.3836566236918));
#26427=CARTESIAN_POINT('Ctrl Pts',(-6.50872378100871,-1.85964318114955,
69.3917066259005));
#26428=CARTESIAN_POINT('Ctrl Pts',(-6.45739273669824,-2.02345448281813,
69.3997566281092));
#26429=CARTESIAN_POINT('Ctrl Pts',(-6.40448593360075,-2.19229445868348,
69.408053749033));
#26430=CARTESIAN_POINT('Ctrl Pts',(-6.34492130354424,-2.35915755413341,
69.4163508699567));
#26431=CARTESIAN_POINT('Ctrl Pts',(-6.27888194073216,-2.52347589137435,
69.4246479908805));
#26432=CARTESIAN_POINT('Ctrl Pts',(-6.21484943481896,-2.68280079175183,
69.4326929722673));
#26433=CARTESIAN_POINT('Ctrl Pts',(-6.14473012506522,-2.83973297375626,
69.440737953654));
#26434=CARTESIAN_POINT('Ctrl Pts',(-6.06874066805516,-2.99377282102256,
69.4487829350408));
#26435=CARTESIAN_POINT('Ctrl Pts',(-5.99275166831572,-3.14781174134588,
69.4568278680164));
#26436=CARTESIAN_POINT('Ctrl Pts',(-5.91089275629488,-3.29895802662626,
69.464872800992));
#26437=CARTESIAN_POINT('Ctrl Pts',(-5.82342738705123,-3.44673504460986,
69.4729177339677));
#26438=CARTESIAN_POINT('Ctrl Pts',(-5.73594524274834,-3.59454040487626,
69.480964209888));
#26439=CARTESIAN_POINT('Ctrl Pts',(-5.64285469123482,-3.73897489061653,
69.4890106858083));
#26440=CARTESIAN_POINT('Ctrl Pts',(-5.54446342091688,-3.87958945948083,
69.4970571617286));
#26441=CARTESIAN_POINT('Ctrl Pts',(-5.44603381235406,-4.02025881893535,
69.5051067729654));
#26442=CARTESIAN_POINT('Ctrl Pts',(-5.34229958796078,-4.15710499374216,
69.5131563842021));
#26443=CARTESIAN_POINT('Ctrl Pts',(-5.23360964023565,-4.28971084499089,
69.5212059954388));
#26444=CARTESIAN_POINT('Ctrl Pts',(-5.12480134792087,-4.42246108111955,
69.5292643713126));
#26445=CARTESIAN_POINT('Ctrl Pts',(-5.01102679745427,-4.55096148893403,
69.5373227471863));
#26446=CARTESIAN_POINT('Ctrl Pts',(-4.89267321585187,-4.67483024321587,
69.5453811230601));
#26447=CARTESIAN_POINT('Ctrl Pts',(-4.77424238184176,-4.79877984979959,
69.5534447588417));
#26448=CARTESIAN_POINT('Ctrl Pts',(-4.65122683144362,-4.91809152404778,
69.5615083946234));
#26449=CARTESIAN_POINT('Ctrl Pts',(-4.52404758038812,-5.03242312314698,
69.569572030405));
#26450=CARTESIAN_POINT('Ctrl Pts',(-4.39670069411057,-5.14690542295281,
69.5776462948809));
#26451=CARTESIAN_POINT('Ctrl Pts',(-4.26517943979858,-5.25639431088611,
69.5857205593568));
#26452=CARTESIAN_POINT('Ctrl Pts',(-4.12993502195336,-5.3605900528247,69.5937948238327));
#26453=CARTESIAN_POINT('Ctrl Pts',(-4.10150064171555,-5.38249662311164,
69.5954923926485));
#26454=CARTESIAN_POINT('Ctrl Pts',(-4.0729017780956,-5.40416938177994,69.5971899614643));
#26455=CARTESIAN_POINT('Ctrl Pts',(-4.04414276360816,-5.42560580097336,
69.5988875302802));
#26456=CARTESIAN_POINT('Ctrl Pts',(-3.9047801226389,-5.52948404732367,69.6071137396137));
#26457=CARTESIAN_POINT('Ctrl Pts',(-3.76121775700442,-5.62813453010611,
69.6153399489473));
#26458=CARTESIAN_POINT('Ctrl Pts',(-3.61388435296551,-5.72119995135558,
69.6235661582808));
#26459=CARTESIAN_POINT('Ctrl Pts',(-3.4667164716947,-5.81416081759093,69.6317831258206));
#26460=CARTESIAN_POINT('Ctrl Pts',(-3.31578628869878,-5.90154892689321,
69.6400000933603));
#26461=CARTESIAN_POINT('Ctrl Pts',(-3.16155469770833,-5.98304779300637,
69.6482170609001));
#26462=CARTESIAN_POINT('Ctrl Pts',(-3.00746542378782,-6.06447145610986,
69.65642644624));
#26463=CARTESIAN_POINT('Ctrl Pts',(-2.85008112393073,-6.14001653212085,
69.6646358315799));
#26464=CARTESIAN_POINT('Ctrl Pts',(-2.68989082509428,-6.2094103060656,69.6728452169198));
#26465=CARTESIAN_POINT('Ctrl Pts',(-2.52981620056308,-6.27875397038043,
69.6810486742169));
#26466=CARTESIAN_POINT('Ctrl Pts',(-2.36693994070157,-6.34195503812928,
69.689252131514));
#26467=CARTESIAN_POINT('Ctrl Pts',(-2.20177485896343,-6.39878710932287,
69.6974555888112));
#26468=CARTESIAN_POINT('Ctrl Pts',(-2.03669591213926,-6.45558954213581,
69.7056547679396));
#26469=CARTESIAN_POINT('Ctrl Pts',(-1.86933085969487,-6.50602947896676,
69.7138539470679));
#26470=CARTESIAN_POINT('Ctrl Pts',(-1.70021172503698,-6.54992893778603,
69.7220531261963));
#26471=CARTESIAN_POINT('Ctrl Pts',(-1.53112445606874,-6.59382012500118,
69.7302507604227));
#26472=CARTESIAN_POINT('Ctrl Pts',(-1.36028410843392,-6.6311731929181,69.738448394649));
#26473=CARTESIAN_POINT('Ctrl Pts',(-1.18823737214972,-6.66186017171081,
69.7466460288754));
#26474=CARTESIAN_POINT('Ctrl Pts',(-1.01620305438703,-6.69254493548384,
69.7548430713875));
#26475=CARTESIAN_POINT('Ctrl Pts',(-0.842962874346927,-6.71656450454903,
69.7630401138996));
#26476=CARTESIAN_POINT('Ctrl Pts',(-0.669073155748615,-6.73384215082716,
69.7712371564118));
#26477=CARTESIAN_POINT('Ctrl Pts',(-0.495164384536056,-6.75112169016909,
69.7794350970511));
#26478=CARTESIAN_POINT('Ctrl Pts',(-0.320606289974542,-6.76165779956088,
69.7876330376905));
#26479=CARTESIAN_POINT('Ctrl Pts',(-0.145959805460637,-6.76542568765557,
69.7958309783299));
#26480=CARTESIAN_POINT('Ctrl Pts',(0.0287375564089473,-6.76919467339723,
69.8040313071624));
#26481=CARTESIAN_POINT('Ctrl Pts',(0.203523001014131,-6.76619150273411,
69.8122316359949));
#26482=CARTESIAN_POINT('Ctrl Pts',(0.377836053506462,-6.75644351095091,
69.8204319648274));
#26483=CARTESIAN_POINT('Ctrl Pts',(0.552330744723304,-6.7466853615073,69.8286408386154));
#26484=CARTESIAN_POINT('Ctrl Pts',(0.726351701803452,-6.73016836955846,
69.8368497124034));
#26485=CARTESIAN_POINT('Ctrl Pts',(0.89934302486302,-6.70697182964341,69.8450585861914));
#26486=CARTESIAN_POINT('Ctrl Pts',(1.07242719045789,-6.6837628404012,69.8532718655915));
#26487=CARTESIAN_POINT('Ctrl Pts',(1.24448026737596,-6.65386721803353,69.8614851449915));
#26488=CARTESIAN_POINT('Ctrl Pts',(1.41495709764256,-6.61741531202561,69.8696984243915));
#26489=CARTESIAN_POINT('Ctrl Pts',(1.58568327706861,-6.58091008937572,69.8779237170036));
#26490=CARTESIAN_POINT('Ctrl Pts',(1.75482825487382,-6.53782950742589,69.8861490096157));
#26491=CARTESIAN_POINT('Ctrl Pts',(1.92186133355828,-6.48835402968839,69.8943743022278));
#26492=CARTESIAN_POINT('Ctrl Pts',(2.07292268937523,-6.44360940302174,69.9018130913812));
#26493=CARTESIAN_POINT('Ctrl Pts',(2.22225675967473,-6.3936350772232,69.9092518805345));
#26494=CARTESIAN_POINT('Ctrl Pts',(2.36948624373537,-6.33859794755503,69.9166906696879));
#26495=CARTESIAN_POINT('Ctrl Pts',(2.53230028618154,-6.27773501902492,69.9249168707148));
#26496=CARTESIAN_POINT('Ctrl Pts',(2.69299538908088,-6.21050989780627,69.9331430717417));
#26497=CARTESIAN_POINT('Ctrl Pts',(2.85103898890883,-6.137089349498,69.9413692727686));
#26498=CARTESIAN_POINT('Ctrl Pts',(3.00890506006193,-6.0637512737015,69.9495862333924));
#26499=CARTESIAN_POINT('Ctrl Pts',(3.16412523665829,-5.98423177831405,69.9578031940162));
#26500=CARTESIAN_POINT('Ctrl Pts',(3.3161838111228,-5.89874681020021,69.9660201546399));
#26501=CARTESIAN_POINT('Ctrl Pts',(3.46810209919027,-5.81334070891922,69.9742295344495));
#26502=CARTESIAN_POINT('Ctrl Pts',(3.61686428345511,-5.72198027025017,69.9824389142591));
#26503=CARTESIAN_POINT('Ctrl Pts',(3.76197620713176,-5.62492880105824,69.9906482940687));
#26504=CARTESIAN_POINT('Ctrl Pts',(3.90698336903285,-5.52794739698555,69.9988517472172));
#26505=CARTESIAN_POINT('Ctrl Pts',(4.04834522243183,-5.42528334452511,70.0070552003656));
#26506=CARTESIAN_POINT('Ctrl Pts',(4.18559365423153,-5.31724503494589,70.015258653514));
#26507=CARTESIAN_POINT('Ctrl Pts',(4.32277053290059,-5.20926305008512,70.0234578298722));
#26508=CARTESIAN_POINT('Ctrl Pts',(4.45583798104866,-5.0959126111233,70.0316570062303));
#26509=CARTESIAN_POINT('Ctrl Pts',(4.58435817621401,-4.97754448620801,70.0398561825885));
#26510=CARTESIAN_POINT('Ctrl Pts',(4.71285418836387,-4.85919863404289,70.0480538161478));
#26511=CARTESIAN_POINT('Ctrl Pts',(4.83680438412177,-4.73583721471198,70.0562514497071));
#26512=CARTESIAN_POINT('Ctrl Pts',(4.95580503290423,-4.60785041812786,70.0644490832665));
#26513=CARTESIAN_POINT('Ctrl Pts',(5.07479711071924,-4.47987283973439,70.072646126395));
#26514=CARTESIAN_POINT('Ctrl Pts',(5.18884010664361,-4.34727080963164,70.0808431695235));
#26515=CARTESIAN_POINT('Ctrl Pts',(5.29756814212362,-4.21047037509551,70.089040212652));
#26516=CARTESIAN_POINT('Ctrl Pts',(5.40630810765516,-4.07365493029798,70.0972381551911));
#26517=CARTESIAN_POINT('Ctrl Pts',(5.50973172766425,-3.93264044414168,70.1054360977301));
#26518=CARTESIAN_POINT('Ctrl Pts',(5.60751428151198,-3.78788497484271,70.1136340402692));
#26519=CARTESIAN_POINT('Ctrl Pts',(5.70532533631333,-3.64308731326349,70.1218343722855));
#26520=CARTESIAN_POINT('Ctrl Pts',(5.79749184914728,-3.49454679375442,70.1300347043018));
#26521=CARTESIAN_POINT('Ctrl Pts',(5.88373316257174,-3.3427493282706,70.138235036318));
#26522=CARTESIAN_POINT('Ctrl Pts',(5.9700643627525,-3.19079364880273,70.1464439152965));
#26523=CARTESIAN_POINT('Ctrl Pts',(6.05045784807698,-3.0355745537015,70.1546527942749));
#26524=CARTESIAN_POINT('Ctrl Pts',(6.12467911357747,-2.87760225808013,70.1628616732534));
#26525=CARTESIAN_POINT('Ctrl Pts',(6.19894022277438,-2.71954515926731,70.1710749589484));
#26526=CARTESIAN_POINT('Ctrl Pts',(6.26702236708854,-2.55873224350469,70.1792882446435));
#26527=CARTESIAN_POINT('Ctrl Pts',(6.3287397748899,-2.39569235540095,70.1875015303385));
#26528=CARTESIAN_POINT('Ctrl Pts',(6.39054746765106,-2.2324139600386,70.1957268310581));
#26529=CARTESIAN_POINT('Ctrl Pts',(6.44597170293687,-2.06690242195696,70.2039521317777));
#26530=CARTESIAN_POINT('Ctrl Pts',(6.49487666602076,-1.89970158003278,70.2121774324973));
#26531=CARTESIAN_POINT('Ctrl Pts',(6.53910530522891,-1.74848858964412,70.2196162246968));
#26532=CARTESIAN_POINT('Ctrl Pts',(6.57800243450117,-1.59589426002877,70.2270550168962));
#26533=CARTESIAN_POINT('Ctrl Pts',(6.61150393632732,-1.44232614201103,70.2344938090957));
#26534=CARTESIAN_POINT('Ctrl Pts',(6.64821996084301,-1.27402291742043,70.2426463653059));
#26535=CARTESIAN_POINT('Ctrl Pts',(6.67856269821642,-1.10405355869292,70.2507989215161));
#26536=CARTESIAN_POINT('Ctrl Pts',(6.70238019229282,-0.932946278175195,
70.2589514777263));
#26537=CARTESIAN_POINT('Ctrl Pts',(6.72617009322831,-0.762037229565748,
70.2670945890036));
#26538=CARTESIAN_POINT('Ctrl Pts',(6.74344974919201,-0.589993241758193,
70.275237700281));
#26539=CARTESIAN_POINT('Ctrl Pts',(6.7541175053542,-0.417355632366388,70.2833808115583));
#26540=CARTESIAN_POINT('Ctrl Pts',(6.76477514542661,-0.24488173289927,70.2915162008326));
#26541=CARTESIAN_POINT('Ctrl Pts',(6.76883334602624,-0.0718156949128621,
70.299651590107));
#26542=CARTESIAN_POINT('Ctrl Pts',(6.76624184566292,0.101293069852138,70.3077869793814));
#26543=CARTESIAN_POINT('Ctrl Pts',(6.76365225824779,0.274274052231617,70.315916363417));
#26544=CARTESIAN_POINT('Ctrl Pts',(6.75442274912214,0.447297334609687,70.3240457474528));
#26545=CARTESIAN_POINT('Ctrl Pts',(6.7385550331034,0.619810508007817,70.3321751314884));
#26546=CARTESIAN_POINT('Ctrl Pts',(6.72269569705731,0.792232574678687,70.3403002222776));
#26547=CARTESIAN_POINT('Ctrl Pts',(6.70020516934282,0.964144705670353,70.3484253130669));
#26548=CARTESIAN_POINT('Ctrl Pts',(6.6711372089452,1.13499662529313,70.3565504038561));
#26549=CARTESIAN_POINT('Ctrl Pts',(6.64195828982401,1.30650072383258,70.364706509883));
#26550=CARTESIAN_POINT('Ctrl Pts',(6.60615163732752,1.47693612887344,70.37286261591));
#26551=CARTESIAN_POINT('Ctrl Pts',(6.56382402666672,1.64575306378349,70.3810187219369));
#26552=CARTESIAN_POINT('Ctrl Pts',(6.52166677700755,1.81389054096667,70.3891420011076));
#26553=CARTESIAN_POINT('Ctrl Pts',(6.47304107356705,1.98042219989944,70.3972652802783));
#26554=CARTESIAN_POINT('Ctrl Pts',(6.41810321571569,2.14481703471879,70.405388559449));
#26555=CARTESIAN_POINT('Ctrl Pts',(6.36315804242397,2.30923376010065,70.413512920303));
#26556=CARTESIAN_POINT('Ctrl Pts',(6.30189915652911,2.47151274762659,70.421637281157));
#26557=CARTESIAN_POINT('Ctrl Pts',(6.23453208593151,2.63114018430994,70.429761642011));
#26558=CARTESIAN_POINT('Ctrl Pts',(6.16714322790689,2.79081924667771,70.4378886303938));
#26559=CARTESIAN_POINT('Ctrl Pts',(6.09364239355962,2.94784471368909,70.4460156187766));
#26560=CARTESIAN_POINT('Ctrl Pts',(6.01428238284227,3.10172474914089,70.4541426071594));
#26561=CARTESIAN_POINT('Ctrl Pts',(5.93440931861393,3.25659960165164,70.4623221356048));
#26562=CARTESIAN_POINT('Ctrl Pts',(5.84860122980117,3.40828787786311,70.4705016640501));
#26563=CARTESIAN_POINT('Ctrl Pts',(5.75716122730205,3.55631601560519,70.4786811924954));
#26564=CARTESIAN_POINT('Ctrl Pts',(5.66615184533946,3.70364704098556,70.4868222008966));
#26565=CARTESIAN_POINT('Ctrl Pts',(5.56956373772252,3.84735205990366,70.4949632092979));
#26566=CARTESIAN_POINT('Ctrl Pts',(5.46773726086385,3.98699614323379,70.5031042176991));
#26567=CARTESIAN_POINT('Ctrl Pts',(5.36518807985398,4.12763133773487,70.5113030061665));
#26568=CARTESIAN_POINT('Ctrl Pts',(5.25732613262743,4.26414744429977,70.5195017946338));
#26569=CARTESIAN_POINT('Ctrl Pts',(5.14453768453907,4.39613705568394,70.5277005831012));
#26570=CARTESIAN_POINT('Ctrl Pts',(5.03174923645066,4.52812666706816,70.5358993715686));
#26571=CARTESIAN_POINT('Ctrl Pts',(4.91403458704895,4.6555895544032,70.5440981600359));
#26572=CARTESIAN_POINT('Ctrl Pts',(4.79181446060722,4.77815897340342,70.5522969485033));
#26573=CARTESIAN_POINT('Ctrl Pts',(4.66852063006232,4.90180516504276,70.560567763347));
#26574=CARTESIAN_POINT('Ctrl Pts',(4.54025684618928,5.02085771462031,70.5688385781906));
#26575=CARTESIAN_POINT('Ctrl Pts',(4.40739849221652,5.13489313723349,70.5771093930343));
#26576=CARTESIAN_POINT('Ctrl Pts',(4.27530604256738,5.24827116630976,70.5853325281299));
#26577=CARTESIAN_POINT('Ctrl Pts',(4.13867210375974,5.35668949579421,70.5935556632255));
#26578=CARTESIAN_POINT('Ctrl Pts',(3.99790500771599,5.45976597935108,70.601778798321));
#26579=CARTESIAN_POINT('Ctrl Pts',(3.85591360860525,5.5637389568934,70.6100734530388));
#26580=CARTESIAN_POINT('Ctrl Pts',(3.70971705065656,5.66227644336873,70.6183681077565));
#26581=CARTESIAN_POINT('Ctrl Pts',(3.55977124940387,5.75502542582721,70.6266627624742));
#26582=CARTESIAN_POINT('Ctrl Pts',(3.40982544815124,5.84777440828565,70.6349574171919));
#26583=CARTESIAN_POINT('Ctrl Pts',(3.25613069578252,5.93473464875063,70.6432520719096));
#26584=CARTESIAN_POINT('Ctrl Pts',(3.09917575053263,6.01559628526637,70.6515467266273));
#26585=CARTESIAN_POINT('Origin',(0.,0.,-3.69717978381041));
#26586=CARTESIAN_POINT('',(3.09917575053265,6.01559628526636,73.0456387728543));
#26587=CARTESIAN_POINT('',(3.09917575053262,6.01559628526637,72.6513920151221));
#26588=CARTESIAN_POINT('',(3.09917575053259,6.01559628526639,-3.69717978381041));
#26589=CARTESIAN_POINT('',(-6.76699866280443,0.00425412777605735,71.6971797837803));
#26590=CARTESIAN_POINT('Ctrl Pts',(-6.76699866280482,0.00425412714360294,
71.6971797838099));
#26591=CARTESIAN_POINT('Ctrl Pts',(-6.76710997009626,-0.172801298538676,
71.7054757833312));
#26592=CARTESIAN_POINT('Ctrl Pts',(-6.760268040189,-0.349875666979543,71.7137717828525));
#26593=CARTESIAN_POINT('Ctrl Pts',(-6.7464953643748,-0.526392722659913,
71.7220677823738));
#26594=CARTESIAN_POINT('Ctrl Pts',(-6.73275154850618,-0.702539895777978,
71.7303463980477));
#26595=CARTESIAN_POINT('Ctrl Pts',(-6.71210605334925,-0.878131742588406,
71.7386250137217));
#26596=CARTESIAN_POINT('Ctrl Pts',(-6.684633245895,-1.05260028874936,71.7469036293956));
#26597=CARTESIAN_POINT('Ctrl Pts',(-6.65715276890628,-1.22711754098203,
71.7551845561958));
#26598=CARTESIAN_POINT('Ctrl Pts',(-6.62284123491531,-1.4005105231155,71.763465482996));
#26599=CARTESIAN_POINT('Ctrl Pts',(-6.58182431353282,-1.57222062885213,
71.7717464097962));
#26600=CARTESIAN_POINT('Ctrl Pts',(-6.54078908784747,-1.74400736232374,
71.7800310320613));
#26601=CARTESIAN_POINT('Ctrl Pts',(-6.49304259177669,-1.91410938374628,
71.7883156543264));
#26602=CARTESIAN_POINT('Ctrl Pts',(-6.43876066150863,-2.08198226308701,
71.7966002765915));
#26603=CARTESIAN_POINT('Ctrl Pts',(-6.38433238472729,-2.25030773522326,
71.804907234569));
#26604=CARTESIAN_POINT('Ctrl Pts',(-6.32333350806107,-2.41639169931005,
71.8132141925465));
#26605=CARTESIAN_POINT('Ctrl Pts',(-6.25598989030927,-2.5797053111447,71.821521150524));
#26606=CARTESIAN_POINT('Ctrl Pts',(-6.18869916031527,-2.74289066597393,
71.8298215847002));
#26607=CARTESIAN_POINT('Ctrl Pts',(-6.1150738337816,-2.90330971843124,71.8381220188764));
#26608=CARTESIAN_POINT('Ctrl Pts',(-6.03538536448875,-3.06045952466537,
71.8464224530525));
#26609=CARTESIAN_POINT('Ctrl Pts',(-5.95556533654408,-3.21786877140359,
71.8547365905153));
#26610=CARTESIAN_POINT('Ctrl Pts',(-5.86966232667769,-3.37199767841978,
71.863050727978));
#26611=CARTESIAN_POINT('Ctrl Pts',(-5.77799260821506,-3.52237000035659,
71.8713648654408));
#26612=CARTESIAN_POINT('Ctrl Pts',(-5.68640927847976,-3.67260061275471,
71.8796711677343));
#26613=CARTESIAN_POINT('Ctrl Pts',(-5.5890703469852,-3.81908146603657,71.8879774700278));
#26614=CARTESIAN_POINT('Ctrl Pts',(-5.48633121941073,-3.96137081714388,
71.8962837723214));
#26615=CARTESIAN_POINT('Ctrl Pts',(-5.38551320208138,-4.1009995117259,71.9044347557718));
#26616=CARTESIAN_POINT('Ctrl Pts',(-5.27920294434396,-4.23699626317783,
71.9125857392222));
#26617=CARTESIAN_POINT('Ctrl Pts',(-5.1676920987235,-4.36889544081691,71.9207367226727));
#26618=CARTESIAN_POINT('Ctrl Pts',(-5.0563107831579,-4.50064140548713,71.9288782380097));
#26619=CARTESIAN_POINT('Ctrl Pts',(-4.93974113838109,-4.62829899449591,
71.9370197533468));
#26620=CARTESIAN_POINT('Ctrl Pts',(-4.81831816033767,-4.75143126918197,
71.9451612686838));
#26621=CARTESIAN_POINT('Ctrl Pts',(-4.69701067436911,-4.87444642598711,
71.9532950401777));
#26622=CARTESIAN_POINT('Ctrl Pts',(-4.57085930045932,-4.99294457905048,
71.9614288116715));
#26623=CARTESIAN_POINT('Ctrl Pts',(-4.44023937580192,-5.1065216425252,71.9695625831654));
#26624=CARTESIAN_POINT('Ctrl Pts',(-4.30971621890314,-5.2200145641824,71.97769032888));
#26625=CARTESIAN_POINT('Ctrl Pts',(-4.17473137769658,-5.32859341648519,
71.9858180745945));
#26626=CARTESIAN_POINT('Ctrl Pts',(-4.03569712435546,-5.43189080527849,
71.9939458203091));
#26627=CARTESIAN_POINT('Ctrl Pts',(-3.89673664151605,-5.5351333852746,72.0020692535046));
#26628=CARTESIAN_POINT('Ctrl Pts',(-3.75373131839898,-5.63309986499319,
72.0101926867));
#26629=CARTESIAN_POINT('Ctrl Pts',(-3.60712658657559,-5.72546301956615,
72.0183161198954));
#26630=CARTESIAN_POINT('Ctrl Pts',(-3.45959189018067,-5.81841206560659,
72.0264910828401));
#26631=CARTESIAN_POINT('Ctrl Pts',(-3.30841224985171,-5.90568621161012,
72.0346660457848));
#26632=CARTESIAN_POINT('Ctrl Pts',(-3.15407179309374,-5.98699591815549,
72.0428410087295));
#26633=CARTESIAN_POINT('Ctrl Pts',(-3.00073898990254,-6.06777477221062,
72.0509625992095));
#26634=CARTESIAN_POINT('Ctrl Pts',(-2.84428685973461,-6.14266668689104,
72.0590841896896));
#26635=CARTESIAN_POINT('Ctrl Pts',(-2.68521500197278,-6.21143376308404,
72.0672057801696));
#26636=CARTESIAN_POINT('Ctrl Pts',(-2.52612214344734,-6.28020991794834,
72.075328442867));
#26637=CARTESIAN_POINT('Ctrl Pts',(-2.36440920441213,-6.34285947848565,
72.0834511055644));
#26638=CARTESIAN_POINT('Ctrl Pts',(-2.20059583500245,-6.39919268118799,
72.0915737682618));
#26639=CARTESIAN_POINT('Ctrl Pts',(-2.03672964396345,-6.45554404853441,
72.0996990501122));
#26640=CARTESIAN_POINT('Ctrl Pts',(-1.87076201978423,-6.50557488337561,
72.1078243319625));
#26641=CARTESIAN_POINT('Ctrl Pts',(-1.70322779292431,-6.54914529426628,
72.1159496138129));
#26642=CARTESIAN_POINT('Ctrl Pts',(-1.53386839200249,-6.59319037582763,
72.1241634152092));
#26643=CARTESIAN_POINT('Ctrl Pts',(-1.36290842597664,-6.63063334804685,
72.1323772166055));
#26644=CARTESIAN_POINT('Ctrl Pts',(-1.19091005837655,-6.66138290693889,
72.1405910180017));
#26645=CARTESIAN_POINT('Ctrl Pts',(-1.02047087970615,-6.69185371683762,
72.1487303601552));
#26646=CARTESIAN_POINT('Ctrl Pts',(-0.849012418815287,-6.71575198123387,
72.1568697023087));
#26647=CARTESIAN_POINT('Ctrl Pts',(-0.677085565759804,-6.73304122493244,
72.1650090444622));
#26648=CARTESIAN_POINT('Ctrl Pts',(-0.502799515293674,-6.75056771335597,
72.1732600754798));
#26649=CARTESIAN_POINT('Ctrl Pts',(-0.328032516604215,-6.76130246251573,
72.1815111064974));
#26650=CARTESIAN_POINT('Ctrl Pts',(-0.153356693526112,-6.76526205882305,
72.1897621375151));
#26651=CARTESIAN_POINT('Ctrl Pts',(0.0213191295519908,-6.76922165513038,
72.1980131685327));
#26652=CARTESIAN_POINT('Ctrl Pts',(0.195903394273016,-6.76640617183079,
72.2062641995503));
#26653=CARTESIAN_POINT('Ctrl Pts',(0.369831528183824,-6.75688638655122,
72.214515230568));
#26654=CARTESIAN_POINT('Ctrl Pts',(0.543353537741656,-6.74738883008853,
72.2227469953257));
#26655=CARTESIAN_POINT('Ctrl Pts',(0.716764193046762,-6.73118877289631,
72.2309787600834));
#26656=CARTESIAN_POINT('Ctrl Pts',(0.889505497419388,-6.70828360835025,
72.2392105248411));
#26657=CARTESIAN_POINT('Ctrl Pts',(1.06204053146055,-6.68540579485322,72.2474324600514));
#26658=CARTESIAN_POINT('Ctrl Pts',(1.23390745439928,-6.65583886355904,72.2556543952617));
#26659=CARTESIAN_POINT('Ctrl Pts',(1.40454935786716,-6.61963217265997,72.263876330472));
#26660=CARTESIAN_POINT('Ctrl Pts',(1.57502168768379,-6.58346146179072,72.2720900952181));
#26661=CARTESIAN_POINT('Ctrl Pts',(1.74427107428641,-6.54066420544886,72.2803038599641));
#26662=CARTESIAN_POINT('Ctrl Pts',(1.91174672088437,-6.49134142340301,72.2885176247101));
#26663=CARTESIAN_POINT('Ctrl Pts',(2.07908948347132,-6.44205777665383,72.296724872222));
#26664=CARTESIAN_POINT('Ctrl Pts',(2.24466096707993,-6.3862590178193,72.3049321197339));
#26665=CARTESIAN_POINT('Ctrl Pts',(2.40792145601167,-6.32409703133014,72.3131393672457));
#26666=CARTESIAN_POINT('Ctrl Pts',(2.57108509590641,-6.26197192044125,72.3213417460719));
#26667=CARTESIAN_POINT('Ctrl Pts',(2.73194013820082,-6.19349122886557,72.3295441248979));
#26668=CARTESIAN_POINT('Ctrl Pts',(2.88996281538841,-6.11885642303137,72.337746503724));
#26669=CARTESIAN_POINT('Ctrl Pts',(3.04793832801866,-6.04424389322516,72.3459464344106));
#26670=CARTESIAN_POINT('Ctrl Pts',(3.20308283423616,-5.96348105731483,72.3541463650972));
#26671=CARTESIAN_POINT('Ctrl Pts',(3.35489309014139,-5.87681728095417,72.3623462957837));
#26672=CARTESIAN_POINT('Ctrl Pts',(3.50668211989362,-5.79016562194728,72.3705450799537));
#26673=CARTESIAN_POINT('Ctrl Pts',(3.65513751625434,-5.69761484265509,72.3787438641236));
#26674=CARTESIAN_POINT('Ctrl Pts',(3.79978115629632,-5.59945998862885,72.3869426482935));
#26675=CARTESIAN_POINT('Ctrl Pts',(3.94443081146807,-5.50130105274887,72.3951417734169));
#26676=CARTESIAN_POINT('Ctrl Pts',(4.08526809787329,-5.397537779052,72.4033408985403));
#26677=CARTESIAN_POINT('Ctrl Pts',(4.22184433275263,-5.28850824240679,72.4115400236636));
#26678=CARTESIAN_POINT('Ctrl Pts',(4.35845102294825,-5.17945439312017,72.4197409771209));
#26679=CARTESIAN_POINT('Ctrl Pts',(4.49079448907771,-5.06513216553043,72.4279419305781));
#26680=CARTESIAN_POINT('Ctrl Pts',(4.618459521793,-4.94591959554132,72.4361428840353));
#26681=CARTESIAN_POINT('Ctrl Pts',(4.74624420950643,-4.82659529268741,72.4443515238969));
#26682=CARTESIAN_POINT('Ctrl Pts',(4.869341440735,-4.70237173481074,72.4525601637585));
#26683=CARTESIAN_POINT('Ctrl Pts',(4.98737259226172,-4.57366413567466,72.4607688036201));
#26684=CARTESIAN_POINT('Ctrl Pts',(5.10546009610742,-4.44489508689934,72.4689813625818));
#26685=CARTESIAN_POINT('Ctrl Pts',(5.218476466004,-4.31163800160049,72.4771939215434));
#26686=CARTESIAN_POINT('Ctrl Pts',(5.3260837968463,-4.17434071309127,72.4854064805051));
#26687=CARTESIAN_POINT('Ctrl Pts',(5.43383878278655,-4.03685502993994,72.4936303084592));
#26688=CARTESIAN_POINT('Ctrl Pts',(5.53616968615477,-3.89531835452426,72.5018541364133));
#26689=CARTESIAN_POINT('Ctrl Pts',(5.63278162498075,-3.7502080162678,72.5100779643675));
#26690=CARTESIAN_POINT('Ctrl Pts',(5.7215508871709,-3.61687731387508,72.51763420585));
#26691=CARTESIAN_POINT('Ctrl Pts',(5.80549240220805,-3.48053009560183,72.5251904473325));
#26692=CARTESIAN_POINT('Ctrl Pts',(5.88441226823254,-3.34155371907656,72.5327466888151));
#26693=CARTESIAN_POINT('Ctrl Pts',(5.97471142243015,-3.18253863344799,72.5413924487378));
#26694=CARTESIAN_POINT('Ctrl Pts',(6.05864195515587,-3.01971896039609,72.5500382086606));
#26695=CARTESIAN_POINT('Ctrl Pts',(6.13588950645292,-2.85362032593703,72.5586839685834));
#26696=CARTESIAN_POINT('Ctrl Pts',(6.21303788316409,-2.68773493789175,72.5673186286118));
#26697=CARTESIAN_POINT('Ctrl Pts',(6.28352025936741,-2.51857925802448,72.5759532886402));
#26698=CARTESIAN_POINT('Ctrl Pts',(6.3470677158327,-2.34670415916328,72.5845879486686));
#26699=CARTESIAN_POINT('Ctrl Pts',(6.41285895373634,-2.16876036490517,72.5935274877744));
#26700=CARTESIAN_POINT('Ctrl Pts',(6.47121642530732,-1.98790187377263,72.6024670268802));
#26701=CARTESIAN_POINT('Ctrl Pts',(6.52189446506045,-1.80476635236085,72.611406565986));
#26702=CARTESIAN_POINT('Ctrl Pts',(6.57070828173273,-1.62836758453311,72.6200172586089));
#26703=CARTESIAN_POINT('Ctrl Pts',(6.61239743854976,-1.44985664561382,72.6286279512318));
#26704=CARTESIAN_POINT('Ctrl Pts',(6.64679165257546,-1.26982271489104,72.6372386438547));
#26705=CARTESIAN_POINT('Ctrl Pts',(6.68115330679366,-1.08995921603576,72.645841185034));
#26706=CARTESIAN_POINT('Ctrl Pts',(6.70823372962631,-0.908575898445952,
72.6544437262134));
#26707=CARTESIAN_POINT('Ctrl Pts',(6.72791303388148,-0.726274884962787,
72.6630462673927));
#26708=CARTESIAN_POINT('Ctrl Pts',(6.74757018639307,-0.544179076158229,
72.6716391252375));
#26709=CARTESIAN_POINT('Ctrl Pts',(6.75984280769998,-0.361167934827881,
72.6802319830824));
#26710=CARTESIAN_POINT('Ctrl Pts',(6.76466242796618,-0.17785172381141,72.6888248409272));
#26711=CARTESIAN_POINT('Ctrl Pts',(6.76523034021714,-0.156250951077203,
72.6898373665975));
#26712=CARTESIAN_POINT('Ctrl Pts',(6.76569482857818,-0.134645951108895,
72.6908498922679));
#26713=CARTESIAN_POINT('Ctrl Pts',(6.76605582831728,-0.113037728629765,
72.6918624179382));
#26714=CARTESIAN_POINT('Ctrl Pts',(6.76912031005088,0.0703917753572885,
72.7004576219937));
#26715=CARTESIAN_POINT('Ctrl Pts',(6.76471943308091,0.253837892281212,72.7090528260492));
#26716=CARTESIAN_POINT('Ctrl Pts',(6.75289517804965,0.436687204156235,72.7176480301047));
#26717=CARTESIAN_POINT('Ctrl Pts',(6.74105985136034,0.619707727245074,72.7262512822917));
#26718=CARTESIAN_POINT('Ctrl Pts',(6.72178729207275,0.802130025140826,72.7348545344788));
#26719=CARTESIAN_POINT('Ctrl Pts',(6.6951712328786,0.983346918658345,72.7434577866658));
#26720=CARTESIAN_POINT('Ctrl Pts',(6.66745140268478,1.17207889734512,72.7524178166988));
#26721=CARTESIAN_POINT('Ctrl Pts',(6.63176608822662,1.35950298913168,72.7613778467318));
#26722=CARTESIAN_POINT('Ctrl Pts',(6.58827941477441,1.54494768612398,72.7703378767648));
#26723=CARTESIAN_POINT('Ctrl Pts',(6.54641010443929,1.72349529512664,72.7789646639684));
#26724=CARTESIAN_POINT('Ctrl Pts',(6.49730939112459,1.90020781690629,72.787591451172));
#26725=CARTESIAN_POINT('Ctrl Pts',(6.44117420192469,2.07450329005763,72.7962182383755));
#26726=CARTESIAN_POINT('Ctrl Pts',(6.38498536309693,2.24896534120404,72.8048532703883));
#26727=CARTESIAN_POINT('Ctrl Pts',(6.32174873097116,2.42100544554549,72.813488302401));
#26728=CARTESIAN_POINT('Ctrl Pts',(6.25170947614221,2.59006131701813,72.8221233344138));
#26729=CARTESIAN_POINT('Ctrl Pts',(6.1815661980465,2.75936827260152,72.8307711912951));
#26730=CARTESIAN_POINT('Ctrl Pts',(6.10460023137856,2.92568185962392,72.8394190481764));
#26731=CARTESIAN_POINT('Ctrl Pts',(6.02110345828126,3.08846274782027,72.8480669050578));
#26732=CARTESIAN_POINT('Ctrl Pts',(6.01173391866099,3.10672910620517,72.8490373190591));
#26733=CARTESIAN_POINT('Ctrl Pts',(6.00228218838025,3.12495100935973,72.8500077330604));
#26734=CARTESIAN_POINT('Ctrl Pts',(5.99274871423678,3.14312771741994,72.8509781470618));
#26735=CARTESIAN_POINT('Ctrl Pts',(5.91195798973253,3.2971648911917,72.8592018490467));
#26736=CARTESIAN_POINT('Ctrl Pts',(5.82511795541957,3.44828807780692,72.8674255510317));
#26737=CARTESIAN_POINT('Ctrl Pts',(5.73246370899244,3.59599065976049,72.8756492530166));
#26738=CARTESIAN_POINT('Ctrl Pts',(5.63990139356365,3.74354669208099,72.8838647954928));
#26739=CARTESIAN_POINT('Ctrl Pts',(5.54153653989995,3.88768857565882,72.892080337969));
#26740=CARTESIAN_POINT('Ctrl Pts',(5.43765081670197,4.02793279432769,72.9002958804452));
#26741=CARTESIAN_POINT('Ctrl Pts',(5.33384931557788,4.16806331441907,72.9085047624294));
#26742=CARTESIAN_POINT('Ctrl Pts',(5.22453606946594,4.30430217536412,72.9167136444136));
#26743=CARTESIAN_POINT('Ctrl Pts',(5.11003689418772,4.43619340651874,72.9249225263979));
#26744=CARTESIAN_POINT('Ctrl Pts',(4.99560976981379,4.56800164246882,72.9331262427783));
#26745=CARTESIAN_POINT('Ctrl Pts',(4.87600344979385,4.69546742774049,72.9413299591588));
#26746=CARTESIAN_POINT('Ctrl Pts',(4.75158504079528,4.81816651850997,72.9495336755393));
#26747=CARTESIAN_POINT('Ctrl Pts',(4.62721570596386,4.94081721326043,72.9577341561401));
#26748=CARTESIAN_POINT('Ctrl Pts',(4.49803831604578,5.05870470586012,72.965934636741));
#26749=CARTESIAN_POINT('Ctrl Pts',(4.36445807469834,5.17144029398005,72.9741351173419));
#26750=CARTESIAN_POINT('Ctrl Pts',(4.23091161640792,5.28414737075158,72.9823335240035));
#26751=CARTESIAN_POINT('Ctrl Pts',(4.09296479954159,5.39170490879654,72.9905319306652));
#26752=CARTESIAN_POINT('Ctrl Pts',(3.95105725379949,5.49376333465489,72.9987303373268));
#26753=CARTESIAN_POINT('Ctrl Pts',(3.80912557661074,5.59583911559782,73.0069301381315));
#26754=CARTESIAN_POINT('Ctrl Pts',(3.66323211271051,5.6924137021884,73.0151299389361));
#26755=CARTESIAN_POINT('Ctrl Pts',(3.5138472998094,5.78317958856737,73.0233297397407));
#26756=CARTESIAN_POINT('Ctrl Pts',(3.37837121459391,5.86549456235173,73.0307660841119));
#26757=CARTESIAN_POINT('Ctrl Pts',(3.24002419105521,5.94303256079619,73.0382024284831));
#26758=CARTESIAN_POINT('Ctrl Pts',(3.09917575053266,6.01559628526635,73.0456387728543));
#26759=CARTESIAN_POINT('Ctrl Pts',(3.09917575053257,6.0155962852664,71.0459800471047));
#26760=CARTESIAN_POINT('Ctrl Pts',(2.94528128221868,6.09488119431318,71.0541034550639));
#26761=CARTESIAN_POINT('Ctrl Pts',(2.78825364105546,6.16830242277946,71.062226863023));
#26762=CARTESIAN_POINT('Ctrl Pts',(2.62858557352308,6.23560958388724,71.0703502709822));
#26763=CARTESIAN_POINT('Ctrl Pts',(2.46894669294983,6.30290444139925,71.0784721940009));
#26764=CARTESIAN_POINT('Ctrl Pts',(2.30666868121677,6.36408730878024,71.0865941170196));
#26765=CARTESIAN_POINT('Ctrl Pts',(2.14226612133535,6.41895512255529,71.0947160400382));
#26766=CARTESIAN_POINT('Ctrl Pts',(1.97787374744511,6.47381953685124,71.1028374598419));
#26767=CARTESIAN_POINT('Ctrl Pts',(1.81135743428406,6.52236955980444,71.1109588796455));
#26768=CARTESIAN_POINT('Ctrl Pts',(1.64324870502509,6.5644514388815,71.1190802994492));
#26769=CARTESIAN_POINT('Ctrl Pts',(1.47511838094152,6.60653872369091,71.12720276251));
#26770=CARTESIAN_POINT('Ctrl Pts',(1.30539558840919,6.64215612106347,71.1353252255708));
#26771=CARTESIAN_POINT('Ctrl Pts',(1.13462382372935,6.67120062497193,71.1434476886317));
#26772=CARTESIAN_POINT('Ctrl Pts',(0.963797602644333,6.70025439071166,71.151572741817));
#26773=CARTESIAN_POINT('Ctrl Pts',(0.791922103931048,6.72273102820475,71.1596977950024));
#26774=CARTESIAN_POINT('Ctrl Pts',(0.619547709861253,6.73857920003955,71.1678228481878));
#26775=CARTESIAN_POINT('Ctrl Pts',(0.446986941157791,6.75444450723391,71.1759566863427));
#26776=CARTESIAN_POINT('Ctrl Pts',(0.27392656437441,6.76366700033922,71.1840905244977));
#26777=CARTESIAN_POINT('Ctrl Pts',(0.100919640950755,6.76624742572058,71.1922243626527));
#26778=CARTESIAN_POINT('Ctrl Pts',(-0.0721868955381545,6.76882933684643,
71.2003628840685));
#26779=CARTESIAN_POINT('Ctrl Pts',(-0.24523955230309,6.76476156860712,71.2085014054843));
#26780=CARTESIAN_POINT('Ctrl Pts',(-0.417688915932793,6.7540969025849,71.2166399269001));
#26781=CARTESIAN_POINT('Ctrl Pts',(-0.59039269941501,6.74341650265274,71.224790455327));
#26782=CARTESIAN_POINT('Ctrl Pts',(-0.762491048290902,6.72611979841986,
71.2329409837539));
#26783=CARTESIAN_POINT('Ctrl Pts',(-0.933442180150514,6.70231114588959,
71.2410915121808));
#26784=CARTESIAN_POINT('Ctrl Pts',(-1.06438675730829,6.68407427372409,71.2473346267297));
#26785=CARTESIAN_POINT('Ctrl Pts',(-1.19465840221116,6.66201776807838,71.2535777412787));
#26786=CARTESIAN_POINT('Ctrl Pts',(-1.32401957757086,6.63620834198333,71.2598208558276));
#26787=CARTESIAN_POINT('Ctrl Pts',(-1.49444388145069,6.60220622764293,71.2680457227406));
#26788=CARTESIAN_POINT('Ctrl Pts',(-1.66379679169306,6.5615871648036,71.2762705896536));
#26789=CARTESIAN_POINT('Ctrl Pts',(-1.83152606531344,6.51443023387905,71.2844954565667));
#26790=CARTESIAN_POINT('Ctrl Pts',(-1.99906637308398,6.46732643052929,71.2927110572441));
#26791=CARTESIAN_POINT('Ctrl Pts',(-2.16498634442235,6.41369952218237,71.3009266579215));
#26792=CARTESIAN_POINT('Ctrl Pts',(-2.32874247392045,6.3536798384998,71.3091422585989));
#26793=CARTESIAN_POINT('Ctrl Pts',(-2.49234701567201,6.29371571456102,71.3173502541602));
#26794=CARTESIAN_POINT('Ctrl Pts',(-2.65379136996565,6.22737072327476,71.3255582497214));
#26795=CARTESIAN_POINT('Ctrl Pts',(-2.81254569725204,6.15482539970624,71.3337662452826));
#26796=CARTESIAN_POINT('Ctrl Pts',(-2.97118495356932,6.08233265965358,71.3419682913871));
#26797=CARTESIAN_POINT('Ctrl Pts',(-3.12713774158111,6.00364868748302,71.3501703374915));
#26798=CARTESIAN_POINT('Ctrl Pts',(-3.27989268945061,5.9190026985708,71.358372383596));
#26799=CARTESIAN_POINT('Ctrl Pts',(-3.43256758949943,5.83440106649964,71.3665701316013));
#26800=CARTESIAN_POINT('Ctrl Pts',(-3.58204767471219,5.74384381519619,71.3747678796066));
#26801=CARTESIAN_POINT('Ctrl Pts',(-3.72784466929285,5.64760684906668,71.3829656276119));
#26802=CARTESIAN_POINT('Ctrl Pts',(-3.8736138560854,5.55138823816575,71.3911618120648));
#26803=CARTESIAN_POINT('Ctrl Pts',(-4.01570104893917,5.4494922624656,71.3993579965177));
#26804=CARTESIAN_POINT('Ctrl Pts',(-4.15364529628144,5.34223920773669,71.4075541809706));
#26805=CARTESIAN_POINT('Ctrl Pts',(-4.29157933885618,5.23499408731828,71.4157497590905));
#26806=CARTESIAN_POINT('Ctrl Pts',(-4.42537076246738,5.12239289666284,71.4239453372103));
#26807=CARTESIAN_POINT('Ctrl Pts',(-4.55459022422153,5.00479738744994,71.4321409153302));
#26808=CARTESIAN_POINT('Ctrl Pts',(-4.68382363661001,4.88718918253372,71.440337378251));
#26809=CARTESIAN_POINT('Ctrl Pts',(-4.80848383831349,4.76458582639101,71.448533841172));
#26810=CARTESIAN_POINT('Ctrl Pts',(-4.92817697687412,4.63738726920751,71.4567303040928));
#26811=CARTESIAN_POINT('Ctrl Pts',(-5.04790481445122,4.51015183718821,71.4649291431666));
#26812=CARTESIAN_POINT('Ctrl Pts',(-5.1626624748459,4.37831881191929,71.4731279822405));
#26813=CARTESIAN_POINT('Ctrl Pts',(-5.2720951319704,4.24232270336121,71.4813268213143));
#26814=CARTESIAN_POINT('Ctrl Pts',(-5.3816420947562,4.1061845428277,71.4895342243191));
#26815=CARTESIAN_POINT('Ctrl Pts',(-5.48585271661665,3.96587489127608,71.4977416273239));
#26816=CARTESIAN_POINT('Ctrl Pts',(-5.58441382762827,3.82185965228895,71.5059490303287));
#26817=CARTESIAN_POINT('Ctrl Pts',(-5.68302773324149,3.6777672710386,71.5141608296574));
#26818=CARTESIAN_POINT('Ctrl Pts',(-5.77598590437935,3.52996564884307,71.5223726289861));
#26819=CARTESIAN_POINT('Ctrl Pts',(-5.86302028930166,3.37894689026583,71.5305844283148));
#26820=CARTESIAN_POINT('Ctrl Pts',(-5.95018280115931,3.22770581069748,71.5388083165747));
#26821=CARTESIAN_POINT('Ctrl Pts',(-6.03140393182022,3.0732384474288,71.5470322048345));
#26822=CARTESIAN_POINT('Ctrl Pts',(-6.10646253281745,2.91605972766277,71.5552560930943));
#26823=CARTESIAN_POINT('Ctrl Pts',(-6.17581547150636,2.77082912157225,71.5628548334211));
#26824=CARTESIAN_POINT('Ctrl Pts',(-6.23990762182496,2.62328413230967,71.5704535737478));
#26825=CARTESIAN_POINT('Ctrl Pts',(-6.29860228027418,2.47384282340752,71.5780523140746));
#26826=CARTESIAN_POINT('Ctrl Pts',(-6.37026715086443,2.29137831392281,71.5873302067577));
#26827=CARTESIAN_POINT('Ctrl Pts',(-6.43405481597993,2.10565672200331,71.5966080994409));
#26828=CARTESIAN_POINT('Ctrl Pts',(-6.48969440919368,1.91733029895224,71.605885992124));
#26829=CARTESIAN_POINT('Ctrl Pts',(-6.54508447752907,1.72984845662311,71.6151222765763));
#26830=CARTESIAN_POINT('Ctrl Pts',(-6.59239930158858,1.53978526431313,71.6243585610285));
#26831=CARTESIAN_POINT('Ctrl Pts',(-6.63141809376621,1.34780676124961,71.6335948454807));
#26832=CARTESIAN_POINT('Ctrl Pts',(-6.67031674077142,1.15641939104959,71.6428026899191));
#26833=CARTESIAN_POINT('Ctrl Pts',(-6.70097026540113,0.963128656625589,
71.6520105343576));
#26834=CARTESIAN_POINT('Ctrl Pts',(-6.72320763806499,0.768614373704144,
71.661218378796));
#26835=CARTESIAN_POINT('Ctrl Pts',(-6.74533483520506,0.575063815829266,
71.6703806027783));
#26836=CARTESIAN_POINT('Ctrl Pts',(-6.75912898518562,0.38030198423871,71.6795428267606));
#26837=CARTESIAN_POINT('Ctrl Pts',(-6.76447027988159,0.185015763108659,
71.6887050507429));
#26838=CARTESIAN_POINT('Ctrl Pts',(-6.76611711609041,0.124804814575345,
71.6915299617554));
#26839=CARTESIAN_POINT('Ctrl Pts',(-6.76696076101341,0.0645441290638371,
71.6943548727678));
#26840=CARTESIAN_POINT('Ctrl Pts',(-6.76699866280442,0.00425412777616787,
71.6971797837803));
#26841=CARTESIAN_POINT('',(-6.767,3.33069726313195E-12,71.3028202161898));
#26842=CARTESIAN_POINT('Ctrl Pts',(3.09917575053263,6.01559628526637,70.6515467266273));
#26843=CARTESIAN_POINT('Ctrl Pts',(2.9439427023012,6.09557081745671,70.659750383631));
#26844=CARTESIAN_POINT('Ctrl Pts',(2.78552095797009,6.16957970902551,70.6679540406346));
#26845=CARTESIAN_POINT('Ctrl Pts',(2.6244105723732,6.23736788618531,70.6761576976383));
#26846=CARTESIAN_POINT('Ctrl Pts',(2.46334681024357,6.30513644623696,70.6843589805992));
#26847=CARTESIAN_POINT('Ctrl Pts',(2.29959628492877,6.36668773544609,70.6925602635602));
#26848=CARTESIAN_POINT('Ctrl Pts',(2.13368096420307,6.42181396047857,70.7007615465212));
#26849=CARTESIAN_POINT('Ctrl Pts',(1.96778778005423,6.47693283051869,70.7089617352593));
#26850=CARTESIAN_POINT('Ctrl Pts',(1.79973071539011,6.5256282300274,70.7171619239975));
#26851=CARTESIAN_POINT('Ctrl Pts',(1.63004892512788,6.56774158304736,70.7253621127356));
#26852=CARTESIAN_POINT('Ctrl Pts',(1.46035902418122,6.60985694905949,70.7335626934377));
#26853=CARTESIAN_POINT('Ctrl Pts',(1.28904459066358,6.64538955544581,70.7417632741398));
#26854=CARTESIAN_POINT('Ctrl Pts',(1.11665710991708,6.67423148376438,70.7499638548418));
#26855=CARTESIAN_POINT('Ctrl Pts',(0.944230149166233,6.70308001743184,70.7581663136325));
#26856=CARTESIAN_POINT('Ctrl Pts',(0.770730005020289,6.72523476202848,70.7663687724232));
#26857=CARTESIAN_POINT('Ctrl Pts',(0.596715517112192,6.74063940525211,70.7745712312139));
#26858=CARTESIAN_POINT('Ctrl Pts',(0.422537942991574,6.75605848569272,70.7827813773411));
#26859=CARTESIAN_POINT('Ctrl Pts',(0.247845419383574,6.76471479416275,70.7909915234684));
#26860=CARTESIAN_POINT('Ctrl Pts',(0.0731999817781087,6.76660407905381,
70.7992016695956));
#26861=CARTESIAN_POINT('Ctrl Pts',(-0.101529741369486,6.76849427573165,
70.8074157780171));
#26862=CARTESIAN_POINT('Ctrl Pts',(-0.276211975285269,6.76361094738318,
70.8156298864387));
#26863=CARTESIAN_POINT('Ctrl Pts',(-0.450287629949019,6.7520019290811,70.8238439948602));
#26864=CARTESIAN_POINT('Ctrl Pts',(-0.624599517681842,6.74037715651386,
70.8320692504122));
#26865=CARTESIAN_POINT('Ctrl Pts',(-0.798302824744355,6.72200849130114,
70.8402945059643));
#26866=CARTESIAN_POINT('Ctrl Pts',(-0.970845301162993,6.69699547567488,
70.8485197615163));
#26867=CARTESIAN_POINT('Ctrl Pts',(-1.12174326554916,6.67512020635276,70.8557132036479));
#26868=CARTESIAN_POINT('Ctrl Pts',(-1.27175336889713,6.6481638471377,70.8629066457795));
#26869=CARTESIAN_POINT('Ctrl Pts',(-1.4205150722726,6.61622444672537,70.8701000879111));
#26870=CARTESIAN_POINT('Ctrl Pts',(-1.59931525177151,6.57783573244453,70.8787460546831));
#26871=CARTESIAN_POINT('Ctrl Pts',(-1.77671762482904,6.53216062412131,70.8873920214552));
#26872=CARTESIAN_POINT('Ctrl Pts',(-1.95212060784793,6.47931432579215,70.8960379882273));
#26873=CARTESIAN_POINT('Ctrl Pts',(-2.12729922655089,6.42653562507947,70.9046728956298));
#26874=CARTESIAN_POINT('Ctrl Pts',(-2.30048326441725,6.3666041132729,70.9133078030323));
#26875=CARTESIAN_POINT('Ctrl Pts',(-2.47108253964659,6.2996857129744,70.9219427104347));
#26876=CARTESIAN_POINT('Ctrl Pts',(-2.64734556468008,6.23054567910755,70.9308642893664));
#26877=CARTESIAN_POINT('Ctrl Pts',(-2.82084893431632,6.15394690570235,70.9397858682981));
#26878=CARTESIAN_POINT('Ctrl Pts',(-2.99095705046808,6.07012890491259,70.9487074472297));
#26879=CARTESIAN_POINT('Ctrl Pts',(-3.15514447480237,5.98922822848487,70.9573185064721));
#26880=CARTESIAN_POINT('Ctrl Pts',(-3.31616868156277,5.90160250839127,70.9659295657144));
#26881=CARTESIAN_POINT('Ctrl Pts',(-3.47347649773597,5.80751668268597,70.9745406249567));
#26882=CARTESIAN_POINT('Ctrl Pts',(-3.63063596528066,5.71351958431505,70.9831435635674));
#26883=CARTESIAN_POINT('Ctrl Pts',(-3.78408576889572,5.61307468256466,70.9917465021781));
#26884=CARTESIAN_POINT('Ctrl Pts',(-3.93329660906198,5.50649314765228,71.0003494407888));
#26885=CARTESIAN_POINT('Ctrl Pts',(-4.08234036746297,5.40003095950438,71.0089427460903));
#26886=CARTESIAN_POINT('Ctrl Pts',(-4.22715438425042,5.28744602375377,71.0175360513917));
#26887=CARTESIAN_POINT('Ctrl Pts',(-4.36723749492794,5.16909331149048,71.0261293566931));
#26888=CARTESIAN_POINT('Ctrl Pts',(-4.38284502636412,5.15590689902238,71.0270867903337));
#26889=CARTESIAN_POINT('Ctrl Pts',(-4.39839385969793,5.14264893227633,71.0280442239742));
#26890=CARTESIAN_POINT('Ctrl Pts',(-4.4138833242873,5.12931993538895,71.0290016576147));
#26891=CARTESIAN_POINT('Ctrl Pts',(-4.55294640901641,5.00965334440973,71.0375974147313));
#26892=CARTESIAN_POINT('Ctrl Pts',(-4.6870585652526,4.88439841367468,71.0461931718478));
#26893=CARTESIAN_POINT('Ctrl Pts',(-4.81578937574708,4.75399428780069,71.0547889289644));
#26894=CARTESIAN_POINT('Ctrl Pts',(-4.94464029633862,4.62346849057112,71.0633927062061));
#26895=CARTESIAN_POINT('Ctrl Pts',(-5.06809963465862,4.48778412577931,71.0719964834479));
#26896=CARTESIAN_POINT('Ctrl Pts',(-5.18577603295225,4.34741485667725,71.0806002606897));
#26897=CARTESIAN_POINT('Ctrl Pts',(-5.30807722583018,4.20152894154455,71.0895421745755));
#26898=CARTESIAN_POINT('Ctrl Pts',(-5.42413150450199,4.05058272992237,71.0984840884612));
#26899=CARTESIAN_POINT('Ctrl Pts',(-5.53354862518995,3.89514166785477,71.107426002347));
#26900=CARTESIAN_POINT('Ctrl Pts',(-5.63911479380902,3.74517137741593,71.1160532042246));
#26901=CARTESIAN_POINT('Ctrl Pts',(-5.73850291385411,3.59101751378756,71.1246804061022));
#26902=CARTESIAN_POINT('Ctrl Pts',(-5.83140896297384,3.43321401991608,71.1333076079797));
#26903=CARTESIAN_POINT('Ctrl Pts',(-5.92440349085702,3.27526024241789,71.141943025944));
#26904=CARTESIAN_POINT('Ctrl Pts',(-6.01090347907038,3.11365016409605,71.1505784439083));
#26905=CARTESIAN_POINT('Ctrl Pts',(-6.09065166593395,2.94894070544934,71.1592138618726));
#26906=CARTESIAN_POINT('Ctrl Pts',(-6.1705176693811,2.78398791204526,71.1678620374365));
#26907=CARTESIAN_POINT('Ctrl Pts',(-6.24361181285047,2.61592686600952,71.1765102130005));
#26908=CARTESIAN_POINT('Ctrl Pts',(-6.30972503147885,2.44533413404574,71.1851583885645));
#26909=CARTESIAN_POINT('Ctrl Pts',(-6.31671957513785,2.42728602904672,71.1860733348159));
#26910=CARTESIAN_POINT('Ctrl Pts',(-6.32363602825061,2.40920960056799,71.1869882810673));
#26911=CARTESIAN_POINT('Ctrl Pts',(-6.33047417610556,2.39110554046881,71.1879032273187));
#26912=CARTESIAN_POINT('Ctrl Pts',(-6.4020466281971,2.20161680732105,71.197479643058));
#26913=CARTESIAN_POINT('Ctrl Pts',(-6.46516290430702,2.00876335141052,71.2070560587972));
#26914=CARTESIAN_POINT('Ctrl Pts',(-6.51953438499267,1.81327339441637,71.2166324745365));
#26915=CARTESIAN_POINT('Ctrl Pts',(-6.57162171866669,1.62599597449942,71.2258065848553));
#26916=CARTESIAN_POINT('Ctrl Pts',(-6.61568378131449,1.436299258653,71.2349806951742));
#26917=CARTESIAN_POINT('Ctrl Pts',(-6.6515147912199,1.24484536476742,71.2441548054931));
#26918=CARTESIAN_POINT('Ctrl Pts',(-6.68724741901072,1.05391715070428,71.2533037262242));
#26919=CARTESIAN_POINT('Ctrl Pts',(-6.71479403405442,0.861241579233054,
71.2624526469552));
#26920=CARTESIAN_POINT('Ctrl Pts',(-6.7339988753798,0.667493929847773,71.2716015676862));
#26921=CARTESIAN_POINT('Ctrl Pts',(-6.753122924958,0.474561346353395,71.2807120003465));
#26922=CARTESIAN_POINT('Ctrl Pts',(-6.76397515626355,0.280565880181399,
71.2898224330069));
#26923=CARTESIAN_POINT('Ctrl Pts',(-6.76645108534723,0.086189962311772,
71.2989328656672));
#26924=CARTESIAN_POINT('Ctrl Pts',(-6.76680323855356,0.0585437331999436,
71.3002286491748));
#26925=CARTESIAN_POINT('Ctrl Pts',(-6.76698602565755,0.0308898307818761,
71.3015244326823));
#26926=CARTESIAN_POINT('Ctrl Pts',(-6.76699922901903,0.00323024083590044,
71.3028202161898));
#26927=CARTESIAN_POINT('Ctrl Pts',(-6.767,3.33069737261845E-12,71.3028202161898));
#26928=CARTESIAN_POINT('Ctrl Pts',(-6.76700000000009,-0.186007249412401,
71.3115697279958));
#26929=CARTESIAN_POINT('Ctrl Pts',(-6.75932637295456,-0.372014355524311,
71.3203192398017));
#26930=CARTESIAN_POINT('Ctrl Pts',(-6.74400518266954,-0.557389537151886,
71.3290687516077));
#26931=CARTESIAN_POINT('Ctrl Pts',(-6.72868405709679,-0.742763935808368,
71.3378182264582));
#26932=CARTESIAN_POINT('Ctrl Pts',(-6.70571545653032,-0.927506129692142,
71.3465677013088));
#26933=CARTESIAN_POINT('Ctrl Pts',(-6.67517739415696,-1.110988639247,71.3553171761593));
#26934=CARTESIAN_POINT('Ctrl Pts',(-6.6446394582312,-1.29447038906401,71.3640666147813));
#26935=CARTESIAN_POINT('Ctrl Pts',(-6.60653217027178,-1.47669218228127,
71.3728160534033));
#26936=CARTESIAN_POINT('Ctrl Pts',(-6.56098496116732,-1.65703510504042,
71.3815654920253));
#26937=CARTESIAN_POINT('Ctrl Pts',(-6.51543793687533,-1.83737729603968,
71.3903148951455));
#26938=CARTESIAN_POINT('Ctrl Pts',(-6.46245112202648,-2.01584035397027,
71.3990642982658));
#26939=CARTESIAN_POINT('Ctrl Pts',(-6.40220448416243,-2.19181813638142,
71.407813701386));
#26940=CARTESIAN_POINT('Ctrl Pts',(-6.34195808575187,-2.36779521935944,
71.4165630697313));
#26941=CARTESIAN_POINT('Ctrl Pts',(-6.27445201489234,-2.54128677544828,
71.4253124380765));
#26942=CARTESIAN_POINT('Ctrl Pts',(-6.19991555136183,-2.71170355237842,
71.4340618064218));
#26943=CARTESIAN_POINT('Ctrl Pts',(-6.12537937789038,-2.88211966613073,
71.4428111407189));
#26944=CARTESIAN_POINT('Ctrl Pts',(-6.04381298133617,-3.04946076210445,
71.4515604750159));
#26945=CARTESIAN_POINT('Ctrl Pts',(-5.95549339426307,-3.21315848206854,
71.460309809313));
#26946=CARTESIAN_POINT('Ctrl Pts',(-5.8671741435517,-3.37685557859619,71.4690591102885));
#26947=CARTESIAN_POINT('Ctrl Pts',(-5.77210188986257,-3.53690907467279,
71.4778084112641));
#26948=CARTESIAN_POINT('Ctrl Pts',(-5.67059953467099,-3.69277536784858,
71.4865577122396));
#26949=CARTESIAN_POINT('Ctrl Pts',(-5.56909755761795,-3.8486410803575,71.4953069806204));
#26950=CARTESIAN_POINT('Ctrl Pts',(-5.46116568338098,-4.00031938104242,
71.5040562490012));
#26951=CARTESIAN_POINT('Ctrl Pts',(-5.3471704868614,-4.14729511663185,71.5128055173819));
#26952=CARTESIAN_POINT('Ctrl Pts',(-5.23317570555527,-4.29427031688031,
71.5215547538946));
#26953=CARTESIAN_POINT('Ctrl Pts',(-5.11311782178796,-4.43654275987142,
71.5303039904072));
#26954=CARTESIAN_POINT('Ctrl Pts',(-4.98740459171984,-4.57362924147682,
71.5390532269198));
#26955=CARTESIAN_POINT('Ctrl Pts',(-4.86169180910801,-4.71071523514466,
71.547802432291));
#26956=CARTESIAN_POINT('Ctrl Pts',(-4.73032391415404,-4.8426150931655,71.5565516376621));
#26957=CARTESIAN_POINT('Ctrl Pts',(-4.59374707237268,-4.96888084331547,
71.5653008430332));
#26958=CARTESIAN_POINT('Ctrl Pts',(-4.4571707053739,-5.09514615452734,71.5740500179894));
#26959=CARTESIAN_POINT('Ctrl Pts',(-4.31538563819511,-5.2157772025363,71.5827991929456));
#26960=CARTESIAN_POINT('Ctrl Pts',(-4.16887341290665,-5.33036429028637,
71.5915483679019));
#26961=CARTESIAN_POINT('Ctrl Pts',(-4.02236168477358,-5.44495098921162,
71.6002975131698));
#26962=CARTESIAN_POINT('Ctrl Pts',(-3.87112305634461,-5.55349359238743,
71.6090466584377));
#26963=CARTESIAN_POINT('Ctrl Pts',(-3.71567117316758,-5.65562346102457,
71.6177958037056));
#26964=CARTESIAN_POINT('Ctrl Pts',(-3.56021980457321,-5.75775299158756,
71.6265449200118));
#26965=CARTESIAN_POINT('Ctrl Pts',(-3.40055544862404,-5.85346967275344,
71.6352940363179));
#26966=CARTESIAN_POINT('Ctrl Pts',(-3.23722036323414,-5.94244842803556,
71.6440431526241));
#26967=CARTESIAN_POINT('Ctrl Pts',(-3.07388580496062,-6.03142689616467,
71.652792240695));
#26968=CARTESIAN_POINT('Ctrl Pts',(-2.90688079257727,-6.11366734484813,
71.661541328766));
#26969=CARTESIAN_POINT('Ctrl Pts',(-2.7367725109464,-6.18889046787291,71.6702904168369));
#26970=CARTESIAN_POINT('Ctrl Pts',(-2.56666476416692,-6.2641133543825,71.6790394773992));
#26971=CARTESIAN_POINT('Ctrl Pts',(-2.39345402972164,-6.33231884350263,
71.6877885379614));
#26972=CARTESIAN_POINT('Ctrl Pts',(-2.21772856474133,-6.3932752962101,71.6965375985236));
#26973=CARTESIAN_POINT('Ctrl Pts',(-2.04200363768374,-6.45423156232048,
71.7052866323036));
#26974=CARTESIAN_POINT('Ctrl Pts',(-1.86376426620208,-6.50793874252023,
71.7140356660836));
#26975=CARTESIAN_POINT('Ctrl Pts',(-1.68361578194813,-6.55421443796091,
71.7227846998636));
#26976=CARTESIAN_POINT('Ctrl Pts',(-1.50346783420031,-6.60048999558641,
71.7315337075878));
#26977=CARTESIAN_POINT('Ctrl Pts',(-1.32141106257449,-6.63933404145454,
71.740282715312));
#26978=CARTESIAN_POINT('Ctrl Pts',(-1.13806375959286,-6.67061465526989,
71.7490317230362));
#26979=CARTESIAN_POINT('Ctrl Pts',(-0.954716987421707,-6.70189517852444,
71.7577807054311));
#26980=CARTESIAN_POINT('Ctrl Pts',(-0.770079973812568,-6.72561226535797,
71.766529687826));
#26981=CARTESIAN_POINT('Ctrl Pts',(-0.584779770555288,-6.74168536939758,
71.7752786702208));
#26982=CARTESIAN_POINT('Ctrl Pts',(-0.391490647556741,-6.75845143942377,
71.7844048508969));
#26983=CARTESIAN_POINT('Ctrl Pts',(-0.197480213107163,-6.76689975924018,
71.793531031573));
#26984=CARTESIAN_POINT('Ctrl Pts',(-0.00346532630061558,-6.76699911271707,
71.802657212249));
#26985=CARTESIAN_POINT('Ctrl Pts',(0.184486595293259,-6.76709536139781,
71.8114981997789));
#26986=CARTESIAN_POINT('Ctrl Pts',(0.37244237818246,-6.75935659726785,71.8203391873089));
#26987=CARTESIAN_POINT('Ctrl Pts',(0.559750217719346,-6.74380965729039,
71.8291801748388));
#26988=CARTESIAN_POINT('Ctrl Pts',(0.745129914455018,-6.72842275717284,
71.8379301534366));
#26989=CARTESIAN_POINT('Ctrl Pts',(0.929874656311454,-6.70538772273511,
71.8466801320343));
#26990=CARTESIAN_POINT('Ctrl Pts',(1.11335688289505,-6.67478280180788,71.8554301106321));
#26991=CARTESIAN_POINT('Ctrl Pts',(1.29683723118585,-6.64417819418076,71.864179999657));
#26992=CARTESIAN_POINT('Ctrl Pts',(1.47905480729965,-6.60600390230136,71.872929888682));
#26993=CARTESIAN_POINT('Ctrl Pts',(1.65939064804539,-6.56038959797202,71.8816797777069));
#26994=CARTESIAN_POINT('Ctrl Pts',(1.83972470263996,-6.51477574543332,71.8904295800679));
#26995=CARTESIAN_POINT('Ctrl Pts',(2.0181767812558,-6.46172209820184,71.8991793824288));
#26996=CARTESIAN_POINT('Ctrl Pts',(2.19414072347413,-6.40140886724106,71.9079291847898));
#26997=CARTESIAN_POINT('Ctrl Pts',(2.37010298131828,-6.34109621361475,71.9166789033952));
#26998=CARTESIAN_POINT('Ctrl Pts',(2.54357687926641,-6.27352420826081,71.9254286220007));
#26999=CARTESIAN_POINT('Ctrl Pts',(2.71397317789698,-6.19892237325616,71.9341783406062));
#27000=CARTESIAN_POINT('Ctrl Pts',(2.88436790206936,-6.12432122757089,71.9429279783645));
#27001=CARTESIAN_POINT('Ctrl Pts',(3.05168482125999,-6.04269049717547,71.9516776161228));
#27002=CARTESIAN_POINT('Ctrl Pts',(3.21535561997139,-5.95430745235064,71.960427253881));
#27003=CARTESIAN_POINT('Ctrl Pts',(3.37902496075022,-5.86592519481665,71.9691768137));
#27004=CARTESIAN_POINT('Ctrl Pts',(3.53904799384609,-5.77079087940395,71.977926373519));
#27005=CARTESIAN_POINT('Ctrl Pts',(3.69488118814711,-5.66922763747202,71.986675933338));
#27006=CARTESIAN_POINT('Ctrl Pts',(3.85071304610566,-5.56766526649236,71.9954254181255));
#27007=CARTESIAN_POINT('Ctrl Pts',(4.00235489705708,-5.45967423580904,72.0041749029129));
#27008=CARTESIAN_POINT('Ctrl Pts',(4.14929168607401,-5.34562133936525,72.0129243877004));
#27009=CARTESIAN_POINT('Ctrl Pts',(4.296227263855,-5.23156938308742,72.0216738003636));
#27010=CARTESIAN_POINT('Ctrl Pts',(4.43845763091806,-5.11145583677428,72.0304232130269));
#27011=CARTESIAN_POINT('Ctrl Pts',(4.57549970660699,-4.98568866204453,72.0391726256902));
#27012=CARTESIAN_POINT('Ctrl Pts',(4.71254069815041,-4.85992248226408,72.0479219691366));
#27013=CARTESIAN_POINT('Ctrl Pts',(4.84439326931069,-4.72850295734253,72.0566713125829));
#27014=CARTESIAN_POINT('Ctrl Pts',(4.97060959434462,-4.59187644221937,72.0654206560292));
#27015=CARTESIAN_POINT('Ctrl Pts',(5.09682496280291,-4.45525096256921,72.0741699331655));
#27016=CARTESIAN_POINT('Ctrl Pts',(5.21740397615626,-4.31341878218583,72.0829192103018));
#27017=CARTESIAN_POINT('Ctrl Pts',(5.33193710451733,-4.16686161438935,72.0916684874381));
#27018=CARTESIAN_POINT('Ctrl Pts',(5.44646940289189,-4.02030550864777,72.1004177011711));
#27019=CARTESIAN_POINT('Ctrl Pts',(5.55495572749479,-3.86902470980401,72.1091669149041));
#27020=CARTESIAN_POINT('Ctrl Pts',(5.65702762491277,-3.71353301466054,72.117916128637));
#27021=CARTESIAN_POINT('Ctrl Pts',(5.75909881654984,-3.55804239467168,72.1266652818731));
#27022=CARTESIAN_POINT('Ctrl Pts',(5.85475551250622,-3.3983411761983,72.1354144351092));
#27023=CARTESIAN_POINT('Ctrl Pts',(5.94367283727943,-3.23497174692248,72.1441635883454));
#27024=CARTESIAN_POINT('Ctrl Pts',(6.03258957676172,-3.0716033930124,72.1529126839909));
#27025=CARTESIAN_POINT('Ctrl Pts',(6.11476689685157,-2.90456712829772,72.1616617796364));
#27026=CARTESIAN_POINT('Ctrl Pts',(6.18992570525145,-2.73443024476167,72.170410875282));
#27027=CARTESIAN_POINT('Ctrl Pts',(6.26508404388594,-2.56429442463283,72.179159916243));
#27028=CARTESIAN_POINT('Ctrl Pts',(6.33322384283223,-2.39105828656237,72.187908957204));
#27029=CARTESIAN_POINT('Ctrl Pts',(6.39411368719952,-2.21531017132315,72.1966579981651));
#27030=CARTESIAN_POINT('Ctrl Pts',(6.4550031712082,-2.03956309619737,72.2054069873475));
#27031=CARTESIAN_POINT('Ctrl Pts',(6.50864269270014,-1.86130434438842,72.2141559765299));
#27032=CARTESIAN_POINT('Ctrl Pts',(6.55485008446284,-1.6811393072014,72.2229049657123));
#27033=CARTESIAN_POINT('Ctrl Pts',(6.60199664749361,-1.49731239212031,72.2318317792417));
#27034=CARTESIAN_POINT('Ctrl Pts',(6.6414056364087,-1.31150116499858,72.2407585927711));
#27035=CARTESIAN_POINT('Ctrl Pts',(6.67293772282141,-1.12436255155843,72.2496854063004));
#27036=CARTESIAN_POINT('Ctrl Pts',(6.70384494949845,-0.94093239505318,72.258435320456));
#27037=CARTESIAN_POINT('Ctrl Pts',(6.7271844934891,-0.756227260508556,72.2671852346115));
#27038=CARTESIAN_POINT('Ctrl Pts',(6.74287707373917,-0.570874564543536,
72.275935148767));
#27039=CARTESIAN_POINT('Ctrl Pts',(6.7585693453866,-0.385525513634342,72.284684890851));
#27040=CARTESIAN_POINT('Ctrl Pts',(6.76661493004097,-0.199529212420115,
72.293434632935));
#27041=CARTESIAN_POINT('Ctrl Pts',(6.76698649908906,-0.0135174386023319,
72.3021843750189));
#27042=CARTESIAN_POINT('Ctrl Pts',(6.76735806132394,0.17249092444395,72.3109339566648));
#27043=CARTESIAN_POINT('Ctrl Pts',(6.76005588896299,0.358514472899656,72.3196835383107));
#27044=CARTESIAN_POINT('Ctrl Pts',(6.74510478454598,0.543921359660541,72.3284331199566));
#27045=CARTESIAN_POINT('Ctrl Pts',(6.73015393440705,0.729325093148832,72.3371825527957));
#27046=CARTESIAN_POINT('Ctrl Pts',(6.70755443556919,0.914111900254797,72.3459319856347));
#27047=CARTESIAN_POINT('Ctrl Pts',(6.67738304682343,1.09765415591389,72.3546814184738));
#27048=CARTESIAN_POINT('Ctrl Pts',(6.6472121311189,1.28119353391119,72.3634307141351));
#27049=CARTESIAN_POINT('Ctrl Pts',(6.60946960955529,1.46348811672496,72.3721800097964));
#27050=CARTESIAN_POINT('Ctrl Pts',(6.56428366991223,1.64391876348061,72.3809293054577));
#27051=CARTESIAN_POINT('Ctrl Pts',(6.51909837867761,1.82434682109559,72.3896784755686));
#27052=CARTESIAN_POINT('Ctrl Pts',(6.46646995271968,2.00291071820293,72.3984276456794));
#27053=CARTESIAN_POINT('Ctrl Pts',(6.40657713281599,2.17900400212557,72.4071768157902));
#27054=CARTESIAN_POINT('Ctrl Pts',(6.34668509279116,2.35509499309505,72.415925871976));
#27055=CARTESIAN_POINT('Ctrl Pts',(6.27952894037589,2.52871516397964,72.4246749281618));
#27056=CARTESIAN_POINT('Ctrl Pts',(6.20533675061518,2.69927486771257,72.4334239843475));
#27057=CARTESIAN_POINT('Ctrl Pts',(6.12832117907992,2.87632521635763,72.4425059856298));
#27058=CARTESIAN_POINT('Ctrl Pts',(6.04372366626158,3.05007728919841,72.4515879869121));
#27059=CARTESIAN_POINT('Ctrl Pts',(5.95185378007951,3.21989527478043,72.4606699881944));
#27060=CARTESIAN_POINT('Ctrl Pts',(5.86334450817457,3.38350129286602,72.4694197685015));
#27061=CARTESIAN_POINT('Ctrl Pts',(5.76808562057345,3.54345567124816,72.4781695488086));
#27062=CARTESIAN_POINT('Ctrl Pts',(5.66640068804577,3.69921508465167,72.4869193291157));
#27063=CARTESIAN_POINT('Ctrl Pts',(5.5647194110802,3.85496889852143,72.4956687948692));
#27064=CARTESIAN_POINT('Ctrl Pts',(5.45661270815215,4.00652780919499,72.5044182606227));
#27065=CARTESIAN_POINT('Ctrl Pts',(5.34244776449219,4.15337704569094,72.5131677263762));
#27066=CARTESIAN_POINT('Ctrl Pts',(5.22828631819701,4.30022178356121,72.5219169240958));
#27067=CARTESIAN_POINT('Ctrl Pts',(5.10806717844175,4.44235690972558,72.5306661218154));
#27068=CARTESIAN_POINT('Ctrl Pts',(4.98219864544825,4.5792996907053,72.539415319535));
#27069=CARTESIAN_POINT('Ctrl Pts',(4.85633329944131,4.71623900429892,72.5481642957252));
#27070=CARTESIAN_POINT('Ctrl Pts',(4.72481904033754,4.84798602483514,72.5569132719154));
#27071=CARTESIAN_POINT('Ctrl Pts',(4.58810250737304,4.97409332259029,72.5656622481057));
#27072=CARTESIAN_POINT('Ctrl Pts',(4.45137708685749,5.10020881822042,72.5744117930419));
#27073=CARTESIAN_POINT('Ctrl Pts',(4.3094489263616,5.22068366307843,72.583161337978));
#27074=CARTESIAN_POINT('Ctrl Pts',(4.16280009466772,5.33510865604764,72.5919108829142));
#27075=CARTESIAN_POINT('Ctrl Pts',(4.01615988348899,5.44952692272811,72.6006599135225));
#27076=CARTESIAN_POINT('Ctrl Pts',(3.8647997823234,5.55789587288551,72.6094089441308));
#27077=CARTESIAN_POINT('Ctrl Pts',(3.70923383581175,5.65984746713807,72.6181579747391));
#27078=CARTESIAN_POINT('Ctrl Pts',(3.55366577799648,5.76180044505317,72.6269071240871));
#27079=CARTESIAN_POINT('Ctrl Pts',(3.39389200026947,5.85733573570998,72.6356562734351));
#27080=CARTESIAN_POINT('Ctrl Pts',(3.23045513626147,5.94612887621871,72.6444054227831));
#27081=CARTESIAN_POINT('Ctrl Pts',(3.1869512215165,5.9697639920665,72.6467342868961));
#27082=CARTESIAN_POINT('Ctrl Pts',(3.14318791262702,5.99292165435313,72.6490631510091));
#27083=CARTESIAN_POINT('Ctrl Pts',(3.09917575053262,6.01559628526637,72.6513920151221));
#27084=CARTESIAN_POINT('Origin',(0.,0.,-3.69717978381041));
#27085=CARTESIAN_POINT('',(3.09917575053257,6.0155962852664,75.0456602561759));
#27086=CARTESIAN_POINT('',(3.09917575053252,6.01559628526642,74.65129258962));
#27087=CARTESIAN_POINT('',(3.09917575053259,6.01559628526639,-3.69717978381041));
#27088=CARTESIAN_POINT('',(-6.76699811314402,-0.00505338552136531,73.6971797838396));
#27089=CARTESIAN_POINT('Ctrl Pts',(-6.76699811314402,-0.00505338552137147,
73.6971797838396));
#27090=CARTESIAN_POINT('Ctrl Pts',(-6.76684798857142,-0.206085484741003,
73.7066067669995));
#27091=CARTESIAN_POINT('Ctrl Pts',(-6.75773564685474,-0.40676139421809,
73.7160337501595));
#27092=CARTESIAN_POINT('Ctrl Pts',(-6.7397798239725,-0.606347197876985,
73.7254607333194));
#27093=CARTESIAN_POINT('Ctrl Pts',(-6.72173924480955,-0.806875099846274,
73.7349322143582));
#27094=CARTESIAN_POINT('Ctrl Pts',(-6.69477160047039,-1.00630246036111,
73.7444036953969));
#27095=CARTESIAN_POINT('Ctrl Pts',(-6.65904688194988,-1.20390349446855,
73.7538751764357));
#27096=CARTESIAN_POINT('Ctrl Pts',(-6.62310148542693,-1.40272514565269,
73.7634051645139));
#27097=CARTESIAN_POINT('Ctrl Pts',(-6.57829056854179,-1.59969771800889,
73.7729351525921));
#27098=CARTESIAN_POINT('Ctrl Pts',(-6.52483603914106,-1.79410246706424,
73.7824651406703));
#27099=CARTESIAN_POINT('Ctrl Pts',(-6.48144530150877,-1.95190697035518,
73.7902009343809));
#27100=CARTESIAN_POINT('Ctrl Pts',(-6.43236015357818,-2.1080198794279,73.7979367280915));
#27101=CARTESIAN_POINT('Ctrl Pts',(-6.37772216023483,-2.2620674275648,73.8056725218021));
#27102=CARTESIAN_POINT('Ctrl Pts',(-6.31963014829381,-2.4258533109448,73.813897344734));
#27103=CARTESIAN_POINT('Ctrl Pts',(-6.25514327880184,-2.58762986612481,
73.822122167666));
#27104=CARTESIAN_POINT('Ctrl Pts',(-6.18441902472954,-2.74686190525904,
73.830346990598));
#27105=CARTESIAN_POINT('Ctrl Pts',(-6.11377442809694,-2.9059145997438,73.8385625498291));
#27106=CARTESIAN_POINT('Ctrl Pts',(-6.03690658021127,-3.06242816004967,
73.8467781090602));
#27107=CARTESIAN_POINT('Ctrl Pts',(-5.95402242007101,-3.21588339671882,
73.8549936682913));
#27108=CARTESIAN_POINT('Ctrl Pts',(-5.87121495973981,-3.36919662812023,
73.8632016249621));
#27109=CARTESIAN_POINT('Ctrl Pts',(-5.78240244418765,-3.51945685846059,
73.8714095816328));
#27110=CARTESIAN_POINT('Ctrl Pts',(-5.68783953845758,-3.6661656242945,73.8796175383036));
#27111=CARTESIAN_POINT('Ctrl Pts',(-5.59334514600925,-3.81276809581638,
73.8878195480966));
#27112=CARTESIAN_POINT('Ctrl Pts',(-5.49310885546529,-3.95582392768004,
73.8960215578896));
#27113=CARTESIAN_POINT('Ctrl Pts',(-5.38743085978608,-4.09485991592199,
73.9042235676825));
#27114=CARTESIAN_POINT('Ctrl Pts',(-5.28180820900181,-4.2338230892689,73.9124212819799));
#27115=CARTESIAN_POINT('Ctrl Pts',(-5.17074974710591,-4.36877032801805,
73.9206189962772));
#27116=CARTESIAN_POINT('Ctrl Pts',(-5.05459856036554,-4.4992579825512,73.9288167105745));
#27117=CARTESIAN_POINT('Ctrl Pts',(-4.93846946939272,-4.62972081405012,
73.9370128653975));
#27118=CARTESIAN_POINT('Ctrl Pts',(-4.81724981695655,-4.75572547929968,
73.9452090202206));
#27119=CARTESIAN_POINT('Ctrl Pts',(-4.69132269250438,-4.87686173628015,
73.9534051750436));
#27120=CARTESIAN_POINT('Ctrl Pts',(-4.56540484558621,-4.9979890686882,73.9616007260245));
#27121=CARTESIAN_POINT('Ctrl Pts',(-4.4347804753286,-5.11424845772864,73.9697962770053));
#27122=CARTESIAN_POINT('Ctrl Pts',(-4.29986917423884,-5.22526689121529,
73.9779918279862));
#27123=CARTESIAN_POINT('Ctrl Pts',(-4.16494326651792,-5.33629734449046,
73.9861882662863));
#27124=CARTESIAN_POINT('Ctrl Pts',(-4.02572978039465,-5.44208548366305,
73.9943847045864));
#27125=CARTESIAN_POINT('Ctrl Pts',(-3.88268102096551,-5.54229889932276,
74.0025811428865));
#27126=CARTESIAN_POINT('Ctrl Pts',(-3.73959074715509,-5.6425413980585,74.0107799598865));
#27127=CARTESIAN_POINT('Ctrl Pts',(-3.59266327682294,-5.73720574489927,
74.0189787768865));
#27128=CARTESIAN_POINT('Ctrl Pts',(-3.44237951929786,-5.82600311063414,
74.0271775938864));
#27129=CARTESIAN_POINT('Ctrl Pts',(-3.29193870951321,-5.9148932730036,74.0353849789629));
#27130=CARTESIAN_POINT('Ctrl Pts',(-3.13813491446167,-5.99790402210956,
74.0435923640394));
#27131=CARTESIAN_POINT('Ctrl Pts',(-2.98147413730228,-6.07479225723791,
74.0517997491159));
#27132=CARTESIAN_POINT('Ctrl Pts',(-2.82472940140128,-6.15172169884808,
74.0600115327517));
#27133=CARTESIAN_POINT('Ctrl Pts',(-2.66512495873763,-6.22252193992118,
74.0682233163875));
#27134=CARTESIAN_POINT('Ctrl Pts',(-2.50318627035949,-6.28699828979488,
74.0764351000234));
#27135=CARTESIAN_POINT('Ctrl Pts',(-2.34100910679523,-6.35156958924296,
74.0846589765485));
#27136=CARTESIAN_POINT('Ctrl Pts',(-2.17649116610084,-6.40979826653793,
74.0928828530736));
#27137=CARTESIAN_POINT('Ctrl Pts',(-2.01017376801462,-6.46153932297761,
74.1011067295988));
#27138=CARTESIAN_POINT('Ctrl Pts',(-1.85649201112722,-6.5093494531766,74.1087058130822));
#27139=CARTESIAN_POINT('Ctrl Pts',(-1.7012741896522,-6.55162078995792,74.1163048965656));
#27140=CARTESIAN_POINT('Ctrl Pts',(-1.54495370933529,-6.58827800233196,
74.1239039800491));
#27141=CARTESIAN_POINT('Ctrl Pts',(-1.37727264099333,-6.62759927693945,
74.1320553267846));
#27142=CARTESIAN_POINT('Ctrl Pts',(-1.20782614281645,-6.66057652599887,
74.1402066735201));
#27143=CARTESIAN_POINT('Ctrl Pts',(-1.03713977751074,-6.68704943019752,
74.1483580202556));
#27144=CARTESIAN_POINT('Ctrl Pts',(-0.866651660399433,-6.71349158674127,
74.1564998993938));
#27145=CARTESIAN_POINT('Ctrl Pts',(-0.694926900390888,-6.73344438107405,
74.164641778532));
#27146=CARTESIAN_POINT('Ctrl Pts',(-0.522504970112164,-6.74679757782966,
74.1727836576702));
#27147=CARTESIAN_POINT('Ctrl Pts',(-0.350247027367419,-6.76013807458936,
74.1809177932071));
#27148=CARTESIAN_POINT('Ctrl Pts',(-0.177293596488486,-6.76689144186465,
74.1890519287439));
#27149=CARTESIAN_POINT('Ctrl Pts',(-0.00419306548881221,-6.76699870091622,
74.1971860642808));
#27150=CARTESIAN_POINT('Ctrl Pts',(0.168779231809186,-6.76710588050977,
74.2053141740112));
#27151=CARTESIAN_POINT('Ctrl Pts',(0.341898048117475,-6.76057675506325,
74.2134422837416));
#27152=CARTESIAN_POINT('Ctrl Pts',(0.514611168556591,-6.74740426721245,
74.221570393472));
#27153=CARTESIAN_POINT('Ctrl Pts',(0.687232646626987,-6.73423876874374,
74.2296941903903));
#27154=CARTESIAN_POINT('Ctrl Pts',(0.85944849372861,-6.71443695573693,74.2378179873086));
#27155=CARTESIAN_POINT('Ctrl Pts',(1.03070779855958,-6.68804384211022,74.2459417842269));
#27156=CARTESIAN_POINT('Ctrl Pts',(1.20304095111717,-6.66148523566493,74.2541165198131));
#27157=CARTESIAN_POINT('Ctrl Pts',(1.37440514971835,-6.62825239333862,74.2622912553993));
#27158=CARTESIAN_POINT('Ctrl Pts',(1.54424509702084,-6.588444131988,74.2704659909855));
#27159=CARTESIAN_POINT('Ctrl Pts',(1.71298839852233,-6.5488929100639,74.2785879428209));
#27160=CARTESIAN_POINT('Ctrl Pts',(1.88022672055067,-6.50285104346772,74.2867098946563));
#27161=CARTESIAN_POINT('Ctrl Pts',(2.04542682387103,-6.45046650314447,74.2948318464917));
#27162=CARTESIAN_POINT('Ctrl Pts',(2.21064871158063,-6.39807505504579,74.3029548693419));
#27163=CARTESIAN_POINT('Ctrl Pts',(2.37383149636435,-6.33933937790731,74.3110778921922));
#27164=CARTESIAN_POINT('Ctrl Pts',(2.53445836165528,-6.27445693371432,74.3192009150424));
#27165=CARTESIAN_POINT('Ctrl Pts',(2.69513699027794,-6.20955358061871,74.3273265556037));
#27166=CARTESIAN_POINT('Ctrl Pts',(2.85325772009297,-6.13849965297926,74.335452196165));
#27167=CARTESIAN_POINT('Ctrl Pts',(3.00832497268535,-6.06154022165305,74.3435778367264));
#27168=CARTESIAN_POINT('Ctrl Pts',(3.16506191321886,-5.98375212900542,74.3517909701905));
#27169=CARTESIAN_POINT('Ctrl Pts',(3.31867889515768,-5.89993079157754,74.3600041036546));
#27170=CARTESIAN_POINT('Ctrl Pts',(3.46869173861445,-5.81037577291416,74.3682172371187));
#27171=CARTESIAN_POINT('Ctrl Pts',(3.61736322108309,-5.72162152307537,74.3763569316921));
#27172=CARTESIAN_POINT('Ctrl Pts',(3.76249448685049,-5.62723596626766,74.3844966262655));
#27173=CARTESIAN_POINT('Ctrl Pts',(3.90364563443486,-5.52755278226791,74.3926363208389));
#27174=CARTESIAN_POINT('Ctrl Pts',(4.0467070472529,-5.42652053859676,74.4008861737484));
#27175=CARTESIAN_POINT('Ctrl Pts',(4.18567953042559,-5.32004648992106,74.4091360266578));
#27176=CARTESIAN_POINT('Ctrl Pts',(4.32014216904989,-5.20851808475279,74.4173858795673));
#27177=CARTESIAN_POINT('Ctrl Pts',(4.45460480767419,-5.09698967958453,74.4256357324768));
#27178=CARTESIAN_POINT('Ctrl Pts',(4.58455736100398,-4.98040722385045,74.4338855853863));
#27179=CARTESIAN_POINT('Ctrl Pts',(4.70962011429032,-4.85919410798458,74.4421354382958));
#27180=CARTESIAN_POINT('Ctrl Pts',(4.83439740687436,-4.73825766587068,74.4503664605883));
#27181=CARTESIAN_POINT('Ctrl Pts',(4.95469679166588,-4.61233432069282,74.4585974828808));
#27182=CARTESIAN_POINT('Ctrl Pts',(5.07009529176753,-4.48178789462383,74.4668285051733));
#27183=CARTESIAN_POINT('Ctrl Pts',(5.18535602745416,-4.35139731678514,74.4750497011512));
#27184=CARTESIAN_POINT('Ctrl Pts',(5.29572729358617,-4.21639491369581,74.4832708971291));
#27185=CARTESIAN_POINT('Ctrl Pts',(5.40082100489027,-4.07718303159622,74.4914920931069));
#27186=CARTESIAN_POINT('Ctrl Pts',(5.50581032135212,-3.93810943562516,74.4997051225594));
#27187=CARTESIAN_POINT('Ctrl Pts',(5.60553230885063,-3.79483497208888,74.507918152012));
#27188=CARTESIAN_POINT('Ctrl Pts',(5.69963736852876,-3.64779698822051,74.5161311814645));
#27189=CARTESIAN_POINT('Ctrl Pts',(5.79366780682141,-3.50087559933768,74.5243376983274));
#27190=CARTESIAN_POINT('Ctrl Pts',(5.88208999633018,-3.3501969347092,74.5325442151903));
#27191=CARTESIAN_POINT('Ctrl Pts',(5.96459605500922,-3.1962294818377,74.5407507320531));
#27192=CARTESIAN_POINT('Ctrl Pts',(6.04705321906005,-3.04235327294858,74.5489523855812));
#27193=CARTESIAN_POINT('Ctrl Pts',(6.12360106782642,-2.88519247348388,74.5571540391092));
#27194=CARTESIAN_POINT('Ctrl Pts',(6.19397627050322,-2.72524255075453,74.5653556926372));
#27195=CARTESIAN_POINT('Ctrl Pts',(6.26433055714531,-2.56534016633423,74.5735549085727));
#27196=CARTESIAN_POINT('Ctrl Pts',(6.328515704314,-2.40265063592481,74.5817541245082));
#27197=CARTESIAN_POINT('Ctrl Pts',(6.38631528380104,-2.23769213608334,74.5899533404436));
#27198=CARTESIAN_POINT('Ctrl Pts',(6.44410682728185,-2.07275657079511,74.5981514164236));
#27199=CARTESIAN_POINT('Ctrl Pts',(6.49551445196764,-1.90555300229453,74.6063494924035));
#27200=CARTESIAN_POINT('Ctrl Pts',(6.54037064899189,-1.73661762452344,74.6145475683835));
#27201=CARTESIAN_POINT('Ctrl Pts',(6.58522875098158,-1.56767507235778,74.6227459925216));
#27202=CARTESIAN_POINT('Ctrl Pts',(6.62353477893024,-1.39700091089266,74.6309444166597));
#27203=CARTESIAN_POINT('Ctrl Pts',(6.65517166661411,-1.22514451714757,74.6391428407978));
#27204=CARTESIAN_POINT('Ctrl Pts',(6.68681563995494,-1.05324963303441,74.6473431011223));
#27205=CARTESIAN_POINT('Ctrl Pts',(6.71178743317195,-0.880172341777026,
74.6555433614467));
#27206=CARTESIAN_POINT('Ctrl Pts',(6.73002145600003,-0.706470241255208,
74.6637436217712));
#27207=CARTESIAN_POINT('Ctrl Pts',(6.74827260585864,-0.532604984132883,
74.671951584516));
#27208=CARTESIAN_POINT('Ctrl Pts',(6.75977330347216,-0.358114102214749,
74.6801595472608));
#27209=CARTESIAN_POINT('Ctrl Pts',(6.76450995960047,-0.183559272351012,
74.6883675100057));
#27210=CARTESIAN_POINT('Ctrl Pts',(6.76924888186432,-0.00892093106215111,
74.6965793996465));
#27211=CARTESIAN_POINT('Ctrl Pts',(6.76721731464129,0.165781060886628,74.7047912892873));
#27212=CARTESIAN_POINT('Ctrl Pts',(6.75845380030758,0.339987101384871,74.7130031789282));
#27213=CARTESIAN_POINT('Ctrl Pts',(6.74967823927898,0.514432612823238,74.7212263569774));
#27214=CARTESIAN_POINT('Ctrl Pts',(6.73415226842231,0.688380453082736,74.7294495350267));
#27215=CARTESIAN_POINT('Ctrl Pts',(6.71196625382715,0.861276963285036,74.737672713076));
#27216=CARTESIAN_POINT('Ctrl Pts',(6.69155672835339,1.02032922182219,74.7452374408982));
#27217=CARTESIAN_POINT('Ctrl Pts',(6.66551165699124,1.17849166295503,74.7528021687204));
#27218=CARTESIAN_POINT('Ctrl Pts',(6.63393905664814,1.33534324901066,74.7603668965425));
#27219=CARTESIAN_POINT('Ctrl Pts',(6.59784581407433,1.514653229249,74.7690147606185));
#27220=CARTESIAN_POINT('Ctrl Pts',(6.55444614030209,1.69265943061418,74.7776626246944));
#27221=CARTESIAN_POINT('Ctrl Pts',(6.50384734659557,1.86875859655059,74.7863104887704));
#27222=CARTESIAN_POINT('Ctrl Pts',(6.45331376152844,2.04463081662196,74.7949472080065));
#27223=CARTESIAN_POINT('Ctrl Pts',(6.39559964071816,2.21860061058749,74.8035839272427));
#27224=CARTESIAN_POINT('Ctrl Pts',(6.33086315836925,2.39007545278449,74.8122206464788));
#27225=CARTESIAN_POINT('Ctrl Pts',(6.26386469293625,2.56754186539624,74.8211591447444));
#27226=CARTESIAN_POINT('Ctrl Pts',(6.1893442944921,2.74233550284023,74.83009764301));
#27227=CARTESIAN_POINT('Ctrl Pts',(6.10753435341912,2.91381418793396,74.8390361412756));
#27228=CARTESIAN_POINT('Ctrl Pts',(6.02870710322883,3.07904096887162,74.8476487527733));
#27229=CARTESIAN_POINT('Ctrl Pts',(5.9431125609327,3.24118991098983,74.856261364271));
#27230=CARTESIAN_POINT('Ctrl Pts',(5.85100847465207,3.39970422677469,74.8648739757687));
#27231=CARTESIAN_POINT('Ctrl Pts',(5.75899218745423,3.55806743730355,74.8734783772138));
#27232=CARTESIAN_POINT('Ctrl Pts',(5.66047888052456,3.71280266671292,74.8820827786589));
#27233=CARTESIAN_POINT('Ctrl Pts',(5.55577284468835,3.86337638578272,74.890687180104));
#27234=CARTESIAN_POINT('Ctrl Pts',(5.45118572917823,4.01377909010987,74.8992818090635));
#27235=CARTESIAN_POINT('Ctrl Pts',(5.34042008979548,4.16002946362168,74.907876438023));
#27236=CARTESIAN_POINT('Ctrl Pts',(5.22382438185899,4.30162153466521,74.9164710669825));
#27237=CARTESIAN_POINT('Ctrl Pts',(5.21020600002388,4.31815949238614,74.917474919877));
#27238=CARTESIAN_POINT('Ctrl Pts',(5.19650813218543,4.33463393194399,74.9184787727716));
#27239=CARTESIAN_POINT('Ctrl Pts',(5.18273137234608,4.35104407264507,74.9194826256661));
#27240=CARTESIAN_POINT('Ctrl Pts',(5.0648095340086,4.49150626995506,74.9280750799241));
#27241=CARTESIAN_POINT('Ctrl Pts',(4.9412437964944,4.62708890396287,74.9366675341821));
#27242=CARTESIAN_POINT('Ctrl Pts',(4.81246774574751,4.7573567446787,74.9452599884402));
#27243=CARTESIAN_POINT('Ctrl Pts',(4.68348043585812,4.887838291842,74.9538665387549));
#27244=CARTESIAN_POINT('Ctrl Pts',(4.5492659386127,5.01298739568452,74.9624730890697));
#27245=CARTESIAN_POINT('Ctrl Pts',(4.41029378809865,5.1324066189906,74.9710796393844));
#27246=CARTESIAN_POINT('Ctrl Pts',(4.27120756351748,5.25192386651551,74.9796932543103));
#27247=CARTESIAN_POINT('Ctrl Pts',(4.1273561282961,5.36570165351677,74.9883068692362));
#27248=CARTESIAN_POINT('Ctrl Pts',(3.97924031196239,5.47338428576447,74.996920484162));
#27249=CARTESIAN_POINT('Ctrl Pts',(3.83087972288424,5.58124487181938,75.0055483337471));
#27250=CARTESIAN_POINT('Ctrl Pts',(3.67824091424832,5.68298998936973,75.0141761833322));
#27251=CARTESIAN_POINT('Ctrl Pts',(3.52185349553243,5.77830744734182,75.0228040329172));
#27252=CARTESIAN_POINT('Ctrl Pts',(3.38375706251097,5.86247662833286,75.0304227740035));
#27253=CARTESIAN_POINT('Ctrl Pts',(3.24273811510174,5.94163437395071,75.0380415150897));
#27254=CARTESIAN_POINT('Ctrl Pts',(3.09917575053257,6.0155962852664,75.0456602561759));
#27255=CARTESIAN_POINT('Ctrl Pts',(3.09917575053266,6.01559628526635,73.0456387728543));
#27256=CARTESIAN_POINT('Ctrl Pts',(2.9438003872764,6.0956441367509,73.0538420919943));
#27257=CARTESIAN_POINT('Ctrl Pts',(2.78538097620002,6.16963789028042,73.0620454111343));
#27258=CARTESIAN_POINT('Ctrl Pts',(2.62443417564996,6.23735795491012,73.0702487302742));
#27259=CARTESIAN_POINT('Ctrl Pts',(2.46263547823033,6.30543646413684,73.0784954698604));
#27260=CARTESIAN_POINT('Ctrl Pts',(2.29828289869186,6.36717454230061,73.0867422094466));
#27261=CARTESIAN_POINT('Ctrl Pts',(2.13191836530622,6.42239932452585,73.0949889490328));
#27262=CARTESIAN_POINT('Ctrl Pts',(1.96614521010812,6.47742779849382,73.1032063738257));
#27263=CARTESIAN_POINT('Ctrl Pts',(1.79837474182039,6.52598916190316,73.1114237986185));
#27264=CARTESIAN_POINT('Ctrl Pts',(1.62915472964356,6.56796344896042,73.1196412234114));
#27265=CARTESIAN_POINT('Ctrl Pts',(1.45902920573916,6.61016234425814,73.1279026203942));
#27266=CARTESIAN_POINT('Ctrl Pts',(1.28743894176949,6.64570340328322,73.1361640173771));
#27267=CARTESIAN_POINT('Ctrl Pts',(1.11494689210193,6.6745173928751,73.1444254143599));
#27268=CARTESIAN_POINT('Ctrl Pts',(0.942454842434423,6.70333138246697,73.1526868113428));
#27269=CARTESIAN_POINT('Ctrl Pts',(0.769061373292736,6.72541831514887,73.1609482083256));
#27270=CARTESIAN_POINT('Ctrl Pts',(0.595330304088778,6.7407618878754,73.1692096053084));
#27271=CARTESIAN_POINT('Ctrl Pts',(0.423858878567678,6.75590589349317,73.1773635499306));
#27272=CARTESIAN_POINT('Ctrl Pts',(0.251528364636971,6.76452759997373,73.1855174945528));
#27273=CARTESIAN_POINT('Ctrl Pts',(0.0788809832144273,6.76654023785325,
73.193671439175));
#27274=CARTESIAN_POINT('Ctrl Pts',(-0.0935557238406468,6.76855041979508,
73.2018154338801));
#27275=CARTESIAN_POINT('Ctrl Pts',(-0.266308167148405,6.76396758206107,
73.2099594285852));
#27276=CARTESIAN_POINT('Ctrl Pts',(-0.438827156451265,6.75275645397944,
73.2181034232904));
#27277=CARTESIAN_POINT('Ctrl Pts',(-0.611171938803255,6.74155664671789,
73.2262391943183));
#27278=CARTESIAN_POINT('Ctrl Pts',(-0.783283374325619,6.72374189737634,
73.2343749653461));
#27279=CARTESIAN_POINT('Ctrl Pts',(-0.954610411039097,6.69932891886462,
73.242510736374));
#27280=CARTESIAN_POINT('Ctrl Pts',(-1.12580048206165,6.67493545706511,73.2506400033409));
#27281=CARTESIAN_POINT('Ctrl Pts',(-1.29620704255985,6.64395432029271,73.2587692703078));
#27282=CARTESIAN_POINT('Ctrl Pts',(-1.46528231078734,6.60645417373751,73.2668985372747));
#27283=CARTESIAN_POINT('Ctrl Pts',(-1.63425796263297,6.56897612165513,73.2750230146105));
#27284=CARTESIAN_POINT('Ctrl Pts',(-1.80190352818636,6.52498678775252,73.2831474919462));
#27285=CARTESIAN_POINT('Ctrl Pts',(-1.967679599671,6.4746062423161,73.291271969282));
#27286=CARTESIAN_POINT('Ctrl Pts',(-2.13446028624788,6.42392038709735,73.2994456815434));
#27287=CARTESIAN_POINT('Ctrl Pts',(-2.29934837463323,6.36676565786725,73.3076193938048));
#27288=CARTESIAN_POINT('Ctrl Pts',(-2.46180767628279,6.30331594995802,73.3157931060662));
#27289=CARTESIAN_POINT('Ctrl Pts',(-2.62322832714176,6.24027189496378,73.3239145613462));
#27290=CARTESIAN_POINT('Ctrl Pts',(-2.78225082007247,6.1710132738783,73.3320360166262));
#27291=CARTESIAN_POINT('Ctrl Pts',(-2.93836730018601,6.09575972370939,73.3401574719062));
#27292=CARTESIAN_POINT('Ctrl Pts',(-3.09449584766683,6.02050035665153,73.348279554952));
#27293=CARTESIAN_POINT('Ctrl Pts',(-3.24771760519109,5.93924529635381,73.3564016379978));
#27294=CARTESIAN_POINT('Ctrl Pts',(-3.39754771358598,5.85226097623019,73.3645237210436));
#27295=CARTESIAN_POINT('Ctrl Pts',(-3.54741793373219,5.76525336910867,73.3726479784919));
#27296=CARTESIAN_POINT('Ctrl Pts',(-3.69389438039104,5.67251363174842,73.3807722359403));
#27297=CARTESIAN_POINT('Ctrl Pts',(-3.83651970643785,5.57435247738372,73.3888964933887));
#27298=CARTESIAN_POINT('Ctrl Pts',(-3.9806862301632,5.47513060156496,73.3971085409026));
#27299=CARTESIAN_POINT('Ctrl Pts',(-4.12091760154934,5.37036967537356,73.4053205884165));
#27300=CARTESIAN_POINT('Ctrl Pts',(-4.25677506424986,5.26043297195018,73.4135326359304));
#27301=CARTESIAN_POINT('Ctrl Pts',(-4.39139473239348,5.15149789957744,73.4216698636478));
#27302=CARTESIAN_POINT('Ctrl Pts',(-4.52171962839195,5.03748125929308,73.4298070913652));
#27303=CARTESIAN_POINT('Ctrl Pts',(-4.64735964561845,4.91877396556064,73.4379443190825));
#27304=CARTESIAN_POINT('Ctrl Pts',(-4.77473250617606,4.79842944551418,73.4461937764947));
#27305=CARTESIAN_POINT('Ctrl Pts',(-4.89729004003016,4.67326421850854,73.4544432339068));
#27306=CARTESIAN_POINT('Ctrl Pts',(-5.01466794408449,4.54372032706365,73.462692691319));
#27307=CARTESIAN_POINT('Ctrl Pts',(-5.13204584813878,4.41417643561881,73.4709421487311));
#27308=CARTESIAN_POINT('Ctrl Pts',(-5.24424392380754,4.28025421525507,73.4791916061433));
#27309=CARTESIAN_POINT('Ctrl Pts',(-5.35094358129603,4.14242583395126,73.4874410635555));
#27310=CARTESIAN_POINT('Ctrl Pts',(-5.45771720077136,4.00450191287571,73.4956962393202));
#27311=CARTESIAN_POINT('Ctrl Pts',(-5.55930636755762,3.86225133982876,73.5039514150849));
#27312=CARTESIAN_POINT('Ctrl Pts',(-5.65534280373195,3.71609832650822,73.5122065908496));
#27313=CARTESIAN_POINT('Ctrl Pts',(-5.75122614844573,3.57017829536785,73.5204486070577));
#27314=CARTESIAN_POINT('Ctrl Pts',(-5.84157421225403,3.4203685181075,73.5286906232659));
#27315=CARTESIAN_POINT('Ctrl Pts',(-5.92605926931867,3.26712573013685,73.536932639474));
#27316=CARTESIAN_POINT('Ctrl Pts',(-6.01046493164367,3.11402695190798,73.5451669102565));
#27317=CARTESIAN_POINT('Ctrl Pts',(-6.08901838818733,2.95750189607801,73.553401181039));
#27318=CARTESIAN_POINT('Ctrl Pts',(-6.16143498754642,2.79803643547378,73.5616354518214));
#27319=CARTESIAN_POINT('Ctrl Pts',(-6.23379639318408,2.63869251457578,73.569863446694));
#27320=CARTESIAN_POINT('Ctrl Pts',(-6.30003011072029,2.47641297433791,73.5780914415667));
#27321=CARTESIAN_POINT('Ctrl Pts',(-6.35989721255139,2.31170855554526,73.5863194364393));
#27322=CARTESIAN_POINT('Ctrl Pts',(-6.41972931476821,2.14710042655032,73.5945426210466));
#27323=CARTESIAN_POINT('Ctrl Pts',(-6.47320209467886,1.98007057609258,73.6027658056538));
#27324=CARTESIAN_POINT('Ctrl Pts',(-6.52012456255799,1.81115010110371,73.6109889902611));
#27325=CARTESIAN_POINT('Ctrl Pts',(-6.56702979874941,1.64229166004028,73.6192091550069));
#27326=CARTESIAN_POINT('Ctrl Pts',(-6.60738941932224,1.47154431938259,73.6274293197528));
#27327=CARTESIAN_POINT('Ctrl Pts',(-6.64106211326897,1.29945488867581,73.6356494844986));
#27328=CARTESIAN_POINT('Ctrl Pts',(-6.67472745511617,1.12740303199343,73.6438678544529));
#27329=CARTESIAN_POINT('Ctrl Pts',(-6.70170871299765,0.954010018103379,
73.6520862244071));
#27330=CARTESIAN_POINT('Ctrl Pts',(-6.72191555794214,0.779833464205928,
73.6603045943613));
#27331=CARTESIAN_POINT('Ctrl Pts',(-6.74212466589795,0.605637403873252,
73.6685238847098));
#27332=CARTESIAN_POINT('Ctrl Pts',(-6.75555780237903,0.43065798111306,73.6767431750583));
#27333=CARTESIAN_POINT('Ctrl Pts',(-6.76217640569453,0.255458916987017,
73.6849624654068));
#27334=CARTESIAN_POINT('Ctrl Pts',(-6.76545574736762,0.168652446696076,
73.6890349048745));
#27335=CARTESIAN_POINT('Ctrl Pts',(-6.76706296667692,0.0817921139574352,
73.6931073443422));
#27336=CARTESIAN_POINT('Ctrl Pts',(-6.7669981131445,-0.00505338488856453,
73.6971797838099));
#27337=CARTESIAN_POINT('',(-6.76699967339098,-0.00123438120911981,73.3028202161898));
#27338=CARTESIAN_POINT('Ctrl Pts',(3.09917575053262,6.01559628526637,72.6513920151221));
#27339=CARTESIAN_POINT('Ctrl Pts',(2.93382384459274,6.10078395293755,72.6601414630345));
#27340=CARTESIAN_POINT('Ctrl Pts',(2.76495772122998,6.17915010267043,72.6688909109469));
#27341=CARTESIAN_POINT('Ctrl Pts',(2.59315093316731,6.25042856433169,72.6776403588593));
#27342=CARTESIAN_POINT('Ctrl Pts',(2.42134553245636,6.32170645041444,72.6863897361193));
#27343=CARTESIAN_POINT('Ctrl Pts',(2.24659977927608,6.38589665313451,72.6951391133793));
#27344=CARTESIAN_POINT('Ctrl Pts',(2.06950718689935,6.4427811543907,72.7038884906393));
#27345=CARTESIAN_POINT('Ctrl Pts',(1.89241596572876,6.4996652151972,72.712637800154));
#27346=CARTESIAN_POINT('Ctrl Pts',(1.71297821457211,6.54924360009543,72.7213871096686));
#27347=CARTESIAN_POINT('Ctrl Pts',(1.53180337335856,6.59134792173553,72.7301364191833));
#27348=CARTESIAN_POINT('Ctrl Pts',(1.35062987477787,6.63345193135304,72.7388856638594));
#27349=CARTESIAN_POINT('Ctrl Pts',(1.16771959102949,6.66808192368239,72.7476349085355));
#27350=CARTESIAN_POINT('Ctrl Pts',(0.983693746906737,6.6951202836317,72.7563841532117));
#27351=CARTESIAN_POINT('Ctrl Pts',(0.799669205419682,6.72215845218869,72.7651333359559));
#27352=CARTESIAN_POINT('Ctrl Pts',(0.614529402873204,6.74160505424582,72.7738825187));
#27353=CARTESIAN_POINT('Ctrl Pts',(0.428903127362894,6.75339404354124,72.7826317014442));
#27354=CARTESIAN_POINT('Ctrl Pts',(0.243278104163466,6.76518295330332,72.7913808251628));
#27355=CARTESIAN_POINT('Ctrl Pts',(0.0571669005386472,6.76931433552276,
72.8001299488814));
#27356=CARTESIAN_POINT('Ctrl Pts',(-0.128798404778041,6.76577415902472,
72.8088790726));
#27357=CARTESIAN_POINT('Ctrl Pts',(-0.314762517259671,6.76223400523439,
72.8176281401992));
#27358=CARTESIAN_POINT('Ctrl Pts',(-0.500580446820127,6.75102239665084,
72.8263772077985));
#27359=CARTESIAN_POINT('Ctrl Pts',(-0.68562111884327,6.73217741012491,72.8351262753977));
#27360=CARTESIAN_POINT('Ctrl Pts',(-0.870660665415115,6.71333253821764,
72.8438752897835));
#27361=CARTESIAN_POINT('Ctrl Pts',(-1.05492267885546,6.68685441030603,72.8526243041693));
#27362=CARTESIAN_POINT('Ctrl Pts',(-1.23778137635308,6.65283295028167,72.861373318555));
#27363=CARTESIAN_POINT('Ctrl Pts',(-1.42999922978902,6.61707018861854,72.8705701289224));
#27364=CARTESIAN_POINT('Ctrl Pts',(-1.62066601233749,6.572971729344,72.8797669392898));
#27365=CARTESIAN_POINT('Ctrl Pts',(-1.80906628500437,6.5207030431128,72.8889637496572));
#27366=CARTESIAN_POINT('Ctrl Pts',(-1.98831342545581,6.47097374915014,72.897713747395));
#27367=CARTESIAN_POINT('Ctrl Pts',(-2.16550875896756,6.4138493398951,72.9064637451327));
#27368=CARTESIAN_POINT('Ctrl Pts',(-2.34005036714066,6.34952386240456,72.9152137428705));
#27369=CARTESIAN_POINT('Ctrl Pts',(-2.51458843547144,6.28519968948574,72.9239635631513));
#27370=CARTESIAN_POINT('Ctrl Pts',(-2.6864726171811,6.21367483971075,72.9327133834322));
#27371=CARTESIAN_POINT('Ctrl Pts',(-2.85511905908785,6.13519226743819,72.9414632037131));
#27372=CARTESIAN_POINT('Ctrl Pts',(-3.02376230488932,6.05671118252913,72.9502128581716));
#27373=CARTESIAN_POINT('Ctrl Pts',(-3.18916767379947,5.9712727599261,72.9589625126302));
#27374=CARTESIAN_POINT('Ctrl Pts',(-3.35077334102824,5.87916720437975,72.9677121670887));
#27375=CARTESIAN_POINT('Ctrl Pts',(-3.51237616037403,5.78706327195622,72.9764616673571));
#27376=CARTESIAN_POINT('Ctrl Pts',(-3.67017916302332,5.68829258362278,72.9852111676256));
#27377=CARTESIAN_POINT('Ctrl Pts',(-3.82364636566492,5.58319061741022,72.993960667894));
#27378=CARTESIAN_POINT('Ctrl Pts',(-3.97711106778829,5.4780903636768,73.0027100256024));
#27379=CARTESIAN_POINT('Ctrl Pts',(-4.12623987481959,5.36665920043201,73.0114593833109));
#27380=CARTESIAN_POINT('Ctrl Pts',(-4.27052628213962,5.24927559512308,73.0202087410193));
#27381=CARTESIAN_POINT('Ctrl Pts',(-4.41481053025007,5.13189374643011,73.0289579677958));
#27382=CARTESIAN_POINT('Ctrl Pts',(-4.55425230136555,5.0085598147733,73.0377071945723));
#27383=CARTESIAN_POINT('Ctrl Pts',(-4.6883780063057,4.87969268192056,73.0464564213489));
#27384=CARTESIAN_POINT('Ctrl Pts',(-4.82250188228922,4.75082730631782,73.0552055288197));
#27385=CARTESIAN_POINT('Ctrl Pts',(-4.95130963053,4.6164290790349,73.0639546362906));
#27386=CARTESIAN_POINT('Ctrl Pts',(-5.07436379033406,4.47695444731646,73.0727037437614));
#27387=CARTESIAN_POINT('Ctrl Pts',(-5.19741643562834,4.33748153220551,73.0814527435511));
#27388=CARTESIAN_POINT('Ctrl Pts',(-5.31471544462792,4.19293255254564,73.0902017433409));
#27389=CARTESIAN_POINT('Ctrl Pts',(-5.42586245275638,4.04379841779589,73.0989507431306));
#27390=CARTESIAN_POINT('Ctrl Pts',(-5.53702160019161,3.89464799484331,73.1077006984728));
#27391=CARTESIAN_POINT('Ctrl Pts',(-5.64202723081257,3.74091164443841,73.1164506538149));
#27392=CARTESIAN_POINT('Ctrl Pts',(-5.74052265232971,3.58311159163227,73.1252006091571));
#27393=CARTESIAN_POINT('Ctrl Pts',(-5.83901427066928,3.42531763191766,73.1339502266395));
#27394=CARTESIAN_POINT('Ctrl Pts',(-5.93099603115756,3.26346052695584,73.142699844122));
#27395=CARTESIAN_POINT('Ctrl Pts',(-6.01615550622775,3.09809004467036,73.1514494616045));
#27396=CARTESIAN_POINT('Ctrl Pts',(-6.10131214578824,2.93272506863777,73.1601987877556));
#27397=CARTESIAN_POINT('Ctrl Pts',(-6.17964682328776,2.76384720416832,73.1689481139067));
#27398=CARTESIAN_POINT('Ctrl Pts',(-6.25089348288594,2.5920300279152,73.1776974400578));
#27399=CARTESIAN_POINT('Ctrl Pts',(-6.32213814889374,2.42021765936918,73.1864465213893));
#27400=CARTESIAN_POINT('Ctrl Pts',(-6.38629508412638,2.24546640831769,73.1951956027209));
#27401=CARTESIAN_POINT('Ctrl Pts',(-6.44314639819872,2.06836976659854,73.2039446840525));
#27402=CARTESIAN_POINT('Ctrl Pts',(-6.50000285283759,1.89125711158076,73.2126945564869));
#27403=CARTESIAN_POINT('Ctrl Pts',(-6.54955227673305,1.71179891440045,73.2214444289213));
#27404=CARTESIAN_POINT('Ctrl Pts',(-6.59162635926436,1.53060476278209,73.2301943013557));
#27405=CARTESIAN_POINT('Ctrl Pts',(-6.6336975205524,1.34942319164483,73.2389435662782));
#27406=CARTESIAN_POINT('Ctrl Pts',(-6.66829431424289,1.166506186425,73.2476928312007));
#27407=CARTESIAN_POINT('Ctrl Pts',(-6.69529923745446,0.982474997616606,
73.2564420961232));
#27408=CARTESIAN_POINT('Ctrl Pts',(-6.72230554731467,0.798434359175797,
73.2651918103029));
#27409=CARTESIAN_POINT('Ctrl Pts',(-6.74171916496721,0.6132797062384,73.2739415244826));
#27410=CARTESIAN_POINT('Ctrl Pts',(-6.75347414817287,0.427639953653452,
73.2826912386623));
#27411=CARTESIAN_POINT('Ctrl Pts',(-6.76248837758744,0.285283364197985,
73.2894008978381));
#27412=CARTESIAN_POINT('Ctrl Pts',(-6.76699999999992,0.142641701105874,
73.296110557014));
#27413=CARTESIAN_POINT('Ctrl Pts',(-6.767,3.66893179809862E-12,73.3028202161898));
#27414=CARTESIAN_POINT('Ctrl Pts',(-6.76699905248981,-0.00358100572350501,
73.3028202161898));
#27415=CARTESIAN_POINT('Ctrl Pts',(-6.7668945298339,-0.201096667011066,
73.3120892241327));
#27416=CARTESIAN_POINT('Ctrl Pts',(-6.7581382485434,-0.398339799715601,
73.3213582320757));
#27417=CARTESIAN_POINT('Ctrl Pts',(-6.74082625458302,-0.594601047362251,
73.3306272400186));
#27418=CARTESIAN_POINT('Ctrl Pts',(-6.72346196364603,-0.791455171248329,
73.3399242482654));
#27419=CARTESIAN_POINT('Ctrl Pts',(-6.69749027576094,-0.987321300288637,
73.3492212565122));
#27420=CARTESIAN_POINT('Ctrl Pts',(-6.66305861989671,-1.18149855176388,
73.358518264759));
#27421=CARTESIAN_POINT('Ctrl Pts',(-6.62848720793987,-1.37646395743209,
73.3678530090227));
#27422=CARTESIAN_POINT('Ctrl Pts',(-6.58538708590094,-1.56972658068534,
73.3771877532863));
#27423=CARTESIAN_POINT('Ctrl Pts',(-6.53395714227279,-1.76059451974109,
73.3865224975499));
#27424=CARTESIAN_POINT('Ctrl Pts',(-6.48620301544764,-1.93782068655211,
73.3951900660907));
#27425=CARTESIAN_POINT('Ctrl Pts',(-6.4312677765939,-2.11298232444131,73.4038576346315));
#27426=CARTESIAN_POINT('Ctrl Pts',(-6.3693478532621,-2.28554083843309,73.4125252031723));
#27427=CARTESIAN_POINT('Ctrl Pts',(-6.31058250118312,-2.44930818960721,
73.4207511939287));
#27428=CARTESIAN_POINT('Ctrl Pts',(-6.24541983593963,-2.61102258676869,
73.4289771846852));
#27429=CARTESIAN_POINT('Ctrl Pts',(-6.17402305823175,-2.77014950434496,
73.4372031754416));
#27430=CARTESIAN_POINT('Ctrl Pts',(-6.10270113114897,-2.92910959717604,
73.4454205422718));
#27431=CARTESIAN_POINT('Ctrl Pts',(-6.02515825204532,-3.08548728810339,
73.4536379091019));
#27432=CARTESIAN_POINT('Ctrl Pts',(-5.94160691409611,-3.23876462225418,
73.4618552759321));
#27433=CARTESIAN_POINT('Ctrl Pts',(-5.85812645102926,-3.39191193439344,
73.4700656721389));
#27434=CARTESIAN_POINT('Ctrl Pts',(-5.76864785070083,-3.54196381487223,
73.4782760683457));
#27435=CARTESIAN_POINT('Ctrl Pts',(-5.67343110477985,-3.68842357916176,
73.4864864645525));
#27436=CARTESIAN_POINT('Ctrl Pts',(-5.57827608214668,-3.83478840239765,
73.4946915384534));
#27437=CARTESIAN_POINT('Ctrl Pts',(-5.4773905178737,-3.97756544843949,73.5028966123542));
#27438=CARTESIAN_POINT('Ctrl Pts',(-5.37107965378552,-4.11628380371073,
73.5111016862551));
#27439=CARTESIAN_POINT('Ctrl Pts',(-5.264816442573,-4.25493997974382,73.5193030823065));
#27440=CARTESIAN_POINT('Ctrl Pts',(-5.15313299397265,-4.38954080574244,
73.5275044783578));
#27441=CARTESIAN_POINT('Ctrl Pts',(-5.03637711933686,-4.51964539668989,
73.5357058744091));
#27442=CARTESIAN_POINT('Ctrl Pts',(-4.91963039055831,-4.6497397961329,73.5439066280191));
#27443=CARTESIAN_POINT('Ctrl Pts',(-4.79781225981491,-4.77533838980424,
73.5521073816291));
#27444=CARTESIAN_POINT('Ctrl Pts',(-4.67131022207002,-4.89603408987153,
73.5603081352391));
#27445=CARTESIAN_POINT('Ctrl Pts',(-4.54480882726469,-5.01672917650965,
73.5685088471693));
#27446=CARTESIAN_POINT('Ctrl Pts',(-4.41362383142904,-5.13252117101907,
73.5767095590994));
#27447=CARTESIAN_POINT('Ctrl Pts',(-4.27817882947111,-5.2430406161945,73.5849102710296));
#27448=CARTESIAN_POINT('Ctrl Pts',(-4.14270996986308,-5.35357952856485,
73.5931124274554));
#27449=CARTESIAN_POINT('Ctrl Pts',(-4.00297988682076,-5.4588438147124,73.6013145838811));
#27450=CARTESIAN_POINT('Ctrl Pts',(-3.8594444509964,-5.55850497253291,73.6095167403069));
#27451=CARTESIAN_POINT('Ctrl Pts',(-3.71585771994449,-5.65820174623976,
73.6177218279356));
#27452=CARTESIAN_POINT('Ctrl Pts',(-3.56846322126033,-5.75229119848255,
73.6259269155642));
#27453=CARTESIAN_POINT('Ctrl Pts',(-3.4177449647962,-5.84048870862792,73.6341320031929));
#27454=CARTESIAN_POINT('Ctrl Pts',(-3.26685453089381,-5.92878697379604,
73.642346464145));
#27455=CARTESIAN_POINT('Ctrl Pts',(-3.11263306310723,-6.01117966866163,
73.6505609250971));
#27456=CARTESIAN_POINT('Ctrl Pts',(-2.95558922926776,-6.08742813574308,
73.6587753860492));
#27457=CARTESIAN_POINT('Ctrl Pts',(-2.79845235217987,-6.16372177750531,
73.6669947137962));
#27458=CARTESIAN_POINT('Ctrl Pts',(-2.63849010344047,-6.23386379139131,
73.6752140415432));
#27459=CARTESIAN_POINT('Ctrl Pts',(-2.47623009019335,-6.29766413366266,
73.6834333692902));
#27460=CARTESIAN_POINT('Ctrl Pts',(-2.31371866493584,-6.36156333067951,
73.6916654323851));
#27461=CARTESIAN_POINT('Ctrl Pts',(-2.14890269852081,-6.41910110179752,
73.69989749548));
#27462=CARTESIAN_POINT('Ctrl Pts',(-1.98232516376679,-6.47013724314229,
73.7081295585748));
#27463=CARTESIAN_POINT('Ctrl Pts',(-1.83259280338129,-6.51601234820857,
73.7155291532432));
#27464=CARTESIAN_POINT('Ctrl Pts',(-1.68143748548776,-6.55663493444886,
73.7229287479116));
#27465=CARTESIAN_POINT('Ctrl Pts',(-1.52925889565088,-6.5919387307584,73.73032834258));
#27466=CARTESIAN_POINT('Ctrl Pts',(-1.3615344729331,-6.63084899311601,73.7384838442536));
#27467=CARTESIAN_POINT('Ctrl Pts',(-1.19205048369878,-6.66341720214219,
73.7466393459272));
#27468=CARTESIAN_POINT('Ctrl Pts',(-1.02133203116545,-6.68948203391828,
73.7547948476007));
#27469=CARTESIAN_POINT('Ctrl Pts',(-0.85082136254669,-6.71551514180807,
73.7629404230945));
#27470=CARTESIAN_POINT('Ctrl Pts',(-0.679079578733357,-6.73506057376915,
73.7710859985883));
#27471=CARTESIAN_POINT('Ctrl Pts',(-0.50664583599944,-6.7480070388867,73.779231574082));
#27472=CARTESIAN_POINT('Ctrl Pts',(-0.334385706404295,-6.76094046898912,
73.7873689482869));
#27473=CARTESIAN_POINT('Ctrl Pts',(-0.161435366625639,-6.76728813231959,
73.7955063224918));
#27474=CARTESIAN_POINT('Ctrl Pts',(0.0116569628525796,-6.76698995973964,
73.8036436966968));
#27475=CARTESIAN_POINT('Ctrl Pts',(0.184611391120607,-6.76669202471129,
73.8117745879238));
#27476=CARTESIAN_POINT('Ctrl Pts',(0.357707220051187,-6.75975879677122,
73.8199054791507));
#27477=CARTESIAN_POINT('Ctrl Pts',(0.53039224945409,-6.74618211003224,73.8280363703777));
#27478=CARTESIAN_POINT('Ctrl Pts',(0.702975976759167,-6.73261338777549,
73.8361624917857));
#27479=CARTESIAN_POINT('Ctrl Pts',(0.875149020997245,-6.71240899658853,
73.8442886131937));
#27480=CARTESIAN_POINT('Ctrl Pts',(1.04636033042912,-6.68561284093719,73.8524147346016));
#27481=CARTESIAN_POINT('Ctrl Pts',(1.21817723480565,-6.65872190406812,73.8605695990761));
#27482=CARTESIAN_POINT('Ctrl Pts',(1.38902521657901,-6.62519249248478,73.8687244635505));
#27483=CARTESIAN_POINT('Ctrl Pts',(1.55835308561361,-6.5851214613368,73.8768793280249));
#27484=CARTESIAN_POINT('Ctrl Pts',(1.72702209283733,-6.5452063482447,73.8850024615811));
#27485=CARTESIAN_POINT('Ctrl Pts',(1.89418244129293,-6.49880053328504,73.8931255951372));
#27486=CARTESIAN_POINT('Ctrl Pts',(2.05930044737118,-6.44605078070728,73.9012487286933));
#27487=CARTESIAN_POINT('Ctrl Pts',(2.22443141676527,-6.39329688677801,73.9093724999918));
#27488=CARTESIAN_POINT('Ctrl Pts',(2.38751937590625,-6.33419817444008,73.9174962712903));
#27489=CARTESIAN_POINT('Ctrl Pts',(2.54804689179495,-6.26895095189092,73.9256200425888));
#27490=CARTESIAN_POINT('Ctrl Pts',(2.70861755005445,-6.20368619390647,73.9337459971813));
#27491=CARTESIAN_POINT('Ctrl Pts',(2.86662605611284,-6.13226977309168,73.9418719517737));
#27492=CARTESIAN_POINT('Ctrl Pts',(3.02157604846565,-6.05494567963568,73.9499979063661));
#27493=CARTESIAN_POINT('Ctrl Pts',(3.17751461768377,-5.97712826050239,73.9581757043346));
#27494=CARTESIAN_POINT('Ctrl Pts',(3.33035517554299,-5.89332769382333,73.9663535023031));
#27495=CARTESIAN_POINT('Ctrl Pts',(3.47961871874631,-5.80383860665942,73.9745313002715));
#27496=CARTESIAN_POINT('Ctrl Pts',(3.62817207918886,-5.71477530067164,73.9826701889992));
#27497=CARTESIAN_POINT('Ctrl Pts',(3.77318211615054,-5.62007773840826,73.9908090777269));
#27498=CARTESIAN_POINT('Ctrl Pts',(3.91420772899504,-5.52007851885057,73.9989479664547));
#27499=CARTESIAN_POINT('Ctrl Pts',(4.0562446346044,-5.41936220624013,74.0071452190435));
#27500=CARTESIAN_POINT('Ctrl Pts',(4.19423945743656,-5.31326814462259,74.0153424716324));
#27501=CARTESIAN_POINT('Ctrl Pts',(4.32777758708844,-5.20217552151934,74.0235397242212));
#27502=CARTESIAN_POINT('Ctrl Pts',(4.46131571674026,-5.09108289841613,74.03173697681));
#27503=CARTESIAN_POINT('Ctrl Pts',(4.59039691733635,-4.97499200813957,74.0399342293989));
#27504=CARTESIAN_POINT('Ctrl Pts',(4.71464653915873,-4.85431735785771,74.0481314819877));
#27505=CARTESIAN_POINT('Ctrl Pts',(4.83933408596642,-4.73321738278469,74.0563576262679));
#27506=CARTESIAN_POINT('Ctrl Pts',(4.95952710313247,-4.6071409550378,74.064583770548));
#27507=CARTESIAN_POINT('Ctrl Pts',(5.07480476132472,-4.47645458308648,74.0728099148282));
#27508=CARTESIAN_POINT('Ctrl Pts',(5.18995290982151,-4.34591503188515,74.0810268173744));
#27509=CARTESIAN_POINT('Ctrl Pts',(5.30019646045681,-4.21077611595185,74.0892437199207));
#27510=CARTESIAN_POINT('Ctrl Pts',(5.40514976365807,-4.07144262300565,74.097460622467));
#27511=CARTESIAN_POINT('Ctrl Pts',(5.51000622205972,-3.93223769889713,74.1056699429338));
#27512=CARTESIAN_POINT('Ctrl Pts',(5.60958194035312,-3.78884619070722,74.1138792634006));
#27513=CARTESIAN_POINT('Ctrl Pts',(5.7035300177456,-3.64170761273813,74.1220885838675));
#27514=CARTESIAN_POINT('Ctrl Pts',(5.79741025624129,-3.49467528195454,74.1302919764723));
#27515=CARTESIAN_POINT('Ctrl Pts',(5.88567075572104,-3.34390157177274,74.138495369077));
#27516=CARTESIAN_POINT('Ctrl Pts',(5.96800656585284,-3.18985683533563,74.1466987616818));
#27517=CARTESIAN_POINT('Ctrl Pts',(6.05029943927973,-3.03589243057171,74.1548978763588));
#27518=CARTESIAN_POINT('Ctrl Pts',(6.12667360978057,-2.87866071332104,74.1630969910359));
#27519=CARTESIAN_POINT('Ctrl Pts',(6.19686888050713,-2.71865869093608,74.1712961057129));
#27520=CARTESIAN_POINT('Ctrl Pts',(6.26705092974843,-2.55868680540164,74.1794936760626));
#27521=CARTESIAN_POINT('Ctrl Pts',(6.33105624777745,-2.3959459796825,74.1876912464123));
#27522=CARTESIAN_POINT('Ctrl Pts',(6.38867168667037,-2.2309556427541,74.195888816762));
#27523=CARTESIAN_POINT('Ctrl Pts',(6.44628296930304,-2.0659772078921,74.2040857957557));
#27524=CARTESIAN_POINT('Ctrl Pts',(6.49750517172593,-1.89874992334064,74.2122827747494));
#27525=CARTESIAN_POINT('Ctrl Pts',(6.54217420807248,-1.72981086573973,74.2204797537431));
#27526=CARTESIAN_POINT('Ctrl Pts',(6.58684814096861,-1.56085328930478,74.2286776312768));
#27527=CARTESIAN_POINT('Ctrl Pts',(6.6249673849238,-1.39018391282502,74.2368755088104));
#27528=CARTESIAN_POINT('Ctrl Pts',(6.65641840003207,-1.21835261058305,74.2450733863441));
#27529=CARTESIAN_POINT('Ctrl Pts',(6.6878785791955,-1.04647124091,74.2532736525384));
#27530=CARTESIAN_POINT('Ctrl Pts',(6.71266659481192,-0.873427623847161,
74.2614739187327));
#27531=CARTESIAN_POINT('Ctrl Pts',(6.73072044516196,-0.699779457457002,
74.269674184927));
#27532=CARTESIAN_POINT('Ctrl Pts',(6.74879311057494,-0.525950321294897,
74.277882997139));
#27533=CARTESIAN_POINT('Ctrl Pts',(6.76011755247661,-0.35151573431645,74.286091809351));
#27534=CARTESIAN_POINT('Ctrl Pts',(6.76468379567344,-0.177037127612258,
74.294300621563));
#27535=CARTESIAN_POINT('Ctrl Pts',(6.76925248981363,-0.00246486904519361,
74.3025138398771));
#27536=CARTESIAN_POINT('Ctrl Pts',(6.76705575824902,0.172151098040432,74.3107270581912));
#27537=CARTESIAN_POINT('Ctrl Pts',(6.75813573864054,0.346251842030471,74.3189402765053));
#27538=CARTESIAN_POINT('Ctrl Pts',(6.74920267048595,0.520607267252796,74.3271655094295));
#27539=CARTESIAN_POINT('Ctrl Pts',(6.73352669172724,0.694445605969707,74.3353907423537));
#27540=CARTESIAN_POINT('Ctrl Pts',(6.71120171431555,0.867214246751078,74.343615975278));
#27541=CARTESIAN_POINT('Ctrl Pts',(6.69100924580547,1.02347981755876,74.3510555239838));
#27542=CARTESIAN_POINT('Ctrl Pts',(6.6653780545573,1.17887021819433,74.3584950726896));
#27543=CARTESIAN_POINT('Ctrl Pts',(6.63441304834135,1.33298631050661,74.3659346213954));
#27544=CARTESIAN_POINT('Ctrl Pts',(6.60017157051125,1.50340974660639,74.3741613641998));
#27545=CARTESIAN_POINT('Ctrl Pts',(6.55931130238019,1.67275119429102,74.3823881070042));
#27546=CARTESIAN_POINT('Ctrl Pts',(6.51191234648319,1.84045825590252,74.3906148498087));
#27547=CARTESIAN_POINT('Ctrl Pts',(6.46456732214236,2.00797449679571,74.3988322320474));
#27548=CARTESIAN_POINT('Ctrl Pts',(6.41069852222834,2.17385971274366,74.4070496142861));
#27549=CARTESIAN_POINT('Ctrl Pts',(6.35043729118156,2.33757036488117,74.4152669965248));
#27550=CARTESIAN_POINT('Ctrl Pts',(6.29023253077494,2.50112760419973,74.4234766782763));
#27551=CARTESIAN_POINT('Ctrl Pts',(6.22364739306416,2.66251400373133,74.4316863600279));
#27552=CARTESIAN_POINT('Ctrl Pts',(6.15086340626104,2.82119980815234,74.4398960417794));
#27553=CARTESIAN_POINT('Ctrl Pts',(6.07813302054994,2.97976874988449,74.448099677587));
#27554=CARTESIAN_POINT('Ctrl Pts',(5.99921302826485,3.13564073349938,74.4563033133946));
#27555=CARTESIAN_POINT('Ctrl Pts',(5.91433360269426,3.28830458383064,74.4645069492022));
#27556=CARTESIAN_POINT('Ctrl Pts',(5.82949891879122,3.4408879619486,74.4727062607068));
#27557=CARTESIAN_POINT('Ctrl Pts',(5.73871123386279,3.5902662631069,74.4809055722115));
#27558=CARTESIAN_POINT('Ctrl Pts',(5.64224736972041,3.73595150114173,74.4891048837162));
#27559=CARTESIAN_POINT('Ctrl Pts',(5.54580997815359,3.88159675878073,74.497301945084));
#27560=CARTESIAN_POINT('Ctrl Pts',(5.44369970712473,4.02355067278505,74.5054990064518));
#27561=CARTESIAN_POINT('Ctrl Pts',(5.33623763147803,4.16135277769114,74.5136960678197));
#27562=CARTESIAN_POINT('Ctrl Pts',(5.22878551558251,4.29914211088527,74.5218923694712));
#27563=CARTESIAN_POINT('Ctrl Pts',(5.11598280375026,4.43278011886775,74.5300886711228));
#27564=CARTESIAN_POINT('Ctrl Pts',(4.99819194940795,4.56183803273128,74.5382849727743));
#27565=CARTESIAN_POINT('Ctrl Pts',(4.88039060421225,4.69090744093078,74.5464820044163));
#27566=CARTESIAN_POINT('Ctrl Pts',(4.75760047408038,4.81539567833841,74.5546790360583));
#27567=CARTESIAN_POINT('Ctrl Pts',(4.63022211397191,4.93490954073988,74.5628760677003));
#27568=CARTESIAN_POINT('Ctrl Pts',(4.50275829987343,5.05450358109619,74.5710785984637));
#27569=CARTESIAN_POINT('Ctrl Pts',(4.37070036836415,5.16911633407734,74.579281129227));
#27570=CARTESIAN_POINT('Ctrl Pts',(4.23448385801849,5.27839326463848,74.5874836599903));
#27571=CARTESIAN_POINT('Ctrl Pts',(4.09821754742812,5.38771014643512,74.5956891895681));
#27572=CARTESIAN_POINT('Ctrl Pts',(3.95778991377851,5.49168710161214,74.6038947191459));
#27573=CARTESIAN_POINT('Ctrl Pts',(3.81366689612691,5.59001196826856,74.6121002487237));
#27574=CARTESIAN_POINT('Ctrl Pts',(3.66939428475425,5.68843889206281,74.6203142953012));
#27575=CARTESIAN_POINT('Ctrl Pts',(3.5214189293987,5.78120181515348,74.6285283418787));
#27576=CARTESIAN_POINT('Ctrl Pts',(3.37023360463566,5.86803326934881,74.6367423884562));
#27577=CARTESIAN_POINT('Ctrl Pts',(3.28096469730114,5.91930378155252,74.6415924555108));
#27578=CARTESIAN_POINT('Ctrl Pts',(3.19057711381039,5.9685072062785,74.6464425225654));
#27579=CARTESIAN_POINT('Ctrl Pts',(3.09917575053252,6.01559628526642,74.65129258962));
#27580=CARTESIAN_POINT('Origin',(0.,0.,-3.69717978381041));
#27581=CARTESIAN_POINT('',(3.09917575053268,6.01559628526634,77.0459357433347));
#27582=CARTESIAN_POINT('',(3.09917575053257,6.0155962852664,76.6515786160344));
#27583=CARTESIAN_POINT('',(3.09917575053259,6.01559628526639,-3.69717978381041));
#27584=CARTESIAN_POINT('',(-6.7669993834644,-0.0028886315797119,75.6971797837722));
#27585=CARTESIAN_POINT('Ctrl Pts',(-6.76699938346406,-0.00288863237634982,
75.6971797838099));
#27586=CARTESIAN_POINT('Ctrl Pts',(-6.76694558422489,-0.12892039096998,
75.7031402796343));
#27587=CARTESIAN_POINT('Ctrl Pts',(-6.76337111739666,-0.254880375023853,
75.7091007754587));
#27588=CARTESIAN_POINT('Ctrl Pts',(-6.75628652671121,-0.380632853259699,
75.7150612712831));
#27589=CARTESIAN_POINT('Ctrl Pts',(-6.74651377909609,-0.554100493994067,
75.7232834006818));
#27590=CARTESIAN_POINT('Ctrl Pts',(-6.73004235460007,-0.727434860285483,
75.7315055300805));
#27591=CARTESIAN_POINT('Ctrl Pts',(-6.70687319369236,-0.900078309776879,
75.7397276594792));
#27592=CARTESIAN_POINT('Ctrl Pts',(-6.68373002776888,-1.07252805938576,
75.7479405639377));
#27593=CARTESIAN_POINT('Ctrl Pts',(-6.65390413616611,-1.2442880832005,75.7561534683962));
#27594=CARTESIAN_POINT('Ctrl Pts',(-6.61744842796308,-1.41480221347329,
75.7643663728547));
#27595=CARTESIAN_POINT('Ctrl Pts',(-6.58102628549849,-1.5851593468592,75.772571715474));
#27596=CARTESIAN_POINT('Ctrl Pts',(-6.53798655766103,-1.75427252235299,
75.7807770580933));
#27597=CARTESIAN_POINT('Ctrl Pts',(-6.48843377827388,-1.92159207558593,
75.7889824007127));
#27598=CARTESIAN_POINT('Ctrl Pts',(-6.43891665472678,-2.08879123356953,
75.7971818391549));
#27599=CARTESIAN_POINT('Ctrl Pts',(-6.38289591568522,-2.25419899708455,
75.8053812775971));
#27600=CARTESIAN_POINT('Ctrl Pts',(-6.32052688106321,-2.41727717603038,
75.8135807160394));
#27601=CARTESIAN_POINT('Ctrl Pts',(-6.25819018009885,-2.58027081119515,
75.821775903689));
#27602=CARTESIAN_POINT('Ctrl Pts',(-6.18951186787573,-2.74093693321145,
75.8299710913385));
#27603=CARTESIAN_POINT('Ctrl Pts',(-6.1146967252889,-2.89875369042305,75.8381662789881));
#27604=CARTESIAN_POINT('Ctrl Pts',(-6.03989512918573,-3.05654187237502,
75.8463599827673));
#27605=CARTESIAN_POINT('Ctrl Pts',(-5.95895906378854,-3.21148139032135,
75.8545536865464));
#27606=CARTESIAN_POINT('Ctrl Pts',(-5.87214107893503,-3.36307123758683,
75.8627473903256));
#27607=CARTESIAN_POINT('Ctrl Pts',(-5.78532900198887,-3.51465076926186,
75.8709405365286));
#27608=CARTESIAN_POINT('Ctrl Pts',(-5.69263598035683,-3.6628807721734,75.8791336827315));
#27609=CARTESIAN_POINT('Ctrl Pts',(-5.59436004092235,-3.80728574348331,
75.8873268289345));
#27610=CARTESIAN_POINT('Ctrl Pts',(-5.49607288063054,-3.95170720252756,
75.8955209106067));
#27611=CARTESIAN_POINT('Ctrl Pts',(-5.39220173462517,-4.09230246297833,
75.903714992279));
#27612=CARTESIAN_POINT('Ctrl Pts',(-5.28308741197602,-4.22862582849565,
75.9119090739513));
#27613=CARTESIAN_POINT('Ctrl Pts',(-5.17394074735488,-4.36498960086665,
75.9201055843859));
#27614=CARTESIAN_POINT('Ctrl Pts',(-5.05954803483568,-4.4970786759378,75.9283020948205));
#27615=CARTESIAN_POINT('Ctrl Pts',(-4.9402897543287,-4.62448117557796,75.9364986052552));
#27616=CARTESIAN_POINT('Ctrl Pts',(-4.8209054916518,-4.75201826078559,75.9447037743269));
#27617=CARTESIAN_POINT('Ctrl Pts',(-4.69664563788882,-4.87485861704672,
75.9529089433986));
#27618=CARTESIAN_POINT('Ctrl Pts',(-4.56792757942939,-4.99262722713086,
75.9611141124703));
#27619=CARTESIAN_POINT('Ctrl Pts',(-4.43913979586148,-5.11045963113181,
75.9693237261888));
#27620=CARTESIAN_POINT('Ctrl Pts',(-4.30588926724456,-5.22321458055498,
75.9775333399073));
#27621=CARTESIAN_POINT('Ctrl Pts',(-4.16862561853974,-5.33055808076923,
75.9857429536257));
#27622=CARTESIAN_POINT('Ctrl Pts',(-4.03115813489194,-5.43806098484935,
75.9939647585264));
#27623=CARTESIAN_POINT('Ctrl Pts',(-3.88966591261312,-5.54013617011796,
76.002186563427));
#27624=CARTESIAN_POINT('Ctrl Pts',(-3.74462772472484,-5.63649289924348,
76.0104083683277));
#27625=CARTESIAN_POINT('Ctrl Pts',(-3.61006253213103,-5.72589184996997,
76.0180364887284));
#27626=CARTESIAN_POINT('Ctrl Pts',(-3.47244546280035,-5.81036873395858,
76.0256646091292));
#27627=CARTESIAN_POINT('Ctrl Pts',(-3.33217612770128,-5.88972760439545,
76.03329272953));
#27628=CARTESIAN_POINT('Ctrl Pts',(-3.18130721697897,-5.97508329764449,
76.0414972755551));
#27629=CARTESIAN_POINT('Ctrl Pts',(-3.0269371937853,-6.05476244532253,76.0497018215801));
#27630=CARTESIAN_POINT('Ctrl Pts',(-2.86953283138995,-6.12846394535982,
76.0579063676052));
#27631=CARTESIAN_POINT('Ctrl Pts',(-2.71230795975889,-6.20208140237333,
76.0661015578525));
#27632=CARTESIAN_POINT('Ctrl Pts',(-2.55205596184382,-6.26973463211893,
76.0742967480997));
#27633=CARTESIAN_POINT('Ctrl Pts',(-2.38927063934438,-6.33116693919588,
76.082491938347));
#27634=CARTESIAN_POINT('Ctrl Pts',(-2.22663776963892,-6.39254171327962,
76.0906794535802));
#27635=CARTESIAN_POINT('Ctrl Pts',(-2.06147663517094,-6.44770703976832,
76.0988669688133));
#27636=CARTESIAN_POINT('Ctrl Pts',(-1.89430363851353,-6.49645308804077,
76.1070544840465));
#27637=CARTESIAN_POINT('Ctrl Pts',(-1.72725314759053,-6.54516341481176,
76.1152359994017));
#27638=CARTESIAN_POINT('Ctrl Pts',(-1.55819407566226,-6.58746373160529,
76.123417514757));
#27639=CARTESIAN_POINT('Ctrl Pts',(-1.38766077589796,-6.62319307970365,
76.1315990301122));
#27640=CARTESIAN_POINT('Ctrl Pts',(-1.21721771192587,-6.65890352201624,
76.13977621631));
#27641=CARTESIAN_POINT('Ctrl Pts',(-1.04530232627216,-6.68804984785324,
76.1479534025077));
#27642=CARTESIAN_POINT('Ctrl Pts',(-0.872462095912834,-6.71052150664875,
76.1561305887054));
#27643=CARTESIAN_POINT('Ctrl Pts',(-0.699654505435783,-6.73298892180089,
76.1643062306886));
#27644=CARTESIAN_POINT('Ctrl Pts',(-0.525922774676362,-6.74878412739203,
76.1724818726718));
#27645=CARTESIAN_POINT('Ctrl Pts',(-0.351822777305957,-6.75784801052589,
76.180657514655));
#27646=CARTESIAN_POINT('Ctrl Pts',(-0.177735405281618,-6.76691123636703,
76.1888325637587));
#27647=CARTESIAN_POINT('Ctrl Pts',(-0.00328018015343351,-6.76924409207052,
76.1970076128625));
#27648=CARTESIAN_POINT('Ctrl Pts',(0.170983807039123,-6.76483950568899,
76.2051826619662));
#27649=CARTESIAN_POINT('Ctrl Pts',(0.345267310525105,-6.76043442602596,
76.2133586266158));
#27650=CARTESIAN_POINT('Ctrl Pts',(0.519359172578241,-6.74929041020694,
76.2215345912652));
#27651=CARTESIAN_POINT('Ctrl Pts',(0.692702185721435,-6.73145249421674,
76.2297105559148));
#27652=CARTESIAN_POINT('Ctrl Pts',(0.866096596041697,-6.71360928918426,
76.2378889447837));
#27653=CARTESIAN_POINT('Ctrl Pts',(1.0387413563423,-6.68906826780223,76.2460673336527));
#27654=CARTESIAN_POINT('Ctrl Pts',(1.21008622448555,-6.65792612825573,76.2542457225217));
#27655=CARTESIAN_POINT('Ctrl Pts',(1.38161435648938,-6.62675068027821,76.2624328586799));
#27656=CARTESIAN_POINT('Ctrl Pts',(1.55183946318712,-6.58896007342355,76.2706199948381));
#27657=CARTESIAN_POINT('Ctrl Pts',(1.72022233242441,-6.54470198916867,76.2788071309962));
#27658=CARTESIAN_POINT('Ctrl Pts',(1.88869703941729,-6.50041976609764,76.286998732503));
#27659=CARTESIAN_POINT('Ctrl Pts',(2.05532716133459,-6.44966313953455,76.2951903340098));
#27660=CARTESIAN_POINT('Ctrl Pts',(2.21959057958728,-6.39262908817706,76.3033819355166));
#27661=CARTESIAN_POINT('Ctrl Pts',(2.38410261633552,-6.33550871376484,76.3115859353021));
#27662=CARTESIAN_POINT('Ctrl Pts',(2.54624045477815,-6.27209205858042,76.3197899350876));
#27663=CARTESIAN_POINT('Ctrl Pts',(2.70550261315695,-6.20262401006227,76.3279939348731));
#27664=CARTESIAN_POINT('Ctrl Pts',(2.85776488207488,-6.13620922080946,76.3358373525076));
#27665=CARTESIAN_POINT('Ctrl Pts',(3.00739862593188,-6.06426375596948,76.3436807701422));
#27666=CARTESIAN_POINT('Ctrl Pts',(3.15398921111939,-5.98703942329951,76.3515241877767));
#27667=CARTESIAN_POINT('Ctrl Pts',(3.30726280273132,-5.90629446404432,76.3597251836989));
#27668=CARTESIAN_POINT('Ctrl Pts',(3.45765999779837,-5.81954056214517,76.3679261796212));
#27669=CARTESIAN_POINT('Ctrl Pts',(3.60467527032724,-5.72700665230025,76.3761271755434));
#27670=CARTESIAN_POINT('Ctrl Pts',(3.75152072858995,-5.63457962643904,76.3843186986668));
#27671=CARTESIAN_POINT('Ctrl Pts',(3.89499173933582,-5.53638607589065,76.3925102217901));
#27672=CARTESIAN_POINT('Ctrl Pts',(4.03460543786044,-5.43270171837061,76.4007017449135));
#27673=CARTESIAN_POINT('Ctrl Pts',(4.17408639711627,-5.32911593990082,76.4088854798556));
#27674=CARTESIAN_POINT('Ctrl Pts',(4.30971705897001,-5.22004996373768,76.4170692147977));
#27675=CARTESIAN_POINT('Ctrl Pts',(4.44104169035459,-5.10582390065819,76.4252529497398));
#27676=CARTESIAN_POINT('Ctrl Pts',(4.57226828555852,-4.991683109373,76.4334305753778));
#27677=CARTESIAN_POINT('Ctrl Pts',(4.69919498096423,-4.87239013893223,76.4416082010157));
#27678=CARTESIAN_POINT('Ctrl Pts',(4.82139738678169,-4.74830667067058,76.4497858266537));
#27679=CARTESIAN_POINT('Ctrl Pts',(4.94353351904604,-4.62429049611128,76.4579590173519));
#27680=CARTESIAN_POINT('Ctrl Pts',(5.06095021247574,-4.49548925547615,76.4661322080501));
#27681=CARTESIAN_POINT('Ctrl Pts',(5.17325833158268,-4.3623029737411,76.4743053987483));
#27682=CARTESIAN_POINT('Ctrl Pts',(5.28554317670111,-4.22914429264627,76.4824768956888));
#27683=CARTESIAN_POINT('Ctrl Pts',(5.39272131867777,-4.09160265213043,76.4906483926292));
#27684=CARTESIAN_POINT('Ctrl Pts',(5.49444231288773,-3.95011299463052,76.4988198895697));
#27685=CARTESIAN_POINT('Ctrl Pts',(5.5961547940308,-3.80863517845135,76.5069907026346));
#27686=CARTESIAN_POINT('Ctrl Pts',(5.69241082521676,-3.6632102959724,76.5151615156995));
#27687=CARTESIAN_POINT('Ctrl Pts',(5.7829019613343,-3.51430418512626,76.5233323287644));
#27688=CARTESIAN_POINT('Ctrl Pts',(5.87340226301671,-3.3653829920447,76.5315039694255));
#27689=CARTESIAN_POINT('Ctrl Pts',(5.95813631873793,-3.21298017692343,76.5396756100866));
#27690=CARTESIAN_POINT('Ctrl Pts',(6.03684050559114,-3.05758821786946,76.5478472507477));
#27691=CARTESIAN_POINT('Ctrl Pts',(6.11556722283918,-2.90215177525838,76.5560212306781));
#27692=CARTESIAN_POINT('Ctrl Pts',(6.18826047013951,-2.74372480665621,76.5641952106085));
#27693=CARTESIAN_POINT('Ctrl Pts',(6.25470382725598,-2.58282191281346,76.5723691905389));
#27694=CARTESIAN_POINT('Ctrl Pts',(6.3212173727178,-2.42174904700708,76.5805518051644));
#27695=CARTESIAN_POINT('Ctrl Pts',(6.38146769987743,-2.2581953650045,76.5887344197898));
#27696=CARTESIAN_POINT('Ctrl Pts',(6.43528722598349,-2.09269379487151,76.5969170344152));
#27697=CARTESIAN_POINT('Ctrl Pts',(6.48913567283891,-1.92710328992665,76.6051040460944));
#27698=CARTESIAN_POINT('Ctrl Pts',(6.53654633228566,-1.7595631576783,76.6132910577736));
#27699=CARTESIAN_POINT('Ctrl Pts',(6.57740232329675,-1.59061864615329,76.6214780694527));
#27700=CARTESIAN_POINT('Ctrl Pts',(6.61831981538679,-1.42141982015728,76.6296774051519));
#27701=CARTESIAN_POINT('Ctrl Pts',(6.65266284940058,-1.25081274422523,76.6378767408511));
#27702=CARTESIAN_POINT('Ctrl Pts',(6.68036599908149,-1.07935124881386,76.6460760765503));
#27703=CARTESIAN_POINT('Ctrl Pts',(6.7070347716732,-0.914291763447366,76.6539692663747));
#27704=CARTESIAN_POINT('Ctrl Pts',(6.72755054752573,-0.748440793180089,
76.6618624561991));
#27705=CARTESIAN_POINT('Ctrl Pts',(6.7419006060402,-0.582293069059596,76.6697556460235));
#27706=CARTESIAN_POINT('Ctrl Pts',(6.75680918446336,-0.409678694533961,
76.6779560473938));
#27707=CARTESIAN_POINT('Ctrl Pts',(6.76510607348375,-0.236238752306226,
76.6861564487641));
#27708=CARTESIAN_POINT('Ctrl Pts',(6.76671116160101,-0.0625224396867994,
76.6943568501344));
#27709=CARTESIAN_POINT('Ctrl Pts',(6.76831441495384,0.110995299093639,76.7025478776862));
#27710=CARTESIAN_POINT('Ctrl Pts',(6.76324109415873,0.284788421595302,76.710738905238));
#27711=CARTESIAN_POINT('Ctrl Pts',(6.7514627060908,0.458301569127896,76.7189299327898));
#27712=CARTESIAN_POINT('Ctrl Pts',(6.73969537533962,0.631651825964342,76.7271132707676));
#27713=CARTESIAN_POINT('Ctrl Pts',(6.72123553599781,0.804722273265913,76.7352966087455));
#27714=CARTESIAN_POINT('Ctrl Pts',(6.69610671255181,0.976956444330344,76.7434799467234));
#27715=CARTESIAN_POINT('Ctrl Pts',(6.67099634724974,1.14906410238369,76.7516572737063));
#27716=CARTESIAN_POINT('Ctrl Pts',(6.63922680585662,1.32033635172206,76.7598346006892));
#27717=CARTESIAN_POINT('Ctrl Pts',(6.6008735259449,1.49022068650244,76.7680119276722));
#27718=CARTESIAN_POINT('Ctrl Pts',(6.56254058675614,1.66001492285582,76.7761849177967));
#27719=CARTESIAN_POINT('Ctrl Pts',(6.51763094366037,1.82842235944485,76.7843579079213));
#27720=CARTESIAN_POINT('Ctrl Pts',(6.46627134011109,1.99489948520167,76.7925308980459));
#27721=CARTESIAN_POINT('Ctrl Pts',(6.41492143745227,2.16134516647203,76.800702344442));
#27722=CARTESIAN_POINT('Ctrl Pts',(6.35712410075653,2.32586091634325,76.8088737908381));
#27723=CARTESIAN_POINT('Ctrl Pts',(6.29305635190756,2.4879169503253,76.8170452372342));
#27724=CARTESIAN_POINT('Ctrl Pts',(6.22899324904884,2.64996123251699,76.8252160910629));
#27725=CARTESIAN_POINT('Ctrl Pts',(6.15866077139806,2.80954581770161,76.8333869448916));
#27726=CARTESIAN_POINT('Ctrl Pts',(6.08228461484099,2.96615961540652,76.8415577987203));
#27727=CARTESIAN_POINT('Ctrl Pts',(6.005899868952,3.12279102604134,76.8497295714506));
#27728=CARTESIAN_POINT('Ctrl Pts',(5.92347024850822,3.27645065885469,76.8579013441809));
#27729=CARTESIAN_POINT('Ctrl Pts',(5.83526806284311,3.42665078973088,76.8660731169113));
#27730=CARTESIAN_POINT('Ctrl Pts',(5.74703964218504,3.57689559636364,76.8742473202662));
#27731=CARTESIAN_POINT('Ctrl Pts',(5.65303541946452,3.72367854019776,76.8824215236211));
#27732=CARTESIAN_POINT('Ctrl Pts',(5.55357179756744,3.86653970486062,76.890595726976));
#27733=CARTESIAN_POINT('Ctrl Pts',(5.45400136205057,4.0095542876057,76.898778708578));
#27734=CARTESIAN_POINT('Ctrl Pts',(5.34896002110029,4.14863838027531,76.90696169018));
#27735=CARTESIAN_POINT('Ctrl Pts',(5.23880596380514,4.28336328993931,76.915144671782));
#27736=CARTESIAN_POINT('Ctrl Pts',(5.12859165816888,4.41816188687832,76.9233321290345));
#27737=CARTESIAN_POINT('Ctrl Pts',(5.01325930138959,4.54859627816795,76.9315195862871));
#27738=CARTESIAN_POINT('Ctrl Pts',(4.89320480833117,4.67427381565572,76.9397070435396));
#27739=CARTESIAN_POINT('Ctrl Pts',(4.77296769160171,4.80014253043873,76.9479069553323));
#27740=CARTESIAN_POINT('Ctrl Pts',(4.64799434283454,4.92123967936631,76.9561068671249));
#27741=CARTESIAN_POINT('Ctrl Pts',(4.51871566902883,5.03721130214659,76.9643067789176));
#27742=CARTESIAN_POINT('Ctrl Pts',(4.39426875893537,5.1488485094962,76.9722002207019));
#27743=CARTESIAN_POINT('Ctrl Pts',(4.26583276678869,5.255736246645,76.9800936624861));
#27744=CARTESIAN_POINT('Ctrl Pts',(4.13381722501289,5.35759686335084,76.9879871042704));
#27745=CARTESIAN_POINT('Ctrl Pts',(3.99656214708984,5.46350020393626,76.9961938271503));
#27746=CARTESIAN_POINT('Ctrl Pts',(3.85503363666689,5.56428086779919,77.0044005500301));
#27747=CARTESIAN_POINT('Ctrl Pts',(3.70965096763684,5.65957407393092,77.0126072729099));
#27748=CARTESIAN_POINT('Ctrl Pts',(3.56445821167055,5.75474279875514,77.0208032753655));
#27749=CARTESIAN_POINT('Ctrl Pts',(3.41542162516261,5.84443814881979,77.0289992778211));
#27750=CARTESIAN_POINT('Ctrl Pts',(3.26299338575027,5.92833561503986,77.0371952802767));
#27751=CARTESIAN_POINT('Ctrl Pts',(3.20880870231055,5.9581592072171,77.0401087679627));
#27752=CARTESIAN_POINT('Ctrl Pts',(3.15419573595972,5.98725053256884,77.0430222556487));
#27753=CARTESIAN_POINT('Ctrl Pts',(3.09917575053268,6.01559628526634,77.0459357433347));
#27754=CARTESIAN_POINT('Ctrl Pts',(3.09917575053257,6.0155962852664,75.0456602561759));
#27755=CARTESIAN_POINT('Ctrl Pts',(2.936252244306,6.09953286540656,75.0543064777294));
#27756=CARTESIAN_POINT('Ctrl Pts',(2.77005294528275,6.17677667981186,75.0629526992828));
#27757=CARTESIAN_POINT('Ctrl Pts',(2.60114913456995,6.24710430357346,75.0715989208363));
#27758=CARTESIAN_POINT('Ctrl Pts',(2.55557118817139,6.26608190184443,75.0739320654874));
#27759=CARTESIAN_POINT('Ctrl Pts',(2.50979639803627,6.28455616581868,75.0762652101384));
#27760=CARTESIAN_POINT('Ctrl Pts',(2.46383617595217,6.30252332784809,75.0785983547895));
#27761=CARTESIAN_POINT('Ctrl Pts',(2.30188633020025,6.36583414288156,75.086819647012));
#27762=CARTESIAN_POINT('Ctrl Pts',(2.13727981104482,6.42298273401547,75.0950409392344));
#27763=CARTESIAN_POINT('Ctrl Pts',(1.97052598322084,6.47374052225231,75.1032622314568));
#27764=CARTESIAN_POINT('Ctrl Pts',(1.80394795520669,6.52444479921665,75.1114748564023));
#27765=CARTESIAN_POINT('Ctrl Pts',(1.63522746682688,6.56877158618861,75.1196874813477));
#27766=CARTESIAN_POINT('Ctrl Pts',(1.46489384591365,6.60654032154534,75.1279001062932));
#27767=CARTESIAN_POINT('Ctrl Pts',(1.29470559624531,6.64427682317129,75.1361057221731));
#27768=CARTESIAN_POINT('Ctrl Pts',(1.12290730418151,6.67546634280842,75.1443113380531));
#27769=CARTESIAN_POINT('Ctrl Pts',(0.950043535671968,6.69997808058563,75.152516953933));
#27770=CARTESIAN_POINT('Ctrl Pts',(0.777292597003479,6.7244738193163,75.1607172139287));
#27771=CARTESIAN_POINT('Ctrl Pts',(0.603477921062569,6.74230040791232,75.1689174739244));
#27772=CARTESIAN_POINT('Ctrl Pts',(0.429154437381481,6.75337807833056,75.1771177339201));
#27773=CARTESIAN_POINT('Ctrl Pts',(0.254909749631426,6.7644507415327,75.1853142873175));
#27774=CARTESIAN_POINT('Ctrl Pts',(0.0801570696198197,6.7687805413485,75.1935108407149));
#27775=CARTESIAN_POINT('Ctrl Pts',(-0.0945432858093703,6.76633952496536,
75.2017073941123));
#27776=CARTESIAN_POINT('Ctrl Pts',(-0.269229525155645,6.76389870582045,
75.2099032852145));
#27777=CARTESIAN_POINT('Ctrl Pts',(-0.443863089772879,6.75468815641717,
75.2180991763166));
#27778=CARTESIAN_POINT('Ctrl Pts',(-0.61788301799291,6.73873204513104,75.2262950674187));
#27779=CARTESIAN_POINT('Ctrl Pts',(-0.791901732066226,6.72277604517159,
75.2344909013376));
#27780=CARTESIAN_POINT('Ctrl Pts',(-0.96530646080996,6.70007460874533,75.2426867352565));
#27781=CARTESIAN_POINT('Ctrl Pts',(-1.13754084878975,6.67070384722142,75.2508825691754));
#27782=CARTESIAN_POINT('Ctrl Pts',(-1.30980535679711,6.64132794939369,75.2590798363665));
#27783=CARTESIAN_POINT('Ctrl Pts',(-1.48089876252137,6.60528046312545,75.2672771035575));
#27784=CARTESIAN_POINT('Ctrl Pts',(-1.65027434260422,6.56268874731556,75.2754743707485));
#27785=CARTESIAN_POINT('Ctrl Pts',(-1.81971034495408,6.52008183753246,75.283674562195));
#27786=CARTESIAN_POINT('Ctrl Pts',(-1.98742695312793,6.47092613517448,75.2918747536415));
#27787=CARTESIAN_POINT('Ctrl Pts',(-2.15289200691712,6.41539905279105,75.300074945088));
#27788=CARTESIAN_POINT('Ctrl Pts',(-2.31854714189323,6.35980818259574,75.3082845566633));
#27789=CARTESIAN_POINT('Ctrl Pts',(-2.48194521447529,6.29783142399216,75.3164941682387));
#27790=CARTESIAN_POINT('Ctrl Pts',(-2.64257248217977,6.2296949906417,75.324703779814));
#27791=CARTESIAN_POINT('Ctrl Pts',(-2.8032949711322,6.16151816541813,75.3329182581188));
#27792=CARTESIAN_POINT('Ctrl Pts',(-2.96124305689478,6.0871745393371,75.3411327364236));
#27793=CARTESIAN_POINT('Ctrl Pts',(-3.11592718696044,6.00693655414811,75.3493472147284));
#27794=CARTESIAN_POINT('Ctrl Pts',(-3.27085351692534,5.92657293466219,75.3575745550238));
#27795=CARTESIAN_POINT('Ctrl Pts',(-3.4225053663222,5.84029668953091,75.3658018953191));
#27796=CARTESIAN_POINT('Ctrl Pts',(-3.57042063114997,5.74842461172265,75.3740292356145));
#27797=CARTESIAN_POINT('Ctrl Pts',(-3.70706071678748,5.66355569306146,75.3816294280884));
#27798=CARTESIAN_POINT('Ctrl Pts',(-3.8405123192312,5.57391213840449,75.3892296205624));
#27799=CARTESIAN_POINT('Ctrl Pts',(-3.97043679625273,5.47977377698773,75.3968298130363));
#27800=CARTESIAN_POINT('Ctrl Pts',(-4.10880138720218,5.37952002828168,75.4049237268769));
#27801=CARTESIAN_POINT('Ctrl Pts',(-4.24360748295849,5.27384752031896,75.4130176407175));
#27802=CARTESIAN_POINT('Ctrl Pts',(-4.37439261120662,5.16303963601104,75.421111554558));
#27803=CARTESIAN_POINT('Ctrl Pts',(-4.50501851826732,5.05236665207865,75.4291956146592));
#27804=CARTESIAN_POINT('Ctrl Pts',(-4.6316329194727,4.93657097059121,75.4372796747604));
#27805=CARTESIAN_POINT('Ctrl Pts',(-4.75380155701409,4.81597962584254,75.4453637348615));
#27806=CARTESIAN_POINT('Ctrl Pts',(-4.87584800581626,4.69550889228077,75.4534397095724));
#27807=CARTESIAN_POINT('Ctrl Pts',(-4.99345727873904,4.5702523008029,75.4615156842834));
#27808=CARTESIAN_POINT('Ctrl Pts',(-5.10622758671122,4.44057753368966,75.4695916589943));
#27809=CARTESIAN_POINT('Ctrl Pts',(-5.21890957791099,4.31100432218179,75.477661308955));
#27810=CARTESIAN_POINT('Ctrl Pts',(-5.32675990559054,4.17702010185328,75.4857309589158));
#27811=CARTESIAN_POINT('Ctrl Pts',(-5.42941317645325,4.0390297794589,75.4938006088766));
#27812=CARTESIAN_POINT('Ctrl Pts',(-5.53721182958505,3.89412284396309,75.5022747411639));
#27813=CARTESIAN_POINT('Ctrl Pts',(-5.63927870639082,3.74479814434747,75.5107488734512));
#27814=CARTESIAN_POINT('Ctrl Pts',(-5.73523751793923,3.59156506453974,75.5192230057385));
#27815=CARTESIAN_POINT('Ctrl Pts',(-5.82654210433266,3.44576414487559,75.5272861229349));
#27816=CARTESIAN_POINT('Ctrl Pts',(-5.91231690917891,3.29642536596832,75.5353492401312));
#27817=CARTESIAN_POINT('Ctrl Pts',(-5.9922817639834,3.14401785316687,75.5434123573276));
#27818=CARTESIAN_POINT('Ctrl Pts',(-6.07224075178296,2.99162152247324,75.5514748829347));
#27819=CARTESIAN_POINT('Ctrl Pts',(-6.14639046491053,2.83615723480353,75.5595374085418));
#27820=CARTESIAN_POINT('Ctrl Pts',(-6.21449666504386,2.67811878006908,75.5675999341489));
#27821=CARTESIAN_POINT('Ctrl Pts',(-6.28261123627576,2.52006090044411,75.5756634507406));
#27822=CARTESIAN_POINT('Ctrl Pts',(-6.34468066901941,2.35942856529058,75.5837269673323));
#27823=CARTESIAN_POINT('Ctrl Pts',(-6.40051890149288,2.19673548513068,75.591790483924));
#27824=CARTESIAN_POINT('Ctrl Pts',(-6.45637495898567,2.03399046909878,75.5998565746004));
#27825=CARTESIAN_POINT('Ctrl Pts',(-6.50599573664958,1.86918374994993,75.6079226652768));
#27826=CARTESIAN_POINT('Ctrl Pts',(-6.54924509258621,1.70284400848564,75.6159887559532));
#27827=CARTESIAN_POINT('Ctrl Pts',(-6.59253813844064,1.53633623285129,75.6240629948859));
#27828=CARTESIAN_POINT('Ctrl Pts',(-6.62944681890226,1.36829270265695,75.6321372338187));
#27829=CARTESIAN_POINT('Ctrl Pts',(-6.65988602009892,1.19925276705582,75.6402114727514));
#27830=CARTESIAN_POINT('Ctrl Pts',(-6.69034314218094,1.03011331027184,75.6482904653407));
#27831=CARTESIAN_POINT('Ctrl Pts',(-6.71432314705273,0.859976646327041,
75.6563694579301));
#27832=CARTESIAN_POINT('Ctrl Pts',(-6.73179286057427,0.689386598594249,
75.6644484505195));
#27833=CARTESIAN_POINT('Ctrl Pts',(-6.74928514849801,0.51857611402685,75.6725378828008));
#27834=CARTESIAN_POINT('Ctrl Pts',(-6.76025032810092,0.347311445157489,
75.6806273150821));
#27835=CARTESIAN_POINT('Ctrl Pts',(-6.76470730673057,0.176136464896053,
75.6887167473634));
#27836=CARTESIAN_POINT('Ctrl Pts',(-6.76626158030231,0.116442943775122,
75.6915377594997));
#27837=CARTESIAN_POINT('Ctrl Pts',(-6.7670248458201,0.0567602853936582,
75.694358771636));
#27838=CARTESIAN_POINT('Ctrl Pts',(-6.7669993834644,-0.00288863157981475,
75.6971797837723));
#27839=CARTESIAN_POINT('',(-6.76699950924454,-0.00257718532368157,75.3028202161604));
#27840=CARTESIAN_POINT('Ctrl Pts',(3.09917575053252,6.01559628526642,74.65129258962));
#27841=CARTESIAN_POINT('Ctrl Pts',(2.94413043308495,6.09547410041237,74.6595198212406));
#27842=CARTESIAN_POINT('Ctrl Pts',(2.78616723896163,6.16926519409222,74.6677470528611));
#27843=CARTESIAN_POINT('Ctrl Pts',(2.62581165236062,6.23677818800117,74.6759742844817));
#27844=CARTESIAN_POINT('Ctrl Pts',(2.57537278231676,6.25801398775238,74.6785621099221));
#27845=CARTESIAN_POINT('Ctrl Pts',(2.52469732381167,6.27862901756869,74.6811499353626));
#27846=CARTESIAN_POINT('Ctrl Pts',(2.47380190500018,6.29861835125907,74.6837377608031));
#27847=CARTESIAN_POINT('Ctrl Pts',(2.3134576069224,6.36159407195207,74.6918906174548));
#27848=CARTESIAN_POINT('Ctrl Pts',(2.15045627898565,6.41854141552854,74.7000434741066));
#27849=CARTESIAN_POINT('Ctrl Pts',(1.98529534587594,6.46922649082897,74.7081963307584));
#27850=CARTESIAN_POINT('Ctrl Pts',(1.82032574068788,6.51985285085133,74.7163397428697));
#27851=CARTESIAN_POINT('Ctrl Pts',(1.65320185620246,6.5642312770898,74.724483154981));
#27852=CARTESIAN_POINT('Ctrl Pts',(1.48444204070888,6.6021754617532,74.7326265670922));
#27853=CARTESIAN_POINT('Ctrl Pts',(1.31584224855384,6.64008366655321,74.7407622573653));
#27854=CARTESIAN_POINT('Ctrl Pts',(1.14560996789608,6.67156969676873,74.7488979476384));
#27855=CARTESIAN_POINT('Ctrl Pts',(0.974279696714471,6.69649670145293,74.7570336379114));
#27856=CARTESIAN_POINT('Ctrl Pts',(0.803075891661222,6.7214053064594,74.765163322887));
#27857=CARTESIAN_POINT('Ctrl Pts',(0.63077607008167,6.73976447380729,74.7732930078626));
#27858=CARTESIAN_POINT('Ctrl Pts',(0.457925940292265,6.75148819396194,74.7814226928381));
#27859=CARTESIAN_POINT('Ctrl Pts',(0.285167097745749,6.76320572247479,74.7895480842877));
#27860=CARTESIAN_POINT('Ctrl Pts',(0.111858889681834,6.768294758233,74.7976734757372));
#27861=CARTESIAN_POINT('Ctrl Pts',(-0.0614468195600911,6.76672101452143,
74.8057988671868));
#27862=CARTESIAN_POINT('Ctrl Pts',(-0.23540362763242,6.76514135835208,74.8139547852294));
#27863=CARTESIAN_POINT('Ctrl Pts',(-0.409357548712867,6.75684871675658,
74.8221107032721));
#27864=CARTESIAN_POINT('Ctrl Pts',(-0.582748894518102,6.7418612212013,74.8302666213148));
#27865=CARTESIAN_POINT('Ctrl Pts',(-0.75545270009904,6.72693315482924,74.8383901990945));
#27866=CARTESIAN_POINT('Ctrl Pts',(-0.927598018683367,6.70536328383634,
74.8465137768742));
#27867=CARTESIAN_POINT('Ctrl Pts',(-1.09863573120725,6.6772216175678,74.8546373546539));
#27868=CARTESIAN_POINT('Ctrl Pts',(-1.26969619627758,6.64907620771219,74.8627620130846));
#27869=CARTESIAN_POINT('Ctrl Pts',(-1.43964840083078,6.61435732068323,74.8708866715153));
#27870=CARTESIAN_POINT('Ctrl Pts',(-1.6079523839229,6.57318629973597,74.879011329946));
#27871=CARTESIAN_POINT('Ctrl Pts',(-1.77631077131051,6.53200197024813,74.8871386146742));
#27872=CARTESIAN_POINT('Ctrl Pts',(-1.94301952115045,6.48436144051514,74.8952658994024));
#27873=CARTESIAN_POINT('Ctrl Pts',(-2.1075528641131,6.43043621576085,74.9033931841305));
#27874=CARTESIAN_POINT('Ctrl Pts',(-2.27313268126583,6.37616801276954,74.9115721604705));
#27875=CARTESIAN_POINT('Ctrl Pts',(-2.4365089680254,6.31553501475819,74.9197511368105));
#27876=CARTESIAN_POINT('Ctrl Pts',(-2.59716616673497,6.24876122942517,74.9279301131506));
#27877=CARTESIAN_POINT('Ctrl Pts',(-2.75708328973481,6.18229504099394,74.9360714126123));
#27878=CARTESIAN_POINT('Ctrl Pts',(-2.91430601824737,6.10974473297503,74.944212712074));
#27879=CARTESIAN_POINT('Ctrl Pts',(-3.0683508613743,6.03137728810789,74.9523540115358));
#27880=CARTESIAN_POINT('Ctrl Pts',(-3.22346505384107,5.95246583168064,74.960551826315));
#27881=CARTESIAN_POINT('Ctrl Pts',(-3.37535675287037,5.86765636976144,74.9687496410941));
#27882=CARTESIAN_POINT('Ctrl Pts',(-3.52356256017727,5.77726543310215,74.9769474558732));
#27883=CARTESIAN_POINT('Ctrl Pts',(-3.67176836748422,5.68687449644283,74.9851452706524));
#27884=CARTESIAN_POINT('Ctrl Pts',(-3.81628800975053,5.59090234420921,74.9933430854316));
#27885=CARTESIAN_POINT('Ctrl Pts',(-3.95669274005271,5.48970596305614,75.0015409002108));
#27886=CARTESIAN_POINT('Ctrl Pts',(-4.09673947537978,5.38876760594453,75.0097178127276));
#27887=CARTESIAN_POINT('Ctrl Pts',(-4.23313948046358,5.28230936702573,75.0178947252445));
#27888=CARTESIAN_POINT('Ctrl Pts',(-4.36542511513103,5.17062400143186,75.0260716377614));
#27889=CARTESIAN_POINT('Ctrl Pts',(-4.49755300339918,5.0590718170736,75.034238799571));
#27890=CARTESIAN_POINT('Ctrl Pts',(-4.62557601351266,4.94230514731659,75.0424059613805));
#27891=CARTESIAN_POINT('Ctrl Pts',(-4.74905519303882,4.8206600972762,75.0505731231901));
#27892=CARTESIAN_POINT('Ctrl Pts',(-4.8724128025047,4.69913481152419,75.0587322441108));
#27893=CARTESIAN_POINT('Ctrl Pts',(-4.99123523133266,4.57274096208986,75.0668913650316));
#27894=CARTESIAN_POINT('Ctrl Pts',(-5.10511635540047,4.44185501765002,75.0750504859523));
#27895=CARTESIAN_POINT('Ctrl Pts',(-5.21890902677056,4.31107073373535,75.0832032695958));
#27896=CARTESIAN_POINT('Ctrl Pts',(-5.32776779859115,4.17580157616478,75.0913560532393));
#27897=CARTESIAN_POINT('Ctrl Pts',(-5.43132319685854,4.03646099092589,75.0995088368828));
#27898=CARTESIAN_POINT('Ctrl Pts',(-5.53892443555819,3.89167646183618,75.1079801443527));
#27899=CARTESIAN_POINT('Ctrl Pts',(-5.64079924473297,3.74249622148247,75.1164514518226));
#27900=CARTESIAN_POINT('Ctrl Pts',(-5.73657842999148,3.58942292249834,75.1249227592925));
#27901=CARTESIAN_POINT('Ctrl Pts',(-5.82867849433613,3.44222955634225,75.1330686624024));
#27902=CARTESIAN_POINT('Ctrl Pts',(-5.91514230575042,3.29143698702313,75.1412145655123));
#27903=CARTESIAN_POINT('Ctrl Pts',(-5.99568538203235,3.13752223891458,75.1493604686222));
#27904=CARTESIAN_POINT('Ctrl Pts',(-6.07622062204455,2.98362246561874,75.1575055791936));
#27905=CARTESIAN_POINT('Ctrl Pts',(-6.15083610494592,2.82660144059169,75.1656506897649));
#27906=CARTESIAN_POINT('Ctrl Pts',(-6.21929326435158,2.66696087185227,75.1737958003362));
#27907=CARTESIAN_POINT('Ctrl Pts',(-6.28775664497366,2.50730579537495,75.181941651115));
#27908=CARTESIAN_POINT('Ctrl Pts',(-6.3500604445398,2.34503103571817,75.1900875018937));
#27909=CARTESIAN_POINT('Ctrl Pts',(-6.40601422093905,2.18065834121871,75.1982333526724));
#27910=CARTESIAN_POINT('Ctrl Pts',(-6.46198361135054,2.01623977819294,75.206381476567));
#27911=CARTESIAN_POINT('Ctrl Pts',(-6.51159933340503,1.84972245903932,75.2145296004615));
#27912=CARTESIAN_POINT('Ctrl Pts',(-6.55472079588228,1.68164332961196,75.2226777243561));
#27913=CARTESIAN_POINT('Ctrl Pts',(-6.59788165812257,1.51341062752053,75.2308332931315));
#27914=CARTESIAN_POINT('Ctrl Pts',(-6.63453632191359,1.3436136182976,75.2389888619069));
#27915=CARTESIAN_POINT('Ctrl Pts',(-6.66459516543763,1.17280018793716,75.2471444306823));
#27916=CARTESIAN_POINT('Ctrl Pts',(-6.69467028720986,1.00189425423693,75.2553044160738));
#27917=CARTESIAN_POINT('Ctrl Pts',(-6.71814242126883,0.829971162146733,
75.2634644014653));
#27918=CARTESIAN_POINT('Ctrl Pts',(-6.73497384065071,0.657583732881759,
75.2716243868568));
#27919=CARTESIAN_POINT('Ctrl Pts',(-6.75182495625526,0.484994574866744,
75.2797939211097));
#27920=CARTESIAN_POINT('Ctrl Pts',(-6.7620198204316,0.311940356769789,75.2879634553625));
#27921=CARTESIAN_POINT('Ctrl Pts',(-6.76557278506292,0.13897442216476,75.2961329896153));
#27922=CARTESIAN_POINT('Ctrl Pts',(-6.76654221933179,0.0917802838171845,
75.2983620651304));
#27923=CARTESIAN_POINT('Ctrl Pts',(-6.76701747370815,0.0445926923504295,
75.3005911406454));
#27924=CARTESIAN_POINT('Ctrl Pts',(-6.76699950924454,-0.00257718532368525,
75.3028202161604));
#27925=CARTESIAN_POINT('Ctrl Pts',(-6.7669995092443,-0.00257718594549182,
75.3028202161898));
#27926=CARTESIAN_POINT('Ctrl Pts',(-6.76695511988582,-0.119131743290941,
75.3083281573327));
#27927=CARTESIAN_POINT('Ctrl Pts',(-6.7638995537784,-0.235635131100597,
75.3138360984756));
#27928=CARTESIAN_POINT('Ctrl Pts',(-6.75783999317536,-0.351976741617549,
75.3193440396185));
#27929=CARTESIAN_POINT('Ctrl Pts',(-6.74832645104384,-0.534633684225855,
75.327991536286));
#27930=CARTESIAN_POINT('Ctrl Pts',(-6.73139459518651,-0.717067462451649,
75.3366390329534));
#27931=CARTESIAN_POINT('Ctrl Pts',(-6.70706262624517,-0.898665637278532,
75.3452865296209));
#27932=CARTESIAN_POINT('Ctrl Pts',(-6.68276187306911,-1.08003083769983,
75.3539229323145));
#27933=CARTESIAN_POINT('Ctrl Pts',(-6.65107997811199,-1.26056227178707,
75.3625593350081));
#27934=CARTESIAN_POINT('Ctrl Pts',(-6.61208702713136,-1.43965070265018,
75.3711957377018));
#27935=CARTESIAN_POINT('Ctrl Pts',(-6.57180993352493,-1.62463699664177,
75.3801165603368));
#27936=CARTESIAN_POINT('Ctrl Pts',(-6.52373201512505,-1.80808330155989,
75.3890373829718));
#27937=CARTESIAN_POINT('Ctrl Pts',(-6.4679886896944,-1.98932433504074,75.3979582056069));
#27938=CARTESIAN_POINT('Ctrl Pts',(-6.41417229764686,-2.16430023462252,
75.4065706535476));
#27939=CARTESIAN_POINT('Ctrl Pts',(-6.35321164717404,-2.33722043335061,
75.4151831014883));
#27940=CARTESIAN_POINT('Ctrl Pts',(-6.28528044630663,-2.50749650274444,
75.423795549429));
#27941=CARTESIAN_POINT('Ctrl Pts',(-6.21741364601772,-2.67761114591238,
75.4323998325408));
#27942=CARTESIAN_POINT('Ctrl Pts',(-6.14258958304672,-2.84508637535941,
75.4410041156527));
#27943=CARTESIAN_POINT('Ctrl Pts',(-6.06103140439988,-3.0093499821188,75.4496083987645));
#27944=CARTESIAN_POINT('Ctrl Pts',(-5.97956517166778,-3.17342840367871,
75.4582029817004));
#27945=CARTESIAN_POINT('Ctrl Pts',(-5.89138010394163,-3.33430215333452,
75.4667975646363));
#27946=CARTESIAN_POINT('Ctrl Pts',(-5.79674706374688,-3.49141983710666,
75.4753921475722));
#27947=CARTESIAN_POINT('Ctrl Pts',(-5.78627411962668,-3.50880789437562,
75.4763433014889));
#27948=CARTESIAN_POINT('Ctrl Pts',(-5.7757222510552,-3.52614997036092,75.4772944554055));
#27949=CARTESIAN_POINT('Ctrl Pts',(-5.76509186076488,-3.54344533426756,
75.4782456093221));
#27950=CARTESIAN_POINT('Ctrl Pts',(-5.66902795920877,-3.69973876191513,
75.4868409246132));
#27951=CARTESIAN_POINT('Ctrl Pts',(-5.56666113924929,-3.85203150406105,
75.4954362399043));
#27952=CARTESIAN_POINT('Ctrl Pts',(-5.45835665296343,-3.99982895247407,
75.5040315551953));
#27953=CARTESIAN_POINT('Ctrl Pts',(-5.34995091271714,-4.14776457685291,
75.5126349062543));
#27954=CARTESIAN_POINT('Ctrl Pts',(-5.23559660637491,-4.29119627254647,
75.5212382573133));
#27955=CARTESIAN_POINT('Ctrl Pts',(-5.11569926429793,-4.42966251956756,
75.5298416083722));
#27956=CARTESIAN_POINT('Ctrl Pts',(-4.99108064550539,-4.57358124332105,
75.53878373926));
#27957=CARTESIAN_POINT('Ctrl Pts',(-4.86047385924745,-4.71213526341169,
75.5477258701478));
#27958=CARTESIAN_POINT('Ctrl Pts',(-4.724375335431,-4.84484950127156,75.5566680010357));
#27959=CARTESIAN_POINT('Ctrl Pts',(-4.5930757902966,-4.97288409397118,75.565294822879));
#27960=CARTESIAN_POINT('Ctrl Pts',(-4.4566654365246,-5.09548354393135,75.5739216447223));
#27961=CARTESIAN_POINT('Ctrl Pts',(-4.31562317917473,-5.2122629994437,75.5825484665656));
#27962=CARTESIAN_POINT('Ctrl Pts',(-4.17444631306465,-5.32915390763711,
75.5911835217272));
#27963=CARTESIAN_POINT('Ctrl Pts',(-4.02862896005788,-5.44021354694062,
75.5998185768888));
#27964=CARTESIAN_POINT('Ctrl Pts',(-3.87868012836255,-5.54509958989426,
75.6084536320504));
#27965=CARTESIAN_POINT('Ctrl Pts',(-3.72850930140897,-5.65014091384562,
75.6171014711816));
#27966=CARTESIAN_POINT('Ctrl Pts',(-3.57419502728713,-5.7489902088327,75.6257493103127));
#27967=CARTESIAN_POINT('Ctrl Pts',(-3.41627335681156,-5.84134961730074,
75.6343971494439));
#27968=CARTESIAN_POINT('Ctrl Pts',(-3.39953355785119,-5.851139774188,75.6353138259713));
#27969=CARTESIAN_POINT('Ctrl Pts',(-3.38275324631712,-5.86085705344682,
75.6362305024987));
#27970=CARTESIAN_POINT('Ctrl Pts',(-3.36593307495136,-5.87050113150049,
75.6371471790261));
#27971=CARTESIAN_POINT('Ctrl Pts',(-3.21504622272769,-5.95701419658615,
75.6453703078352));
#27972=CARTESIAN_POINT('Ctrl Pts',(-3.06062266175904,-6.03782044790086,
75.6535934366442));
#27973=CARTESIAN_POINT('Ctrl Pts',(-2.90313284033744,-6.11261880959006,
75.6618165654533));
#27974=CARTESIAN_POINT('Ctrl Pts',(-2.74580854084296,-6.18733855814185,
75.6700310517474));
#27975=CARTESIAN_POINT('Ctrl Pts',(-2.58542471950291,-6.25606283843597,
75.6782455380416));
#27976=CARTESIAN_POINT('Ctrl Pts',(-2.42247862355748,-6.31853514023678,
75.6864600243357));
#27977=CARTESIAN_POINT('Ctrl Pts',(-2.2596711106832,-6.3809543103354,75.6946675243395));
#27978=CARTESIAN_POINT('Ctrl Pts',(-2.09430599618221,-6.43713196409455,
75.7028750243433));
#27979=CARTESIAN_POINT('Ctrl Pts',(-1.92690291084765,-6.48685857500893,
75.7110825243471));
#27980=CARTESIAN_POINT('Ctrl Pts',(-1.75960864155004,-6.53655286242867,
75.7192846892783));
#27981=CARTESIAN_POINT('Ctrl Pts',(-1.59027938264561,-6.57980435797223,
75.7274868542094));
#27982=CARTESIAN_POINT('Ctrl Pts',(-1.41945251573209,-6.6164524902384,75.7356890191405));
#27983=CARTESIAN_POINT('Ctrl Pts',(-1.24870245337201,-6.65308414533393,
75.7438874963402));
#27984=CARTESIAN_POINT('Ctrl Pts',(-1.07645647432253,-6.68311827694216,
75.7520859735398));
#27985=CARTESIAN_POINT('Ctrl Pts',(-0.90326490629413,-6.70644477417487,
75.7602844507395));
#27986=CARTESIAN_POINT('Ctrl Pts',(-0.730087019760185,-6.72976942870042,
75.7684822802897));
#27987=CARTESIAN_POINT('Ctrl Pts',(-0.555964046950391,-6.74638744779066,
75.77668010984));
#27988=CARTESIAN_POINT('Ctrl Pts',(-0.381454617778284,-6.75624018034999,
75.7848779393902));
#27989=CARTESIAN_POINT('Ctrl Pts',(-0.206946137542495,-6.76609285933275,
75.7930757243628));
#27990=CARTESIAN_POINT('Ctrl Pts',(-0.0320515631633243,-6.76918030376751,
75.8012735093354));
#27991=CARTESIAN_POINT('Ctrl Pts',(0.142667390920719,-6.76549591793299,
75.8094712943079));
#27992=CARTESIAN_POINT('Ctrl Pts',(0.317417124460915,-6.7618108830367,75.8176705234476));
#27993=CARTESIAN_POINT('Ctrl Pts',(0.491990817478394,-6.75135164868189,
75.8258697525873));
#27994=CARTESIAN_POINT('Ctrl Pts',(0.665828741854239,-6.73416372584754,
75.8340689817269));
#27995=CARTESIAN_POINT('Ctrl Pts',(0.839728860361798,-6.71696965367645,
75.8422711443113));
#27996=CARTESIAN_POINT('Ctrl Pts',(1.01289232915633,-6.69304213281326,75.8504733068957));
#27997=CARTESIAN_POINT('Ctrl Pts',(1.18476645688375,-6.66247832586667,75.8586754694801));
#27998=CARTESIAN_POINT('Ctrl Pts',(1.35683740336337,-6.63187951929318,75.8668870246323));
#27999=CARTESIAN_POINT('Ctrl Pts',(1.5276157055801,-6.59462930720231,75.8750985797845));
#28000=CARTESIAN_POINT('Ctrl Pts',(1.69655971005235,-6.55087583077462,75.8833101349367));
#28001=CARTESIAN_POINT('Ctrl Pts',(1.86560396893598,-6.50709639024694,75.8915265629735));
#28002=CARTESIAN_POINT('Ctrl Pts',(2.03281141742198,-6.45680609585874,75.8997429910102));
#28003=CARTESIAN_POINT('Ctrl Pts',(2.19765751844408,-6.40020237427116,75.907959419047));
#28004=CARTESIAN_POINT('Ctrl Pts',(2.36275989240819,-6.34351065544149,75.9161886205019));
#28005=CARTESIAN_POINT('Ctrl Pts',(2.52549324862212,-6.28048602473466,75.9244178219569));
#28006=CARTESIAN_POINT('Ctrl Pts',(2.6853536801091,-6.21137381041622,75.9326470234118));
#28007=CARTESIAN_POINT('Ctrl Pts',(2.82977491730534,-6.14893639920448,75.9400814550858));
#28008=CARTESIAN_POINT('Ctrl Pts',(2.9718514988971,-6.08153118812264,75.9475158867598));
#28009=CARTESIAN_POINT('Ctrl Pts',(3.11123121399388,-6.00937012781457,75.9549503184337));
#28010=CARTESIAN_POINT('Ctrl Pts',(3.26423963955559,-5.93015307519732,75.9631116974737));
#28011=CARTESIAN_POINT('Ctrl Pts',(3.41446835462247,-5.84496017405954,75.9712730765136));
#28012=CARTESIAN_POINT('Ctrl Pts',(3.56141261819242,-5.75400983341007,75.9794344555535));
#28013=CARTESIAN_POINT('Ctrl Pts',(3.70817816975507,-5.66317010557085,75.9875859088134));
#28014=CARTESIAN_POINT('Ctrl Pts',(3.85166691434113,-5.56658706664381,75.9957373620734));
#28015=CARTESIAN_POINT('Ctrl Pts',(3.99139590383308,-5.46452630507572,76.0038888153333));
#28016=CARTESIAN_POINT('Ctrl Pts',(4.13098424279492,-5.36256827738032,76.0120320633795));
#28017=CARTESIAN_POINT('Ctrl Pts',(4.26682006869858,-5.25514371809648,76.0201753114257));
#28018=CARTESIAN_POINT('Ctrl Pts',(4.39844678641759,-5.14256306398403,76.0283185594719));
#28019=CARTESIAN_POINT('Ctrl Pts',(4.52996858175746,-5.03007215023948,76.0364553163667));
#28020=CARTESIAN_POINT('Ctrl Pts',(4.65728767356832,-4.91243356157915,76.0445920732614));
#28021=CARTESIAN_POINT('Ctrl Pts',(4.77997812395736,-4.78999980527026,76.0527288301562));
#28022=CARTESIAN_POINT('Ctrl Pts',(4.90259646587445,-4.66763800656731,76.0608608048604));
#28023=CARTESIAN_POINT('Ctrl Pts',(5.020591326389,-4.54048690999453,76.0689927795647));
#28024=CARTESIAN_POINT('Ctrl Pts',(5.1335714292822,-4.40893789709694,76.077124754269));
#28025=CARTESIAN_POINT('Ctrl Pts',(5.24681857948396,-4.27707794617628,76.0852759502511));
#28026=CARTESIAN_POINT('Ctrl Pts',(5.35502696583186,-4.14079951400846,76.0934271462333));
#28027=CARTESIAN_POINT('Ctrl Pts',(5.45784078059092,-4.00053284122487,76.1015783422155));
#28028=CARTESIAN_POINT('Ctrl Pts',(5.56037376191622,-3.86064930344557,76.1097072734042));
#28029=CARTESIAN_POINT('Ctrl Pts',(5.65754139674202,-3.71679958764573,76.1178362045929));
#28030=CARTESIAN_POINT('Ctrl Pts',(5.74903230606199,-3.56944204937628,76.1259651357815));
#28031=CARTESIAN_POINT('Ctrl Pts',(5.84053009743602,-3.4220734266991,76.134094678438));
#28032=CARTESIAN_POINT('Ctrl Pts',(5.92635012001298,-3.27119676626935,76.1422242210945));
#28033=CARTESIAN_POINT('Ctrl Pts',(6.00622549307182,-3.11729759990511,76.1503537637509));
#28034=CARTESIAN_POINT('Ctrl Pts',(6.08612202231604,-2.96335767104841,76.1584854596381));
#28035=CARTESIAN_POINT('Ctrl Pts',(6.16007059859276,-2.80639396625127,76.1666171555253));
#28036=CARTESIAN_POINT('Ctrl Pts',(6.22785129877049,-2.64691465680378,76.1747488514126));
#28037=CARTESIAN_POINT('Ctrl Pts',(6.29592669305193,-2.48674196986045,76.1829159019483));
#28038=CARTESIAN_POINT('Ctrl Pts',(6.35778031115257,-2.32403209590914,76.1910829524841));
#28039=CARTESIAN_POINT('Ctrl Pts',(6.41323926741714,-2.15931727609884,76.1992500030198));
#28040=CARTESIAN_POINT('Ctrl Pts',(6.46854518928777,-1.9950569731839,76.2073945172564));
#28041=CARTESIAN_POINT('Ctrl Pts',(6.51749164193093,-1.82880314043243,76.215539031493));
#28042=CARTESIAN_POINT('Ctrl Pts',(6.55995811662626,-1.66109557464622,76.2236835457296));
#28043=CARTESIAN_POINT('Ctrl Pts',(6.60260085177428,-1.49269192538062,76.231861864415));
#28044=CARTESIAN_POINT('Ctrl Pts',(6.63870963807863,-1.32282281502014,76.2400401831002));
#28045=CARTESIAN_POINT('Ctrl Pts',(6.66821487842452,-1.15204137736361,76.2482185017856));
#28046=CARTESIAN_POINT('Ctrl Pts',(6.69772011877043,-0.981259939707015,
76.2563968204709));
#28047=CARTESIAN_POINT('Ctrl Pts',(6.72062182365632,-0.809566545632992,
76.2645751391562));
#28048=CARTESIAN_POINT('Ctrl Pts',(6.73690308377848,-0.637515364345049,
76.2727534578415));
#28049=CARTESIAN_POINT('Ctrl Pts',(6.75327610140381,-0.464494541475684,
76.280977867683));
#28050=CARTESIAN_POINT('Ctrl Pts',(6.76300227069972,-0.290601008063937,
76.2892022775245));
#28051=CARTESIAN_POINT('Ctrl Pts',(6.76599905201254,-0.11638654632469,76.2974266873659));
#28052=CARTESIAN_POINT('Ctrl Pts',(6.76899247840497,0.0576328809457218,
76.3056418899155));
#28053=CARTESIAN_POINT('Ctrl Pts',(6.76527151208416,0.231972165641657,76.3138570924651));
#28054=CARTESIAN_POINT('Ctrl Pts',(6.75480521895299,0.406073212617499,76.3220722950146));
#28055=CARTESIAN_POINT('Ctrl Pts',(6.74434854016002,0.580014330349336,76.3302799510781));
#28056=CARTESIAN_POINT('Ctrl Pts',(6.7271588959771,0.753717290306709,76.3384876071415));
#28057=CARTESIAN_POINT('Ctrl Pts',(6.70325736954728,0.926622705101763,76.346695263205));
#28058=CARTESIAN_POINT('Ctrl Pts',(6.67937299859103,1.09940401592867,76.3548970281707));
#28059=CARTESIAN_POINT('Ctrl Pts',(6.64878638990511,1.27138856782977,76.3630987931365));
#28060=CARTESIAN_POINT('Ctrl Pts',(6.61157055828366,1.4420207185879,76.3713005581023));
#28061=CARTESIAN_POINT('Ctrl Pts',(6.57437396569766,1.61256465962842,76.3794980830971));
#28062=CARTESIAN_POINT('Ctrl Pts',(6.53055505368496,1.78175724261241,76.3876956080918));
#28063=CARTESIAN_POINT('Ctrl Pts',(6.48023818676576,1.94905157519826,76.3958931330866));
#28064=CARTESIAN_POINT('Ctrl Pts',(6.42993041616303,2.11631566420407,76.4040891761274));
#28065=CARTESIAN_POINT('Ctrl Pts',(6.373127127617,2.28168184128613,76.4122852191682));
#28066=CARTESIAN_POINT('Ctrl Pts',(6.31000303726401,2.44461667132477,76.420481262209));
#28067=CARTESIAN_POINT('Ctrl Pts',(6.24688320746188,2.60754050410187,76.4286767520591));
#28068=CARTESIAN_POINT('Ctrl Pts',(6.17744355427624,2.76803298173554,76.4368722419091));
#28069=CARTESIAN_POINT('Ctrl Pts',(6.1019075782321,2.92557907203235,76.4450677317593));
#28070=CARTESIAN_POINT('Ctrl Pts',(6.02636295823757,3.08314319109718,76.4532641594593));
#28071=CARTESIAN_POINT('Ctrl Pts',(5.94472078066831,3.23775992746542,76.4614605871593));
#28072=CARTESIAN_POINT('Ctrl Pts',(5.8572513118581,3.38893730684659,76.4696570148593));
#28073=CARTESIAN_POINT('Ctrl Pts',(5.76975592011947,3.5401594899797,76.4778558716973));
#28074=CARTESIAN_POINT('Ctrl Pts',(5.6764299768004,3.68793997528957,76.4860547285353));
#28075=CARTESIAN_POINT('Ctrl Pts',(5.57758804065649,3.83181427638733,76.4942535853733));
#28076=CARTESIAN_POINT('Ctrl Pts',(5.4786422249977,3.9758397844847,76.5024610589311));
#28077=CARTESIAN_POINT('Ctrl Pts',(5.37416903822127,4.11595061054609,76.5106685324889));
#28078=CARTESIAN_POINT('Ctrl Pts',(5.26452505114972,4.25171318244976,76.5188760060467));
#28079=CARTESIAN_POINT('Ctrl Pts',(5.15482171308313,4.38754924350633,76.5270879223627));
#28080=CARTESIAN_POINT('Ctrl Pts',(5.03994223078305,4.51903208828505,76.5352998386787));
#28081=CARTESIAN_POINT('Ctrl Pts',(4.92028120311269,4.64576386424192,76.5435117549948));
#28082=CARTESIAN_POINT('Ctrl Pts',(4.80044402700788,4.77268219721208,76.5517357597595));
#28083=CARTESIAN_POINT('Ctrl Pts',(4.6758114953634,4.89483523347394,76.5599597645243));
#28084=CARTESIAN_POINT('Ctrl Pts',(4.54681350183855,5.01186352363057,76.5681837692891));
#28085=CARTESIAN_POINT('Ctrl Pts',(4.4298368382441,5.11798594115522,76.575641378609));
#28086=CARTESIAN_POINT('Ctrl Pts',(4.30927101176112,5.21989465020696,76.5830989879291));
#28087=CARTESIAN_POINT('Ctrl Pts',(4.18545737387484,5.31735230838401,76.590556597249));
#28088=CARTESIAN_POINT('Ctrl Pts',(4.04914339526347,5.42464938291518,76.5987671337835));
#28089=CARTESIAN_POINT('Ctrl Pts',(3.9085045758614,5.52685577924727,76.606977670318));
#28090=CARTESIAN_POINT('Ctrl Pts',(3.76395772984268,5.62360304501994,76.6151882068525));
#28091=CARTESIAN_POINT('Ctrl Pts',(3.6195985629453,5.72022469447976,76.623388082855));
#28092=CARTESIAN_POINT('Ctrl Pts',(3.47134177445127,5.81140113485322,76.6315879588575));
#28093=CARTESIAN_POINT('Ctrl Pts',(3.31963737148585,5.89680394127484,76.6397878348599));
#28094=CARTESIAN_POINT('Ctrl Pts',(3.24692434436106,5.93773812946241,76.6437180952514));
#28095=CARTESIAN_POINT('Ctrl Pts',(3.17341976708094,5.97734650173748,76.6476483556429));
#28096=CARTESIAN_POINT('Ctrl Pts',(3.09917575053257,6.0155962852664,76.6515786160344));
#28097=CARTESIAN_POINT('Origin',(0.,0.,-3.69717978381041));
#28098=CARTESIAN_POINT('',(3.09917575053265,6.01559628526636,79.0457515827422));
#28099=CARTESIAN_POINT('',(3.09917575053268,6.01559628526634,78.6513920151221));
#28100=CARTESIAN_POINT('',(3.09917575053259,6.01559628526639,-3.69717978381041));
#28101=CARTESIAN_POINT('',(-6.76699915081304,0.00184116009375152,77.6971797838099));
#28102=CARTESIAN_POINT('Ctrl Pts',(-6.767,3.94374831596175E-12,77.6971797838099));
#28103=CARTESIAN_POINT('Ctrl Pts',(-6.76700000000011,-0.186007249411788,
77.7059292956159));
#28104=CARTESIAN_POINT('Ctrl Pts',(-6.75932637295459,-0.372014355523699,
77.7146788074218));
#28105=CARTESIAN_POINT('Ctrl Pts',(-6.74400518266959,-0.557389537151275,
77.7234283192278));
#28106=CARTESIAN_POINT('Ctrl Pts',(-6.72868405709685,-0.742763935807823,
77.7321777940783));
#28107=CARTESIAN_POINT('Ctrl Pts',(-6.70571545653038,-0.927506129691662,
77.7409272689289));
#28108=CARTESIAN_POINT('Ctrl Pts',(-6.67517739415703,-1.11098863924659,
77.7496767437794));
#28109=CARTESIAN_POINT('Ctrl Pts',(-6.64463945823127,-1.29447038906366,
77.7584261824014));
#28110=CARTESIAN_POINT('Ctrl Pts',(-6.60653217027184,-1.47669218228099,
77.7671756210234));
#28111=CARTESIAN_POINT('Ctrl Pts',(-6.56098496116737,-1.6570351050402,77.7759250596454));
#28112=CARTESIAN_POINT('Ctrl Pts',(-6.51543793687542,-1.83737729603934,
77.7846744627656));
#28113=CARTESIAN_POINT('Ctrl Pts',(-6.46245112202662,-2.01584035396981,
77.7934238658859));
#28114=CARTESIAN_POINT('Ctrl Pts',(-6.40220448416263,-2.19181813638084,
77.8021732690061));
#28115=CARTESIAN_POINT('Ctrl Pts',(-6.34195808575208,-2.36779521935886,
77.8109226373514));
#28116=CARTESIAN_POINT('Ctrl Pts',(-6.27445201489257,-2.54128677544771,
77.8196720056967));
#28117=CARTESIAN_POINT('Ctrl Pts',(-6.19991555136207,-2.71170355237786,
77.8284213740419));
#28118=CARTESIAN_POINT('Ctrl Pts',(-6.12537937789061,-2.88211966613023,
77.837170708339));
#28119=CARTESIAN_POINT('Ctrl Pts',(-6.04381298133639,-3.04946076210402,
77.845920042636));
#28120=CARTESIAN_POINT('Ctrl Pts',(-5.95549339426327,-3.21315848206817,
77.8546693769331));
#28121=CARTESIAN_POINT('Ctrl Pts',(-5.86717414355185,-3.37685557859594,
77.8634186779087));
#28122=CARTESIAN_POINT('Ctrl Pts',(-5.77210188986266,-3.53690907467265,
77.8721679788842));
#28123=CARTESIAN_POINT('Ctrl Pts',(-5.67059953467101,-3.69277536784855,
77.8809172798598));
#28124=CARTESIAN_POINT('Ctrl Pts',(-5.56909755761804,-3.84864108035737,
77.8896665482405));
#28125=CARTESIAN_POINT('Ctrl Pts',(-5.46116568338115,-4.00031938104218,
77.8984158166213));
#28126=CARTESIAN_POINT('Ctrl Pts',(-5.34717048686166,-4.14729511663152,
77.9071650850021));
#28127=CARTESIAN_POINT('Ctrl Pts',(-5.23317570555561,-4.29427031687988,
77.9159143215147));
#28128=CARTESIAN_POINT('Ctrl Pts',(-5.1131178217884,-4.4365427598709,77.9246635580273));
#28129=CARTESIAN_POINT('Ctrl Pts',(-4.98740459172039,-4.57362924147623,
77.9334127945399));
#28130=CARTESIAN_POINT('Ctrl Pts',(-4.86169180910849,-4.71071523514417,
77.9421619999111));
#28131=CARTESIAN_POINT('Ctrl Pts',(-4.73032391415444,-4.84261509316512,
77.9509112052822));
#28132=CARTESIAN_POINT('Ctrl Pts',(-4.59374707237299,-4.96888084331518,
77.9596604106533));
#28133=CARTESIAN_POINT('Ctrl Pts',(-4.45717070537422,-5.09514615452706,
77.9684095856095));
#28134=CARTESIAN_POINT('Ctrl Pts',(-4.31538563819543,-5.21577720253604,
77.9771587605657));
#28135=CARTESIAN_POINT('Ctrl Pts',(-4.16887341290698,-5.33036429028611,
77.985907935522));
#28136=CARTESIAN_POINT('Ctrl Pts',(-4.02236168477371,-5.44495098921153,
77.9946570807899));
#28137=CARTESIAN_POINT('Ctrl Pts',(-3.87112305634454,-5.55349359238749,
78.0034062260578));
#28138=CARTESIAN_POINT('Ctrl Pts',(-3.71567117316729,-5.65562346102476,
78.0121553713258));
#28139=CARTESIAN_POINT('Ctrl Pts',(-3.56021980457292,-5.75775299158775,
78.0209044876319));
#28140=CARTESIAN_POINT('Ctrl Pts',(-3.40055544862373,-5.85346967275362,
78.0296536039381));
#28141=CARTESIAN_POINT('Ctrl Pts',(-3.23722036323383,-5.94244842803572,
78.0384027202443));
#28142=CARTESIAN_POINT('Ctrl Pts',(-3.07388580496003,-6.03142689616499,
78.0471518083152));
#28143=CARTESIAN_POINT('Ctrl Pts',(-2.90688079257638,-6.11366734484856,
78.0559008963862));
#28144=CARTESIAN_POINT('Ctrl Pts',(-2.7367725109452,-6.18889046787344,78.0646499844571));
#28145=CARTESIAN_POINT('Ctrl Pts',(-2.56666476416548,-6.2641133543831,78.0733990450194));
#28146=CARTESIAN_POINT('Ctrl Pts',(-2.39345402971993,-6.33231884350328,
78.0821481055816));
#28147=CARTESIAN_POINT('Ctrl Pts',(-2.21772856473936,-6.39327529621079,
78.0908971661438));
#28148=CARTESIAN_POINT('Ctrl Pts',(-2.04200363768182,-6.45423156232109,
78.0996461999238));
#28149=CARTESIAN_POINT('Ctrl Pts',(-1.8637642662002,-6.50793874252076,78.1083952337038));
#28150=CARTESIAN_POINT('Ctrl Pts',(-1.6836157819463,-6.55421443796138,78.1171442674838));
#28151=CARTESIAN_POINT('Ctrl Pts',(-1.50346783419841,-6.60048999558685,
78.125893275208));
#28152=CARTESIAN_POINT('Ctrl Pts',(-1.32141106257251,-6.63933404145494,
78.1346422829322));
#28153=CARTESIAN_POINT('Ctrl Pts',(-1.13806375959081,-6.67061465527024,
78.1433912906564));
#28154=CARTESIAN_POINT('Ctrl Pts',(-0.954716987419649,-6.70189517852473,
78.1521402730513));
#28155=CARTESIAN_POINT('Ctrl Pts',(-0.770079973810508,-6.7256122653582,
78.1608892554462));
#28156=CARTESIAN_POINT('Ctrl Pts',(-0.584779770553222,-6.74168536939775,
78.1696382378411));
#28157=CARTESIAN_POINT('Ctrl Pts',(-0.391490647554734,-6.75845143942389,
78.1787644185171));
#28158=CARTESIAN_POINT('Ctrl Pts',(-0.197480213105212,-6.76689975924024,
78.1878905991932));
#28159=CARTESIAN_POINT('Ctrl Pts',(-0.00346532629872835,-6.76699911271707,
78.1970167798692));
#28160=CARTESIAN_POINT('Ctrl Pts',(0.184486595295083,-6.76709536139776,
78.2058577673991));
#28161=CARTESIAN_POINT('Ctrl Pts',(0.372442378184217,-6.75935659726775,
78.2146987549291));
#28162=CARTESIAN_POINT('Ctrl Pts',(0.559750217721036,-6.74380965729025,
78.223539742459));
#28163=CARTESIAN_POINT('Ctrl Pts',(0.745129914456703,-6.72842275717265,
78.2322897210568));
#28164=CARTESIAN_POINT('Ctrl Pts',(0.929874656313132,-6.70538772273487,
78.2410396996546));
#28165=CARTESIAN_POINT('Ctrl Pts',(1.11335688289672,-6.6747828018076,78.2497896782523));
#28166=CARTESIAN_POINT('Ctrl Pts',(1.29683723118751,-6.64417819418044,78.2585395672773));
#28167=CARTESIAN_POINT('Ctrl Pts',(1.4790548073013,-6.60600390230099,78.2672894563022));
#28168=CARTESIAN_POINT('Ctrl Pts',(1.65939064804703,-6.56038959797161,78.2760393453271));
#28169=CARTESIAN_POINT('Ctrl Pts',(1.83972470264153,-6.51477574543287,78.2847891476881));
#28170=CARTESIAN_POINT('Ctrl Pts',(2.01817678125729,-6.46172209820137,78.293538950049));
#28171=CARTESIAN_POINT('Ctrl Pts',(2.19414072347555,-6.40140886724057,78.30228875241));
#28172=CARTESIAN_POINT('Ctrl Pts',(2.37010298131968,-6.34109621361422,78.3110384710155));
#28173=CARTESIAN_POINT('Ctrl Pts',(2.54357687926781,-6.27352420826024,78.3197881896209));
#28174=CARTESIAN_POINT('Ctrl Pts',(2.71397317789835,-6.19892237325556,78.3285379082264));
#28175=CARTESIAN_POINT('Ctrl Pts',(2.8843679020706,-6.1243212275703,78.3372875459847));
#28176=CARTESIAN_POINT('Ctrl Pts',(3.0516848212611,-6.04269049717491,78.3460371837429));
#28177=CARTESIAN_POINT('Ctrl Pts',(3.21535561997237,-5.95430745235011,78.3547868215012));
#28178=CARTESIAN_POINT('Ctrl Pts',(3.37902496075119,-5.86592519481609,78.3635363813202));
#28179=CARTESIAN_POINT('Ctrl Pts',(3.53904799384704,-5.77079087940336,78.3722859411392));
#28180=CARTESIAN_POINT('Ctrl Pts',(3.69488118814804,-5.66922763747141,78.3810355009582));
#28181=CARTESIAN_POINT('Ctrl Pts',(3.85071304610658,-5.56766526649173,78.3897849857457));
#28182=CARTESIAN_POINT('Ctrl Pts',(4.00235489705798,-5.45967423580838,78.3985344705331));
#28183=CARTESIAN_POINT('Ctrl Pts',(4.14929168607489,-5.34562133936456,78.4072839553205));
#28184=CARTESIAN_POINT('Ctrl Pts',(4.29622726385596,-5.23156938308663,78.4160333679838));
#28185=CARTESIAN_POINT('Ctrl Pts',(4.4384576309191,-5.11145583677338,78.4247827806471));
#28186=CARTESIAN_POINT('Ctrl Pts',(4.57549970660809,-4.98568866204352,78.4335321933104));
#28187=CARTESIAN_POINT('Ctrl Pts',(4.71254069815148,-4.85992248226304,78.4422815367568));
#28188=CARTESIAN_POINT('Ctrl Pts',(4.84439326931173,-4.72850295734146,78.4510308802031));
#28189=CARTESIAN_POINT('Ctrl Pts',(4.97060959434564,-4.59187644221827,78.4597802236494));
#28190=CARTESIAN_POINT('Ctrl Pts',(5.0968249628039,-4.45525096256808,78.4685295007857));
#28191=CARTESIAN_POINT('Ctrl Pts',(5.21740397615722,-4.31341878218468,78.477278777922));
#28192=CARTESIAN_POINT('Ctrl Pts',(5.33193710451825,-4.16686161438817,78.4860280550583));
#28193=CARTESIAN_POINT('Ctrl Pts',(5.44646940289274,-4.02030550864661,78.4947772687913));
#28194=CARTESIAN_POINT('Ctrl Pts',(5.55495572749557,-3.86902470980288,78.5035264825242));
#28195=CARTESIAN_POINT('Ctrl Pts',(5.65702762491349,-3.71353301465944,78.5122756962572));
#28196=CARTESIAN_POINT('Ctrl Pts',(5.75909881655046,-3.55804239467067,78.5210248494933));
#28197=CARTESIAN_POINT('Ctrl Pts',(5.85475551250674,-3.39834117619739,78.5297740027294));
#28198=CARTESIAN_POINT('Ctrl Pts',(5.94367283727987,-3.23497174692167,78.5385231559655));
#28199=CARTESIAN_POINT('Ctrl Pts',(6.03258957676211,-3.07160339301163,78.5472722516111));
#28200=CARTESIAN_POINT('Ctrl Pts',(6.11476689685191,-2.904567128297,78.5560213472566));
#28201=CARTESIAN_POINT('Ctrl Pts',(6.18992570525175,-2.734430244761,78.5647704429021));
#28202=CARTESIAN_POINT('Ctrl Pts',(6.26508404388619,-2.56429442463221,78.5735194838632));
#28203=CARTESIAN_POINT('Ctrl Pts',(6.33322384283244,-2.3910582865618,78.5822685248242));
#28204=CARTESIAN_POINT('Ctrl Pts',(6.39411368719969,-2.21531017132265,78.5910175657852));
#28205=CARTESIAN_POINT('Ctrl Pts',(6.45500317120838,-2.03956309619679,78.5997665549676));
#28206=CARTESIAN_POINT('Ctrl Pts',(6.50864269270032,-1.86130434438778,78.6085155441501));
#28207=CARTESIAN_POINT('Ctrl Pts',(6.55485008446302,-1.68113930720069,78.6172645333325));
#28208=CARTESIAN_POINT('Ctrl Pts',(6.60199664749377,-1.4973123921196,78.6261913468618));
#28209=CARTESIAN_POINT('Ctrl Pts',(6.64140563640884,-1.31150116499787,78.6351181603912));
#28210=CARTESIAN_POINT('Ctrl Pts',(6.67293772282154,-1.12436255155771,78.6440449739206));
#28211=CARTESIAN_POINT('Ctrl Pts',(6.70384494949854,-0.94093239505252,78.6527948880761));
#28212=CARTESIAN_POINT('Ctrl Pts',(6.72718449348916,-0.756227260507957,
78.6615448022316));
#28213=CARTESIAN_POINT('Ctrl Pts',(6.74287707373921,-0.570874564542999,
78.6702947163872));
#28214=CARTESIAN_POINT('Ctrl Pts',(6.75856934538663,-0.38552551363374,78.6790444584711));
#28215=CARTESIAN_POINT('Ctrl Pts',(6.766614930041,-0.19952921241945,78.6877942005551));
#28216=CARTESIAN_POINT('Ctrl Pts',(6.76698649908906,-0.0135174386016032,
78.6965439426391));
#28217=CARTESIAN_POINT('Ctrl Pts',(6.76735806132392,0.172490924444679,78.705293524285));
#28218=CARTESIAN_POINT('Ctrl Pts',(6.76005588896295,0.358514472900385,78.7140431059309));
#28219=CARTESIAN_POINT('Ctrl Pts',(6.74510478454592,0.543921359661268,78.7227926875768));
#28220=CARTESIAN_POINT('Ctrl Pts',(6.73015393440698,0.729325093149558,78.7315421204158));
#28221=CARTESIAN_POINT('Ctrl Pts',(6.70755443556909,0.914111900255522,78.7402915532549));
#28222=CARTESIAN_POINT('Ctrl Pts',(6.67738304682331,1.09765415591461,78.7490409860939));
#28223=CARTESIAN_POINT('Ctrl Pts',(6.64721213111874,1.28119353391204,78.7577902817553));
#28224=CARTESIAN_POINT('Ctrl Pts',(6.60946960955508,1.46348811672592,78.7665395774166));
#28225=CARTESIAN_POINT('Ctrl Pts',(6.56428366991196,1.64391876348169,78.7752888730779));
#28226=CARTESIAN_POINT('Ctrl Pts',(6.51909837867733,1.8243468210966,78.7840380431888));
#28227=CARTESIAN_POINT('Ctrl Pts',(6.46646995271939,2.00291071820387,78.7927872132996));
#28228=CARTESIAN_POINT('Ctrl Pts',(6.40657713281569,2.17900400212644,78.8015363834104));
#28229=CARTESIAN_POINT('Ctrl Pts',(6.34668509279078,2.3550949930961,78.8102854395962));
#28230=CARTESIAN_POINT('Ctrl Pts',(6.27952894037541,2.52871516398086,78.819034495782));
#28231=CARTESIAN_POINT('Ctrl Pts',(6.20533675061458,2.69927486771394,78.8277835519678));
#28232=CARTESIAN_POINT('Ctrl Pts',(6.12832117907928,2.87632521635899,78.83686555325));
#28233=CARTESIAN_POINT('Ctrl Pts',(6.04372366626091,3.05007728919975,78.8459475545323));
#28234=CARTESIAN_POINT('Ctrl Pts',(5.95185378007879,3.21989527478174,78.8550295558146));
#28235=CARTESIAN_POINT('Ctrl Pts',(5.86334450817379,3.38350129286738,78.8637793361217));
#28236=CARTESIAN_POINT('Ctrl Pts',(5.7680856205726,3.54345567124955,78.8725291164288));
#28237=CARTESIAN_POINT('Ctrl Pts',(5.66640068804484,3.69921508465309,78.8812788967359));
#28238=CARTESIAN_POINT('Ctrl Pts',(5.5647194110792,3.85496889852288,78.8900283624894));
#28239=CARTESIAN_POINT('Ctrl Pts',(5.45661270815107,4.00652780919646,78.8987778282429));
#28240=CARTESIAN_POINT('Ctrl Pts',(5.34244776449103,4.15337704569243,78.9075272939964));
#28241=CARTESIAN_POINT('Ctrl Pts',(5.22828631819585,4.30022178356262,78.916276491716));
#28242=CARTESIAN_POINT('Ctrl Pts',(5.1080671784406,4.4423569097269,78.9250256894356));
#28243=CARTESIAN_POINT('Ctrl Pts',(4.98219864544711,4.57929969070654,78.9337748871552));
#28244=CARTESIAN_POINT('Ctrl Pts',(4.85633329944008,4.71623900430018,78.9425238633454));
#28245=CARTESIAN_POINT('Ctrl Pts',(4.72481904033624,4.84798602483641,78.9512728395357));
#28246=CARTESIAN_POINT('Ctrl Pts',(4.58810250737165,4.97409332259156,78.9600218157259));
#28247=CARTESIAN_POINT('Ctrl Pts',(4.45137708685612,5.10020881822161,78.9687713606621));
#28248=CARTESIAN_POINT('Ctrl Pts',(4.30944892636025,5.22068366307955,78.9775209055983));
#28249=CARTESIAN_POINT('Ctrl Pts',(4.16280009466638,5.33510865604868,78.9862704505344));
#28250=CARTESIAN_POINT('Ctrl Pts',(4.01615988348763,5.44952692272911,78.9950194811427));
#28251=CARTESIAN_POINT('Ctrl Pts',(3.86479978232201,5.55789587288647,79.003768511751));
#28252=CARTESIAN_POINT('Ctrl Pts',(3.70923383581034,5.659847467139,79.0125175423593));
#28253=CARTESIAN_POINT('Ctrl Pts',(3.55366577799509,5.76180044505402,79.0212666917073));
#28254=CARTESIAN_POINT('Ctrl Pts',(3.39389200026811,5.85733573571076,79.0300158410553));
#28255=CARTESIAN_POINT('Ctrl Pts',(3.23045513626015,5.94612887621942,79.0387649904033));
#28256=CARTESIAN_POINT('Ctrl Pts',(3.18695122151563,5.96976399206696,79.0410938545163));
#28257=CARTESIAN_POINT('Ctrl Pts',(3.1431879126266,5.99292165435335,79.0434227186292));
#28258=CARTESIAN_POINT('Ctrl Pts',(3.09917575053266,6.01559628526635,79.0457515827422));
#28259=CARTESIAN_POINT('Ctrl Pts',(3.09917575053268,6.01559628526634,77.0459357433347));
#28260=CARTESIAN_POINT('Ctrl Pts',(2.94459599297447,6.09523424855869,77.0541212456873));
#28261=CARTESIAN_POINT('Ctrl Pts',(2.78680153118066,6.16898384532002,77.0623067480399));
#28262=CARTESIAN_POINT('Ctrl Pts',(2.62628284950005,6.23657978337662,77.0704922503925));
#28263=CARTESIAN_POINT('Ctrl Pts',(2.46587183064077,6.30413038359885,77.0786722625786));
#28264=CARTESIAN_POINT('Ctrl Pts',(2.30274056247645,6.3655354062191,77.0868522747648));
#28265=CARTESIAN_POINT('Ctrl Pts',(2.13740267681911,6.4205762044482,77.095032286951));
#28266=CARTESIAN_POINT('Ctrl Pts',(1.97214201399145,6.4755912952832,77.1032084785748));
#28267=CARTESIAN_POINT('Ctrl Pts',(1.80467712843983,6.5242479695393,77.1113846701988));
#28268=CARTESIAN_POINT('Ctrl Pts',(1.63554016630024,6.56637627344174,77.1195608618226));
#28269=CARTESIAN_POINT('Ctrl Pts',(1.4664221967583,6.60849984670508,77.1277361353319));
#28270=CARTESIAN_POINT('Ctrl Pts',(1.29563287264218,6.64409641530863,77.1359114088412));
#28271=CARTESIAN_POINT('Ctrl Pts',(1.12371828957322,6.67304624633148,77.1440866823505));
#28272=CARTESIAN_POINT('Ctrl Pts',(0.951806553853321,6.70199559787043,77.1522618204561));
#28273=CARTESIAN_POINT('Ctrl Pts',(0.778769952066066,6.72429837035717,77.1604369585617));
#28274=CARTESIAN_POINT('Ctrl Pts',(0.605163411855234,6.73988621899152,77.1686120966674));
#28275=CARTESIAN_POINT('Ctrl Pts',(0.4315277147346,6.75547668557733,77.176788607773));
#28276=CARTESIAN_POINT('Ctrl Pts',(0.257322247994863,6.7643499497148,77.1849651188785));
#28277=CARTESIAN_POINT('Ctrl Pts',(0.083105707101584,6.76648966905641,77.1931416299841));
#28278=CARTESIAN_POINT('Ctrl Pts',(-0.0911722384356991,6.76863014256697,
77.201321022996));
#28279=CARTESIAN_POINT('Ctrl Pts',(-0.265460905273268,6.76403233996544,
77.2095004160079));
#28280=CARTESIAN_POINT('Ctrl Pts',(-0.439202930077307,6.7527320238709,77.2176798090198));
#28281=CARTESIAN_POINT('Ctrl Pts',(-0.613132562637829,6.74141950562231,
77.2258680341929));
#28282=CARTESIAN_POINT('Ctrl Pts',(-0.786514013848733,6.72339004167877,
77.234056259366));
#28283=CARTESIAN_POINT('Ctrl Pts',(-0.958795441472268,6.69873124564734,
77.2422444845391));
#28284=CARTESIAN_POINT('Ctrl Pts',(-1.13117954412829,6.67405775364596,77.2504375896711));
#28285=CARTESIAN_POINT('Ctrl Pts',(-1.30246196237958,6.64274711990887,77.2586306948031));
#28286=CARTESIAN_POINT('Ctrl Pts',(-1.47210251455571,6.60493778824894,77.2668237999351));
#28287=CARTESIAN_POINT('Ctrl Pts',(-1.64198104633278,6.56707541591244,77.2750283987334));
#28288=CARTESIAN_POINT('Ctrl Pts',(-1.81021276293874,6.52269622631456,77.2832329975316));
#28289=CARTESIAN_POINT('Ctrl Pts',(-1.97627306419992,6.47198839428177,77.2914375963299));
#28290=CARTESIAN_POINT('Ctrl Pts',(-2.07599484862549,6.44153755530184,77.296364585059));
#28291=CARTESIAN_POINT('Ctrl Pts',(-2.17493394727849,6.40880542593423,77.301291573788));
#28292=CARTESIAN_POINT('Ctrl Pts',(-2.27298060169066,6.37384092869739,77.3062185625171));
#28293=CARTESIAN_POINT('Ctrl Pts',(-2.43661332190611,6.31548773114942,77.314441347609));
#28294=CARTESIAN_POINT('Ctrl Pts',(-2.59822931702284,6.25074650535034,77.3226641327008));
#28295=CARTESIAN_POINT('Ctrl Pts',(-2.75729380899212,6.17977506474902,77.3308869177927));
#28296=CARTESIAN_POINT('Ctrl Pts',(-2.91617773354826,6.10888418976783,77.3391003685132));
#28297=CARTESIAN_POINT('Ctrl Pts',(-3.07251559759457,6.03177732774177,77.3473138192338));
#28298=CARTESIAN_POINT('Ctrl Pts',(-3.22578865161336,5.94866174657145,77.3555272699543));
#28299=CARTESIAN_POINT('Ctrl Pts',(-3.37891855779665,5.8656237903667,77.3637330498047));
#28300=CARTESIAN_POINT('Ctrl Pts',(-3.52898904074577,5.77658846088174,77.3719388296551));
#28301=CARTESIAN_POINT('Ctrl Pts',(-3.6755021087829,5.68181073675747,77.3801446095055));
#28302=CARTESIAN_POINT('Ctrl Pts',(-3.82190781754906,5.58710246218812,77.3883443764688));
#28303=CARTESIAN_POINT('Ctrl Pts',(-3.96476100329072,5.48666036821466,77.396544143432));
#28304=CARTESIAN_POINT('Ctrl Pts',(-4.10358896683244,5.38078494192911,77.4047439103953));
#28305=CARTESIAN_POINT('Ctrl Pts',(-4.24234312501469,5.2749658023865,77.4129393181017));
#28306=CARTESIAN_POINT('Ctrl Pts',(-4.37707603927068,5.16371930204179,77.4211347258082));
#28307=CARTESIAN_POINT('Ctrl Pts',(-4.50734459841955,5.04738879729887,77.4293301335146));
#28308=CARTESIAN_POINT('Ctrl Pts',(-4.63758693772306,4.93108170701501,77.4375238916877));
#28309=CARTESIAN_POINT('Ctrl Pts',(-4.76336644023871,4.80969288494777,77.4457176498609));
#28310=CARTESIAN_POINT('Ctrl Pts',(-4.8842734404309,4.68360565794147,77.453911408034));
#28311=CARTESIAN_POINT('Ctrl Pts',(-5.00517072295319,4.55752856495593,77.4621045076495));
#28312=CARTESIAN_POINT('Ctrl Pts',(-5.12119603392262,4.42675407760548,77.4702976072649));
#28313=CARTESIAN_POINT('Ctrl Pts',(-5.23197696954709,4.29170199223209,77.4784907068804));
#28314=CARTESIAN_POINT('Ctrl Pts',(-5.34276918852648,4.1566361514178,77.4866846409864));
#28315=CARTESIAN_POINT('Ctrl Pts',(-5.44831574020577,4.01729212222537,77.4948785750925));
#28316=CARTESIAN_POINT('Ctrl Pts',(-5.54828485420199,3.87412237502028,77.5030725091986));
#28317=CARTESIAN_POINT('Ctrl Pts',(-5.64828236738323,3.73091195621196,77.5112687710341));
#28318=CARTESIAN_POINT('Ctrl Pts',(-5.74269908143153,3.58387394896211,77.5194650328696));
#28319=CARTESIAN_POINT('Ctrl Pts',(-5.83124683478272,3.43348938426151,77.5276612947051));
#28320=CARTESIAN_POINT('Ctrl Pts',(-5.91988642150887,3.28294885487978,77.5358660569301));
#28321=CARTESIAN_POINT('Ctrl Pts',(-6.0026447046072,3.12905514378719,77.544070819155));
#28322=CARTESIAN_POINT('Ctrl Pts',(-6.07927927952005,2.97231432415857,77.5522755813799));
#28323=CARTESIAN_POINT('Ctrl Pts',(-6.15595455676992,2.81549025597441,77.5604847013376));
#28324=CARTESIAN_POINT('Ctrl Pts',(-6.2264994970635,2.65581639285271,77.5686938212953));
#28325=CARTESIAN_POINT('Ctrl Pts',(-6.29072012717906,2.49381821340374,77.576902941253));
#28326=CARTESIAN_POINT('Ctrl Pts',(-6.35503500880818,2.33158228210496,77.5851241090835));
#28327=CARTESIAN_POINT('Ctrl Pts',(-6.41300691173094,2.16701555591936,77.593345276914));
#28328=CARTESIAN_POINT('Ctrl Pts',(-6.46449157378496,2.00065931444194,77.6015664447444));
#28329=CARTESIAN_POINT('Ctrl Pts',(-6.51226066621631,1.84630874946532,77.6091943034177));
#28330=CARTESIAN_POINT('Ctrl Pts',(-6.55444556182836,1.69041800057974,77.6168221620909));
#28331=CARTESIAN_POINT('Ctrl Pts',(-6.59097066947956,1.53342578368182,77.6244500207641));
#28332=CARTESIAN_POINT('Ctrl Pts',(-6.64384035882495,1.30618128610771,77.635491261827));
#28333=CARTESIAN_POINT('Ctrl Pts',(-6.68498080346422,1.07608419429346,77.6465325028899));
#28334=CARTESIAN_POINT('Ctrl Pts',(-6.71413982814934,0.844165486180697,
77.6575737439527));
#28335=CARTESIAN_POINT('Ctrl Pts',(-6.74253161918314,0.618349034201611,
77.668324467353));
#28336=CARTESIAN_POINT('Ctrl Pts',(-6.75956428101389,0.390805215452577,
77.6790751907532));
#28337=CARTESIAN_POINT('Ctrl Pts',(-6.7650483845779,0.162509551473162,77.6898259141535));
#28338=CARTESIAN_POINT('Ctrl Pts',(-6.76629882392945,0.110455486721055,
77.692277204039));
#28339=CARTESIAN_POINT('Ctrl Pts',(-6.766949042737,0.0583624462839173,77.6947284939244));
#28340=CARTESIAN_POINT('Ctrl Pts',(-6.76699712094732,0.00624220238653553,
77.6971797838099));
#28341=CARTESIAN_POINT('',(-6.767,3.76644462146691E-12,77.3028202161898));
#28342=CARTESIAN_POINT('Ctrl Pts',(3.09917575053257,6.0155962852664,76.6515786160344));
#28343=CARTESIAN_POINT('Ctrl Pts',(2.94447999371585,6.09529401023024,76.6597677554965));
#28344=CARTESIAN_POINT('Ctrl Pts',(2.78657234059765,6.16909059992118,76.6679568949587));
#28345=CARTESIAN_POINT('Ctrl Pts',(2.6259447762783,6.2367221384263,76.6761460344209));
#28346=CARTESIAN_POINT('Ctrl Pts',(2.46541858317967,6.30431099501909,76.6843300057597));
#28347=CARTESIAN_POINT('Ctrl Pts',(2.30217622891919,6.36574241074283,76.6925139770985));
#28348=CARTESIAN_POINT('Ctrl Pts',(2.13673265208952,6.42079921610188,76.7006979484374));
#28349=CARTESIAN_POINT('Ctrl Pts',(1.97135990103597,6.47583245184858,76.7088784162487));
#28350=CARTESIAN_POINT('Ctrl Pts',(1.80378814606259,6.52449640038739,76.71705888406));
#28351=CARTESIAN_POINT('Ctrl Pts',(1.63455064267454,6.56662266287109,76.7252393518714));
#28352=CARTESIAN_POINT('Ctrl Pts',(1.46532381932214,6.60874626690159,76.7334193034396));
#28353=CARTESIAN_POINT('Ctrl Pts',(1.29443180442709,6.64433291168642,76.7415992550078));
#28354=CARTESIAN_POINT('Ctrl Pts',(1.12242162302429,6.67326447101923,76.7497792065761));
#28355=CARTESIAN_POINT('Ctrl Pts',(0.950408413126966,6.70219653973508,76.7579593021645));
#28356=CARTESIAN_POINT('Ctrl Pts',(0.777277352866236,6.72447322915449,76.766139397753));
#28357=CARTESIAN_POINT('Ctrl Pts',(0.603584097146813,6.74002783656503,76.7743194933414));
#28358=CARTESIAN_POINT('Ctrl Pts',(0.429855836852966,6.75558557871106,76.7825012374727));
#28359=CARTESIAN_POINT('Ctrl Pts',(0.255565514406007,6.76441850834548,76.7906829816039));
#28360=CARTESIAN_POINT('Ctrl Pts',(0.0812723540308919,6.76651193780594,
76.7988647257352));
#28361=CARTESIAN_POINT('Ctrl Pts',(-0.0930879890354412,6.76860617419551,
76.807049623585));
#28362=CARTESIAN_POINT('Ctrl Pts',(-0.267450812114449,6.76395573194799,
76.8152345214349));
#28363=CARTESIAN_POINT('Ctrl Pts',(-0.441258415564034,6.75259801933255,
76.8234194192848));
#28364=CARTESIAN_POINT('Ctrl Pts',(-0.615256595147889,6.74122785324028,
76.8316132916914));
#28365=CARTESIAN_POINT('Ctrl Pts',(-0.788697979502679,6.72313575241151,
76.839807164098));
#28366=CARTESIAN_POINT('Ctrl Pts',(-0.961030600080398,6.69841094482185,
76.8480010365045));
#28367=CARTESIAN_POINT('Ctrl Pts',(-1.1334708175112,6.67367070015776,76.856200024802));
#28368=CARTESIAN_POINT('Ctrl Pts',(-1.3048005379438,6.64228956004986,76.8643990130995));
#28369=CARTESIAN_POINT('Ctrl Pts',(-1.47447963245551,6.60440752933023,76.872598001397));
#28370=CARTESIAN_POINT('Ctrl Pts',(-1.64439086219489,6.56647367281645,76.8808082065978));
#28371=CARTESIAN_POINT('Ctrl Pts',(-1.81264660864914,6.5220212548482,76.8890184117987));
#28372=CARTESIAN_POINT('Ctrl Pts',(-1.97872258860794,6.47123990571612,76.8972286169996));
#28373=CARTESIAN_POINT('Ctrl Pts',(-2.05377599510466,6.44829069150821,76.9009389902187));
#28374=CARTESIAN_POINT('Ctrl Pts',(-2.12838449552966,6.42404954884372,76.9046493634377));
#28375=CARTESIAN_POINT('Ctrl Pts',(-2.2025011858424,6.39853713956267,76.9083597366568));
#28376=CARTESIAN_POINT('Ctrl Pts',(-2.36615894309163,6.34220294995783,76.9165526464727));
#28377=CARTESIAN_POINT('Ctrl Pts',(-2.52789770493843,6.27950189926979,76.9247455562885));
#28378=CARTESIAN_POINT('Ctrl Pts',(-2.68718362870622,6.21058235156843,76.9329384661044));
#28379=CARTESIAN_POINT('Ctrl Pts',(-2.8462856811994,6.14174236096027,76.9411219184571));
#28380=CARTESIAN_POINT('Ctrl Pts',(-3.00294020397036,6.06669830728647,76.9493053708098));
#28381=CARTESIAN_POINT('Ctrl Pts',(-3.15662855968243,5.9856482636551,76.9574888231624));
#28382=CARTESIAN_POINT('Ctrl Pts',(-3.31017106484937,5.90467513667099,76.965664509403));
#28383=CARTESIAN_POINT('Ctrl Pts',(-3.46075269009441,5.81770753676374,76.9738401956437));
#28384=CARTESIAN_POINT('Ctrl Pts',(-3.60787479708822,5.72499156755149,76.9820158818843));
#28385=CARTESIAN_POINT('Ctrl Pts',(-3.75488748420434,5.6323445544616,76.9901854875799));
#28386=CARTESIAN_POINT('Ctrl Pts',(-3.8984454723192,5.53395787845469,76.9983550932755));
#28387=CARTESIAN_POINT('Ctrl Pts',(-4.03807472580735,5.43012352610839,77.0065246989712));
#28388=CARTESIAN_POINT('Ctrl Pts',(-4.17762878587552,5.32634509084158,77.0146899051547));
#28389=CARTESIAN_POINT('Ctrl Pts',(-4.3132580358509,5.21712503821022,77.0228551113383));
#28390=CARTESIAN_POINT('Ctrl Pts',(-4.44451741051006,5.10279864267374,77.0310203175218));
#28391=CARTESIAN_POINT('Ctrl Pts',(-4.57575070407425,4.9884949636677,77.0391839012878));
#28392=CARTESIAN_POINT('Ctrl Pts',(-4.70261557471194,4.86908719503985,77.0473474850537));
#28393=CARTESIAN_POINT('Ctrl Pts',(-4.82469985157451,4.74495103686191,77.0555110688196));
#28394=CARTESIAN_POINT('Ctrl Pts',(-4.94677460385563,4.62082456334592,77.0636740156918));
#28395=CARTESIAN_POINT('Ctrl Pts',(-5.06406925049367,4.49197069223053,77.071836962564));
#28396=CARTESIAN_POINT('Ctrl Pts',(-5.17620841174312,4.3588020691699,77.0799999094361));
#28397=CARTESIAN_POINT('Ctrl Pts',(-5.28835967056454,4.22561907987909,77.0881637369269));
#28398=CARTESIAN_POINT('Ctrl Pts',(-5.39535410282002,4.08812068833179,77.0963275644177));
#28399=CARTESIAN_POINT('Ctrl Pts',(-5.49685656544128,3.94675270304146,77.1044913919085));
#28400=CARTESIAN_POINT('Ctrl Pts',(-5.59838884747007,3.80534318664484,77.1126576177697));
#28401=CARTESIAN_POINT('Ctrl Pts',(-5.69442573548572,3.66006210641259,77.1208238436309));
#28402=CARTESIAN_POINT('Ctrl Pts',(-5.78467536991784,3.51138432312185,77.1289900694921));
#28403=CARTESIAN_POINT('Ctrl Pts',(-5.87502156397725,3.36254746692816,77.1371650325379));
#28404=CARTESIAN_POINT('Ctrl Pts',(-5.95956794621117,3.210306957146,77.1453399955838));
#28405=CARTESIAN_POINT('Ctrl Pts',(-6.03806813568016,3.05516320167743,77.1535149586297));
#28406=CARTESIAN_POINT('Ctrl Pts',(-6.11661113729133,2.89993483448296,77.1616943801066));
#28407=CARTESIAN_POINT('Ctrl Pts',(-6.1891012231642,2.74180039441464,77.1698738015835));
#28408=CARTESIAN_POINT('Ctrl Pts',(-6.2553402552646,2.58128016512471,77.1780532230604));
#28409=CARTESIAN_POINT('Ctrl Pts',(-6.32167987821284,2.42051616919978,77.186245065838));
#28410=CARTESIAN_POINT('Ctrl Pts',(-6.38174935182926,2.25735948336676,77.1944369086158));
#28411=CARTESIAN_POINT('Ctrl Pts',(-6.43540009344285,2.09234668191381,77.2026287513934));
#28412=CARTESIAN_POINT('Ctrl Pts',(-6.48677735071721,1.93432640299816,77.2104734596171));
#28413=CARTESIAN_POINT('Ctrl Pts',(-6.53226863502543,1.77460434834334,77.2183181678407));
#28414=CARTESIAN_POINT('Ctrl Pts',(-6.57178766936335,1.6136591426952,77.2261628760644));
#28415=CARTESIAN_POINT('Ctrl Pts',(-6.62724690738091,1.38779586902559,77.237171787285));
#28416=CARTESIAN_POINT('Ctrl Pts',(-6.67107997133574,1.15898350456572,77.2481806985057));
#28417=CARTESIAN_POINT('Ctrl Pts',(-6.70303305923548,0.928243937117981,
77.2591896097263));
#28418=CARTESIAN_POINT('Ctrl Pts',(-6.73420260589151,0.703162475960873,
77.2699285646906));
#28419=CARTESIAN_POINT('Ctrl Pts',(-6.75406775022714,0.476246829645958,
77.2806675196549));
#28420=CARTESIAN_POINT('Ctrl Pts',(-6.76243688553776,0.248468044461097,
77.2914064746192));
#28421=CARTESIAN_POINT('Ctrl Pts',(-6.76540188998257,0.16777092517219,77.2952110551427));
#28422=CARTESIAN_POINT('Ctrl Pts',(-6.76692439875737,0.0869657043062816,
77.2990156356663));
#28423=CARTESIAN_POINT('Ctrl Pts',(-6.76699725388582,0.00609638431824338,
77.3028202161898));
#28424=CARTESIAN_POINT('Ctrl Pts',(-6.767,3.76644436666148E-12,77.3028202161898));
#28425=CARTESIAN_POINT('Ctrl Pts',(-6.76700000000011,-0.186007249411994,
77.3115697279958));
#28426=CARTESIAN_POINT('Ctrl Pts',(-6.75932637295458,-0.372014355523931,
77.3203192398017));
#28427=CARTESIAN_POINT('Ctrl Pts',(-6.74400518266957,-0.557389537151535,
77.3290687516077));
#28428=CARTESIAN_POINT('Ctrl Pts',(-6.72868405709682,-0.742763935808111,
77.3378182264582));
#28429=CARTESIAN_POINT('Ctrl Pts',(-6.70571545653034,-0.927506129691979,
77.3465677013088));
#28430=CARTESIAN_POINT('Ctrl Pts',(-6.67517739415697,-1.11098863924693,
77.3553171761593));
#28431=CARTESIAN_POINT('Ctrl Pts',(-6.64463945823122,-1.29447038906391,
77.3640666147813));
#28432=CARTESIAN_POINT('Ctrl Pts',(-6.60653217027181,-1.47669218228113,
77.3728160534033));
#28433=CARTESIAN_POINT('Ctrl Pts',(-6.56098496116736,-1.65703510504025,
77.3815654920253));
#28434=CARTESIAN_POINT('Ctrl Pts',(-6.5154379368754,-1.83737729603941,77.3903148951455));
#28435=CARTESIAN_POINT('Ctrl Pts',(-6.46245112202659,-2.01584035396991,
77.3990642982658));
#28436=CARTESIAN_POINT('Ctrl Pts',(-6.40220448416258,-2.19181813638097,
77.407813701386));
#28437=CARTESIAN_POINT('Ctrl Pts',(-6.34195808575201,-2.36779521935908,
77.4165630697313));
#28438=CARTESIAN_POINT('Ctrl Pts',(-6.27445201489246,-2.54128677544801,
77.4253124380766));
#28439=CARTESIAN_POINT('Ctrl Pts',(-6.19991555136191,-2.71170355237824,
77.4340618064218));
#28440=CARTESIAN_POINT('Ctrl Pts',(-6.12537937789048,-2.88211966613052,
77.4428111407189));
#28441=CARTESIAN_POINT('Ctrl Pts',(-6.04381298133629,-3.04946076210421,
77.451560475016));
#28442=CARTESIAN_POINT('Ctrl Pts',(-5.95549339426321,-3.21315848206827,
77.460309809313));
#28443=CARTESIAN_POINT('Ctrl Pts',(-5.86717414355184,-3.37685557859595,
77.4690591102886));
#28444=CARTESIAN_POINT('Ctrl Pts',(-5.7721018898627,-3.53690907467258,77.4778084112641));
#28445=CARTESIAN_POINT('Ctrl Pts',(-5.67059953467111,-3.69277536784839,
77.4865577122397));
#28446=CARTESIAN_POINT('Ctrl Pts',(-5.56909755761813,-3.84864108035724,
77.4953069806204));
#28447=CARTESIAN_POINT('Ctrl Pts',(-5.46116568338122,-4.00031938104207,
77.5040562490012));
#28448=CARTESIAN_POINT('Ctrl Pts',(-5.34717048686172,-4.14729511663144,
77.5128055173819));
#28449=CARTESIAN_POINT('Ctrl Pts',(-5.2331757055557,-4.29427031687977,77.5215547538946));
#28450=CARTESIAN_POINT('Ctrl Pts',(-5.11311782178851,-4.43654275987077,
77.5303039904072));
#28451=CARTESIAN_POINT('Ctrl Pts',(-4.98740459172053,-4.57362924147608,
77.5390532269198));
#28452=CARTESIAN_POINT('Ctrl Pts',(-4.86169180910883,-4.71071523514381,
77.5478024322909));
#28453=CARTESIAN_POINT('Ctrl Pts',(-4.730323914155,-4.84261509316456,77.556551637662));
#28454=CARTESIAN_POINT('Ctrl Pts',(-4.59374707237378,-4.96888084331445,
77.5653008430331));
#28455=CARTESIAN_POINT('Ctrl Pts',(-4.45717070537482,-5.09514615452655,
77.5740500179894));
#28456=CARTESIAN_POINT('Ctrl Pts',(-4.31538563819583,-5.21577720253572,
77.5827991929456));
#28457=CARTESIAN_POINT('Ctrl Pts',(-4.16887341290716,-5.33036429028597,
77.5915483679019));
#28458=CARTESIAN_POINT('Ctrl Pts',(-4.02236168477423,-5.44495098921114,
77.6002975131698));
#28459=CARTESIAN_POINT('Ctrl Pts',(-3.87112305634541,-5.55349359238687,
77.6090466584377));
#28460=CARTESIAN_POINT('Ctrl Pts',(-3.71567117316853,-5.65562346102394,
77.6177958037056));
#28461=CARTESIAN_POINT('Ctrl Pts',(-3.56021980457443,-5.75775299158681,
77.6265449200117));
#28462=CARTESIAN_POINT('Ctrl Pts',(-3.40055544862552,-5.85346967275257,
77.6352940363179));
#28463=CARTESIAN_POINT('Ctrl Pts',(-3.23722036323591,-5.94244842803459,
77.644043152624));
#28464=CARTESIAN_POINT('Ctrl Pts',(-3.07388580496244,-6.03142689616374,
77.652792240695));
#28465=CARTESIAN_POINT('Ctrl Pts',(-2.90688079257915,-6.11366734484723,
77.6615413287659));
#28466=CARTESIAN_POINT('Ctrl Pts',(-2.73677251094833,-6.18889046787205,
77.6702904168369));
#28467=CARTESIAN_POINT('Ctrl Pts',(-2.56666476416886,-6.26411335438171,
77.6790394773991));
#28468=CARTESIAN_POINT('Ctrl Pts',(-2.39345402972357,-6.3323188435019,77.6877885379613));
#28469=CARTESIAN_POINT('Ctrl Pts',(-2.21772856474325,-6.39327529620944,
77.6965375985235));
#28470=CARTESIAN_POINT('Ctrl Pts',(-2.04200363768559,-6.4542315623199,77.7052866323035));
#28471=CARTESIAN_POINT('Ctrl Pts',(-1.86376426620386,-6.50793874251972,
77.7140356660835));
#28472=CARTESIAN_POINT('Ctrl Pts',(-1.68361578194983,-6.55421443796047,
77.7227846998635));
#28473=CARTESIAN_POINT('Ctrl Pts',(-1.50346783420193,-6.60048999558605,
77.7315337075877));
#28474=CARTESIAN_POINT('Ctrl Pts',(-1.32141106257603,-6.63933404145424,
77.7402827153119));
#28475=CARTESIAN_POINT('Ctrl Pts',(-1.13806375959431,-6.67061465526964,
77.7490317230362));
#28476=CARTESIAN_POINT('Ctrl Pts',(-0.954716987423268,-6.70189517852421,
77.757780705431));
#28477=CARTESIAN_POINT('Ctrl Pts',(-0.770079973814236,-6.72561226535777,
77.7665296878259));
#28478=CARTESIAN_POINT('Ctrl Pts',(-0.584779770557059,-6.74168536939742,
77.7752786702208));
#28479=CARTESIAN_POINT('Ctrl Pts',(-0.391490647558487,-6.75845143942367,
77.7844048508968));
#28480=CARTESIAN_POINT('Ctrl Pts',(-0.197480213108879,-6.76689975924013,
77.7935310315729));
#28481=CARTESIAN_POINT('Ctrl Pts',(-0.00346532630230147,-6.76699911271707,
77.8026572122489));
#28482=CARTESIAN_POINT('Ctrl Pts',(0.184486595291538,-6.76709536139786,
77.8114981997789));
#28483=CARTESIAN_POINT('Ctrl Pts',(0.372442378180706,-6.75935659726795,
77.8203391873088));
#28484=CARTESIAN_POINT('Ctrl Pts',(0.559750217717562,-6.74380965729054,
77.8291801748387));
#28485=CARTESIAN_POINT('Ctrl Pts',(0.745129914453265,-6.72842275717303,
77.8379301534365));
#28486=CARTESIAN_POINT('Ctrl Pts',(0.929874656309734,-6.70538772273535,
77.8466801320343));
#28487=CARTESIAN_POINT('Ctrl Pts',(1.11335688289337,-6.67478280180816,77.855430110632));
#28488=CARTESIAN_POINT('Ctrl Pts',(1.29683723118408,-6.64417819418111,77.864179999657));
#28489=CARTESIAN_POINT('Ctrl Pts',(1.47905480729778,-6.60600390230177,77.8729298886819));
#28490=CARTESIAN_POINT('Ctrl Pts',(1.65939064804344,-6.56038959797252,77.8816797777069));
#28491=CARTESIAN_POINT('Ctrl Pts',(1.839724702638,-6.51477574543387,77.8904295800678));
#28492=CARTESIAN_POINT('Ctrl Pts',(2.01817678125382,-6.46172209820245,77.8991793824287));
#28493=CARTESIAN_POINT('Ctrl Pts',(2.19414072347213,-6.40140886724174,77.9079291847897));
#28494=CARTESIAN_POINT('Ctrl Pts',(2.37010298131632,-6.34109621361548,77.9166789033952));
#28495=CARTESIAN_POINT('Ctrl Pts',(2.54357687926451,-6.27352420826158,77.9254286220007));
#28496=CARTESIAN_POINT('Ctrl Pts',(2.71397317789512,-6.19892237325697,77.9341783406061));
#28497=CARTESIAN_POINT('Ctrl Pts',(2.88436790206755,-6.12432122757174,77.9429279783644));
#28498=CARTESIAN_POINT('Ctrl Pts',(3.05168482125823,-6.04269049717636,77.9516776161227));
#28499=CARTESIAN_POINT('Ctrl Pts',(3.21535561996969,-5.95430745235157,77.960427253881));
#28500=CARTESIAN_POINT('Ctrl Pts',(3.37902496074868,-5.86592519481754,77.9691768137));
#28501=CARTESIAN_POINT('Ctrl Pts',(3.5390479938447,-5.7707908794048,77.977926373519));
#28502=CARTESIAN_POINT('Ctrl Pts',(3.69488118814588,-5.66922763747283,77.986675933338));
#28503=CARTESIAN_POINT('Ctrl Pts',(3.85071304610448,-5.56766526649318,77.9954254181254));
#28504=CARTESIAN_POINT('Ctrl Pts',(4.00235489705594,-5.45967423580988,78.0041749029129));
#28505=CARTESIAN_POINT('Ctrl Pts',(4.14929168607292,-5.34562133936609,78.0129243877003));
#28506=CARTESIAN_POINT('Ctrl Pts',(4.29622726385405,-5.2315693830882,78.0216738003636));
#28507=CARTESIAN_POINT('Ctrl Pts',(4.43845763091726,-5.11145583677499,78.0304232130269));
#28508=CARTESIAN_POINT('Ctrl Pts',(4.57549970660631,-4.98568866204515,78.0391726256902));
#28509=CARTESIAN_POINT('Ctrl Pts',(4.71254069814977,-4.8599224822647,78.0479219691366));
#28510=CARTESIAN_POINT('Ctrl Pts',(4.84439326931009,-4.72850295734315,78.0566713125829));
#28511=CARTESIAN_POINT('Ctrl Pts',(4.97060959434406,-4.59187644221998,78.0654206560292));
#28512=CARTESIAN_POINT('Ctrl Pts',(5.09682496280238,-4.45525096256981,78.0741699331655));
#28513=CARTESIAN_POINT('Ctrl Pts',(5.21740397615577,-4.31341878218643,78.0829192103018));
#28514=CARTESIAN_POINT('Ctrl Pts',(5.33193710451687,-4.16686161438993,78.0916684874381));
#28515=CARTESIAN_POINT('Ctrl Pts',(5.44646940289143,-4.02030550864839,78.1004177011711));
#28516=CARTESIAN_POINT('Ctrl Pts',(5.55495572749432,-3.86902470980468,78.109166914904));
#28517=CARTESIAN_POINT('Ctrl Pts',(5.65702762491231,-3.71353301466125,78.117916128637));
#28518=CARTESIAN_POINT('Ctrl Pts',(5.75909881654934,-3.55804239467248,78.1266652818731));
#28519=CARTESIAN_POINT('Ctrl Pts',(5.85475551250569,-3.3983411761992,78.1354144351092));
#28520=CARTESIAN_POINT('Ctrl Pts',(5.94367283727888,-3.23497174692349,78.1441635883453));
#28521=CARTESIAN_POINT('Ctrl Pts',(6.03258957676119,-3.07160339301345,78.1529126839909));
#28522=CARTESIAN_POINT('Ctrl Pts',(6.11476689685105,-2.90456712829882,78.1616617796364));
#28523=CARTESIAN_POINT('Ctrl Pts',(6.18992570525095,-2.73443024476281,78.1704108752819));
#28524=CARTESIAN_POINT('Ctrl Pts',(6.26508404388545,-2.56429442463402,78.179159916243));
#28525=CARTESIAN_POINT('Ctrl Pts',(6.33322384283176,-2.39105828656361,78.187908957204));
#28526=CARTESIAN_POINT('Ctrl Pts',(6.39411368719907,-2.21531017132444,78.196657998165));
#28527=CARTESIAN_POINT('Ctrl Pts',(6.45500317120774,-2.03956309619882,78.2054069873474));
#28528=CARTESIAN_POINT('Ctrl Pts',(6.50864269269967,-1.86130434439004,78.2141559765298));
#28529=CARTESIAN_POINT('Ctrl Pts',(6.55485008446237,-1.68113930720319,78.2229049657122));
#28530=CARTESIAN_POINT('Ctrl Pts',(6.6019966474932,-1.49731239212209,78.2318317792416));
#28531=CARTESIAN_POINT('Ctrl Pts',(6.64140563640835,-1.31150116500034,78.240758592771));
#28532=CARTESIAN_POINT('Ctrl Pts',(6.67293772282112,-1.12436255156017,78.2496854063004));
#28533=CARTESIAN_POINT('Ctrl Pts',(6.7038449494982,-0.940932395054963,78.2584353204559));
#28534=CARTESIAN_POINT('Ctrl Pts',(6.72718449348889,-0.756227260510381,
78.2671852346114));
#28535=CARTESIAN_POINT('Ctrl Pts',(6.74287707373901,-0.5708745645454,78.2759351487669));
#28536=CARTESIAN_POINT('Ctrl Pts',(6.75856934538649,-0.385525513636246,
78.2846848908509));
#28537=CARTESIAN_POINT('Ctrl Pts',(6.76661493004092,-0.199529212422058,
78.2934346329349));
#28538=CARTESIAN_POINT('Ctrl Pts',(6.76698649908906,-0.01351743860431,78.3021843750189));
#28539=CARTESIAN_POINT('Ctrl Pts',(6.76735806132399,0.172490924442,78.3109339566648));
#28540=CARTESIAN_POINT('Ctrl Pts',(6.76005588896309,0.358514472897737,78.3196835383107));
#28541=CARTESIAN_POINT('Ctrl Pts',(6.74510478454613,0.543921359658655,78.3284331199566));
#28542=CARTESIAN_POINT('Ctrl Pts',(6.73015393440725,0.729325093146978,78.3371825527956));
#28543=CARTESIAN_POINT('Ctrl Pts',(6.70755443556943,0.914111900252981,78.3459319856347));
#28544=CARTESIAN_POINT('Ctrl Pts',(6.67738304682373,1.09765415591211,78.3546814184737));
#28545=CARTESIAN_POINT('Ctrl Pts',(6.64721213111924,1.28119353390945,78.363430714135));
#28546=CARTESIAN_POINT('Ctrl Pts',(6.60946960955567,1.46348811672325,78.3721800097964));
#28547=CARTESIAN_POINT('Ctrl Pts',(6.56428366991265,1.64391876347894,78.3809293054577));
#28548=CARTESIAN_POINT('Ctrl Pts',(6.51909837867806,1.82434682109403,78.3896784755685));
#28549=CARTESIAN_POINT('Ctrl Pts',(6.46646995272014,2.00291071820147,78.3984276456793));
#28550=CARTESIAN_POINT('Ctrl Pts',(6.40657713281646,2.1790040021242,78.4071768157902));
#28551=CARTESIAN_POINT('Ctrl Pts',(6.34668509279168,2.35509499309367,78.4159258719759));
#28552=CARTESIAN_POINT('Ctrl Pts',(6.27952894037646,2.52871516397824,78.4246749281617));
#28553=CARTESIAN_POINT('Ctrl Pts',(6.20533675061579,2.69927486771115,78.4334239843475));
#28554=CARTESIAN_POINT('Ctrl Pts',(6.12832117908056,2.87632521635626,78.4425059856298));
#28555=CARTESIAN_POINT('Ctrl Pts',(6.04372366626226,3.05007728919708,78.451587986912));
#28556=CARTESIAN_POINT('Ctrl Pts',(5.9518537800802,3.21989527477914,78.4606699881943));
#28557=CARTESIAN_POINT('Ctrl Pts',(5.86334450817532,3.38350129286473,78.4694197685014));
#28558=CARTESIAN_POINT('Ctrl Pts',(5.76808562057425,3.54345567124686,78.4781695488086));
#28559=CARTESIAN_POINT('Ctrl Pts',(5.66640068804662,3.69921508465036,78.4869193291157));
#28560=CARTESIAN_POINT('Ctrl Pts',(5.56471941108111,3.85496889852012,78.4956687948692));
#28561=CARTESIAN_POINT('Ctrl Pts',(5.45661270815312,4.00652780919367,78.5044182606226));
#28562=CARTESIAN_POINT('Ctrl Pts',(5.34244776449322,4.15337704568962,78.5131677263761));
#28563=CARTESIAN_POINT('Ctrl Pts',(5.22828631819809,4.30022178355989,78.5219169240957));
#28564=CARTESIAN_POINT('Ctrl Pts',(5.10806717844289,4.44235690972426,78.5306661218153));
#28565=CARTESIAN_POINT('Ctrl Pts',(4.98219864544945,4.57929969070399,78.5394153195349));
#28566=CARTESIAN_POINT('Ctrl Pts',(4.8563332994424,4.71623900429781,78.5481642957252));
#28567=CARTESIAN_POINT('Ctrl Pts',(4.7248190403385,4.84798602483421,78.5569132719154));
#28568=CARTESIAN_POINT('Ctrl Pts',(4.58810250737386,4.97409332258953,78.5656622481057));
#28569=CARTESIAN_POINT('Ctrl Pts',(4.45137708685827,5.10020881821975,78.5744117930419));
#28570=CARTESIAN_POINT('Ctrl Pts',(4.30944892636232,5.22068366307784,78.583161337978));
#28571=CARTESIAN_POINT('Ctrl Pts',(4.16280009466838,5.33510865604713,78.5919108829142));
#28572=CARTESIAN_POINT('Ctrl Pts',(4.01615988348954,5.4495269227277,78.6006599135225));
#28573=CARTESIAN_POINT('Ctrl Pts',(3.86479978232383,5.55789587288521,78.6094089441308));
#28574=CARTESIAN_POINT('Ctrl Pts',(3.70923383581206,5.65984746713787,78.6181579747391));
#28575=CARTESIAN_POINT('Ctrl Pts',(3.55366577799671,5.76180044505303,78.6269071240871));
#28576=CARTESIAN_POINT('Ctrl Pts',(3.39389200026962,5.85733573570988,78.6356562734351));
#28577=CARTESIAN_POINT('Ctrl Pts',(3.23045513626155,5.94612887621866,78.6444054227832));
#28578=CARTESIAN_POINT('Ctrl Pts',(3.18695122151658,5.96976399206646,78.6467342868961));
#28579=CARTESIAN_POINT('Ctrl Pts',(3.14318791262709,5.9929216543531,78.6490631510091));
#28580=CARTESIAN_POINT('Ctrl Pts',(3.09917575053268,6.01559628526634,78.6513920151221));
#28581=CARTESIAN_POINT('Origin',(0.,0.,-3.69717978381041));
#28582=CARTESIAN_POINT('',(3.09917575053255,6.01559628526641,81.0455808655427));
#28583=CARTESIAN_POINT('',(3.09917575053259,6.01559628526639,80.651216691749));
#28584=CARTESIAN_POINT('',(3.09917575053259,6.01559628526639,-3.69717978381041));
#28585=CARTESIAN_POINT('',(-6.7669999925025,-0.000318545333296113,79.6971797838099));
#28586=CARTESIAN_POINT('Ctrl Pts',(-6.7669999925025,-0.000318545333296113,
79.6971797838099));
#28587=CARTESIAN_POINT('Ctrl Pts',(-6.76699126828019,-0.185651074678613,
79.7058520742601));
#28588=CARTESIAN_POINT('Ctrl Pts',(-6.7593645097331,-0.370812397315357,
79.7145243647103));
#28589=CARTESIAN_POINT('Ctrl Pts',(-6.74418751263934,-0.555179065130915,
79.7231966551606));
#28590=CARTESIAN_POINT('Ctrl Pts',(-6.728987169257,-0.739829338287013,79.7318822859174));
#28591=CARTESIAN_POINT('Ctrl Pts',(-6.70621341493911,-0.923682226209467,
79.7405679166743));
#28592=CARTESIAN_POINT('Ctrl Pts',(-6.67598545392258,-1.10612260577845,
79.7492535474312));
#28593=CARTESIAN_POINT('Ctrl Pts',(-6.64567895497579,-1.28903699978067,
79.757961745091));
#28594=CARTESIAN_POINT('Ctrl Pts',(-6.60787955356384,-1.47053125611473,
79.7666699427509));
#28595=CARTESIAN_POINT('Ctrl Pts',(-6.56275749079366,-1.65000094455482,
79.7753781404107));
#28596=CARTESIAN_POINT('Ctrl Pts',(-6.51757624396202,-1.82970603324961,
79.7840977601216));
#28597=CARTESIAN_POINT('Ctrl Pts',(-6.46505323702654,-2.00738097265852,
79.7928173798325));
#28598=CARTESIAN_POINT('Ctrl Pts',(-6.40540793799161,-2.18243857826839,
79.8015369995434));
#28599=CARTESIAN_POINT('Ctrl Pts',(-6.34562037681719,-2.3579137200447,79.8102774167317));
#28600=CARTESIAN_POINT('Ctrl Pts',(-6.2786766452146,-2.53075876779444,79.8190178339199));
#28601=CARTESIAN_POINT('Ctrl Pts',(-6.20484459315538,-2.70040600184314,
79.8277582511081));
#28602=CARTESIAN_POINT('Ctrl Pts',(-6.13638854804961,-2.85770054238756,
79.8358622435693));
#28603=CARTESIAN_POINT('Ctrl Pts',(-6.06201137532344,-3.01224609912074,
79.8439662360305));
#28604=CARTESIAN_POINT('Ctrl Pts',(-5.9819606965745,-3.16361110515152,79.8520702284916));
#28605=CARTESIAN_POINT('Ctrl Pts',(-5.9014453592497,-3.31585471770051,79.8602212610236));
#28606=CARTESIAN_POINT('Ctrl Pts',(-5.81498775513594,-3.46526172829884,
79.8683722935556));
#28607=CARTESIAN_POINT('Ctrl Pts',(-5.7228122671405,-3.61133060727847,79.8765233260876));
#28608=CARTESIAN_POINT('Ctrl Pts',(-5.63074384366015,-3.75722982299903,
79.8846648909578));
#28609=CARTESIAN_POINT('Ctrl Pts',(-5.53297094985115,-3.89979831914096,
79.892806455828));
#28610=CARTESIAN_POINT('Ctrl Pts',(-5.42976486685794,-4.03855698122921,
79.9009480206981));
#28611=CARTESIAN_POINT('Ctrl Pts',(-5.32665694302677,-4.17718367014688,
79.9090818421373));
#28612=CARTESIAN_POINT('Ctrl Pts',(-5.21812633448767,-4.31200744751291,
79.9172156635765));
#28613=CARTESIAN_POINT('Ctrl Pts',(-5.10448882341879,-4.44257615034258,
79.9253494850156));
#28614=CARTESIAN_POINT('Ctrl Pts',(-4.99093549321105,-4.57304812995348,
79.9334772810492));
#28615=CARTESIAN_POINT('Ctrl Pts',(-4.87228303231264,-4.69927103664301,
79.9416050770828));
#28616=CARTESIAN_POINT('Ctrl Pts',(-4.74888888196918,-4.82082393234907,
79.9497328731164));
#28617=CARTESIAN_POINT('Ctrl Pts',(-4.62556019810287,-4.94231233845131,
79.9578563569668));
#28618=CARTESIAN_POINT('Ctrl Pts',(-4.49749509479425,-5.05913541182123,
79.9659798408173));
#28619=CARTESIAN_POINT('Ctrl Pts',(-4.36508941462806,-5.17090740608475,
79.9741033246677));
#28620=CARTESIAN_POINT('Ctrl Pts',(-4.23184517865899,-5.28338727824497,
79.9822782564207));
#28621=CARTESIAN_POINT('Ctrl Pts',(-4.09420544734246,-5.39075159227332,
79.9904531881736));
#28622=CARTESIAN_POINT('Ctrl Pts',(-3.95260959059071,-5.49264657741333,
79.9986281199266));
#28623=CARTESIAN_POINT('Ctrl Pts',(-3.81193675626825,-5.59387733862141,
80.0067497616642));
#28624=CARTESIAN_POINT('Ctrl Pts',(-3.66735953678444,-5.68970967033223,
80.014871403402));
#28625=CARTESIAN_POINT('Ctrl Pts',(-3.51933978753285,-5.77983879185987,
80.0229930451396));
#28626=CARTESIAN_POINT('Ctrl Pts',(-3.37130049339222,-5.86997981425676,
80.0311157592787));
#28627=CARTESIAN_POINT('Ctrl Pts',(-3.21981807670386,-5.95441593614001,
80.0392384734178));
#28628=CARTESIAN_POINT('Ctrl Pts',(-3.06538091489876,-6.03288727282173,
80.0473611875569));
#28629=CARTESIAN_POINT('Ctrl Pts',(-2.91089395226344,-6.11138391389049,
80.0554865210002));
#28630=CARTESIAN_POINT('Ctrl Pts',(-2.75345067328943,-6.18391177388882,
80.0636118544435));
#28631=CARTESIAN_POINT('Ctrl Pts',(-2.59356139439414,-6.25025825814489,
80.0717371878868));
#28632=CARTESIAN_POINT('Ctrl Pts',(-2.43193308752715,-6.31732635671269,
80.0799508961245));
#28633=CARTESIAN_POINT('Ctrl Pts',(-2.26780561666465,-6.37807768298584,
80.0881646043621));
#28634=CARTESIAN_POINT('Ctrl Pts',(-2.10172306626406,-6.43234398588365,
80.0963783125997));
#28635=CARTESIAN_POINT('Ctrl Pts',(-1.93714316759201,-6.48611930791891,
80.1045177063302));
#28636=CARTESIAN_POINT('Ctrl Pts',(-1.77064379038275,-6.53352643507237,
80.1126571000606));
#28637=CARTESIAN_POINT('Ctrl Pts',(-1.60276547411663,-6.57445296849705,
80.1207964937911));
#28638=CARTESIAN_POINT('Ctrl Pts',(-1.43258800730884,-6.61594000469293,
80.1290473592823));
#28639=CARTESIAN_POINT('Ctrl Pts',(-1.26099394264601,-6.65076757655893,
80.1372982247735));
#28640=CARTESIAN_POINT('Ctrl Pts',(-1.08855215076031,-6.67887290005396,
80.1455490902648));
#28641=CARTESIAN_POINT('Ctrl Pts',(-0.916110358874604,-6.70697822354898,
80.153799955756));
#28642=CARTESIAN_POINT('Ctrl Pts',(-0.742821228910491,-6.72836131821488,
80.1620508212472));
#28643=CARTESIAN_POINT('Ctrl Pts',(-0.569253656216054,-6.74301410905277,
80.1703016867384));
#28644=CARTESIAN_POINT('Ctrl Pts',(-0.396087756160033,-6.75763299018583,
80.1785334579549));
#28645=CARTESIAN_POINT('Ctrl Pts',(-0.22210414601066,-6.76559849540422,
80.1867652291714));
#28646=CARTESIAN_POINT('Ctrl Pts',(-0.047855088193626,-6.76683078630861,
80.1949970003879));
#28647=CARTESIAN_POINT('Ctrl Pts',(0.126185899374362,-6.76806160573832,
80.2032189420725));
#28648=CARTESIAN_POINT('Ctrl Pts',(0.300491348675806,-6.7625752180599,80.211440883757));
#28649=CARTESIAN_POINT('Ctrl Pts',(0.474502880395008,-6.75034339989432,
80.2196628254415));
#28650=CARTESIAN_POINT('Ctrl Pts',(0.648341490250427,-6.73812373695072,
80.2278765966705));
#28651=CARTESIAN_POINT('Ctrl Pts',(0.821886409229279,-6.71917201784723,
80.2360903678995));
#28652=CARTESIAN_POINT('Ctrl Pts',(0.994578157988799,-6.69351202939471,
80.2443041391285));
#28653=CARTESIAN_POINT('Ctrl Pts',(1.16713288415996,-6.66787240090761,80.2525113931255));
#28654=CARTESIAN_POINT('Ctrl Pts',(1.33883543562522,-6.63553515713876,80.2607186471225));
#28655=CARTESIAN_POINT('Ctrl Pts',(1.50913026499436,-6.59657599389851,80.2689259011195));
#28656=CARTESIAN_POINT('Ctrl Pts',(1.67932407241606,-6.55763994193272,80.2771282864262));
#28657=CARTESIAN_POINT('Ctrl Pts',(1.84811147297831,-6.51208987571257,80.285330671733));
#28658=CARTESIAN_POINT('Ctrl Pts',(2.01494584904912,-6.4600528036077,80.2935330570397));
#28659=CARTESIAN_POINT('Ctrl Pts',(2.18173043001608,-6.4080312630226,80.3017329941781));
#28660=CARTESIAN_POINT('Ctrl Pts',(2.34656280485905,-6.34952667619528,80.3099329313165));
#28661=CARTESIAN_POINT('Ctrl Pts',(2.50891005003434,-6.28471633097602,80.3181328684549));
#28662=CARTESIAN_POINT('Ctrl Pts',(2.67123459541787,-6.21991504769889,80.3263316590579));
#28663=CARTESIAN_POINT('Ctrl Pts',(2.83107437011529,-6.14880989410969,80.3345304496609));
#28664=CARTESIAN_POINT('Ctrl Pts',(2.98791500502242,-6.07162687611499,80.342729240264));
#28665=CARTESIAN_POINT('Ctrl Pts',(3.14476216180441,-5.99444064863326,80.3509283717958));
#28666=CARTESIAN_POINT('Ctrl Pts',(3.29860960869036,-5.91117621143672,80.3591275033275));
#28667=CARTESIAN_POINT('Ctrl Pts',(3.44896617558892,-5.82210626145242,80.3673266348593));
#28668=CARTESIAN_POINT('Ctrl Pts',(3.59935627011023,-5.7330164499899,80.3755275946943));
#28669=CARTESIAN_POINT('Ctrl Pts',(3.74625362593384,-5.63811873000138,80.3837285545293));
#28670=CARTESIAN_POINT('Ctrl Pts',(3.8891946911901,-5.53773000912998,80.3919295143642));
#28671=CARTESIAN_POINT('Ctrl Pts',(4.03226972748446,-5.43724719926376,80.4001381605215));
#28672=CARTESIAN_POINT('Ctrl Pts',(4.17138077111078,-5.33126331254785,80.4083468066788));
#28673=CARTESIAN_POINT('Ctrl Pts',(4.30609535650516,-5.22013714194222,80.4165554528361));
#28674=CARTESIAN_POINT('Ctrl Pts',(4.44087425885037,-5.10895791623176,80.4247680180575));
#28675=CARTESIAN_POINT('Ctrl Pts',(4.5712522505928,-4.99263175010406,80.4329805832789));
#28676=CARTESIAN_POINT('Ctrl Pts',(4.69683267576492,-4.87155537953403,80.4411931485002));
#28677=CARTESIAN_POINT('Ctrl Pts',(4.82258541614656,-4.75031287399405,80.4494169825949));
#28678=CARTESIAN_POINT('Ctrl Pts',(4.94352718524975,-4.6243073961534,80.4576408166895));
#28679=CARTESIAN_POINT('Ctrl Pts',(5.05929985198646,-4.49397085078328,80.4658646507842));
#28680=CARTESIAN_POINT('Ctrl Pts',(5.16567326996443,-4.37421595345513,80.4734208155179));
#28681=CARTESIAN_POINT('Ctrl Pts',(5.26768317643285,-4.25080524346746,80.4809769802517));
#28682=CARTESIAN_POINT('Ctrl Pts',(5.36508391286331,-4.12409548967229,80.4885331449855));
#28683=CARTESIAN_POINT('Ctrl Pts',(5.47652852392743,-3.97911589560306,80.4971788069255));
#28684=CARTESIAN_POINT('Ctrl Pts',(5.58219275646772,-3.82948667938921,80.5058244688656));
#28685=CARTESIAN_POINT('Ctrl Pts',(5.68169250808639,-3.67568486728053,80.5144701308057));
#28686=CARTESIAN_POINT('Ctrl Pts',(5.78106452227576,-3.52208050539437,80.5231046934755));
#28687=CARTESIAN_POINT('Ctrl Pts',(5.87428767147399,-3.36431448412436,80.5317392561454));
#28688=CARTESIAN_POINT('Ctrl Pts',(5.96101936055093,-3.20289512521672,80.5403738188152));
#28689=CARTESIAN_POINT('Ctrl Pts',(6.05081494041197,-3.03577345275566,80.5493134067564));
#28690=CARTESIAN_POINT('Ctrl Pts',(6.13365183298998,-2.86473585119626,80.5582529946975));
#28691=CARTESIAN_POINT('Ctrl Pts',(6.20919844019825,-2.69037984869045,80.5671925826386));
#28692=CARTESIAN_POINT('Ctrl Pts',(6.28196482320838,-2.52244039876286,80.575803180839));
#28693=CARTESIAN_POINT('Ctrl Pts',(6.34796775239083,-2.35142273477379,80.5844137790394));
#28694=CARTESIAN_POINT('Ctrl Pts',(6.40695701572333,-2.17788677361189,80.5930243772399));
#28695=CARTESIAN_POINT('Ctrl Pts',(6.46589044563991,-2.00451506446723,80.6016268254977));
#28696=CARTESIAN_POINT('Ctrl Pts',(6.51782334714075,-1.82863009817014,80.6102292737555));
#28697=CARTESIAN_POINT('Ctrl Pts',(6.56255362652765,-1.65081158796176,80.6188317220133));
#28698=CARTESIAN_POINT('Ctrl Pts',(6.60723356820451,-1.47319318776229,80.6274244894117));
#28699=CARTESIAN_POINT('Ctrl Pts',(6.64472698384982,-1.29364587973253,80.6360172568102));
#28700=CARTESIAN_POINT('Ctrl Pts',(6.67488157492676,-1.11276455762361,80.6446100242086));
#28701=CARTESIAN_POINT('Ctrl Pts',(6.67843631935433,-1.09144154017072,80.6456229741753));
#28702=CARTESIAN_POINT('Ctrl Pts',(6.6818891359297,-1.07010000105353,80.646635924142));
#28703=CARTESIAN_POINT('Ctrl Pts',(6.68523982118511,-1.0487409276084,80.6476488741087));
#28704=CARTESIAN_POINT('Ctrl Pts',(6.71367175746758,-0.867500444258104,
80.656244169314));
#28705=CARTESIAN_POINT('Ctrl Pts',(6.73471237551699,-0.685209894751886,
80.6648394645192));
#28706=CARTESIAN_POINT('Ctrl Pts',(6.74831832548549,-0.502482614541714,
80.6734347597246));
#28707=CARTESIAN_POINT('Ctrl Pts',(6.76193701871019,-0.319584192988989,
80.682038105235));
#28708=CARTESIAN_POINT('Ctrl Pts',(6.76810712222662,-0.13624852877261,80.6906414507454));
#28709=CARTESIAN_POINT('Ctrl Pts',(6.76683740358844,0.0469100564533351,
80.6992447962559));
#28710=CARTESIAN_POINT('Ctrl Pts',(6.76551505072461,0.237661198026486,80.7082047801706));
#28711=CARTESIAN_POINT('Ctrl Pts',(6.75612293780566,0.428219885752169,80.7171647640853));
#28712=CARTESIAN_POINT('Ctrl Pts',(6.73873063703672,0.617898374704722,80.726124748));
#28713=CARTESIAN_POINT('Ctrl Pts',(6.72198491915971,0.800525302880217,80.7347516320915));
#28714=CARTESIAN_POINT('Ctrl Pts',(6.69782321040895,0.982336010378989,80.7433785161829));
#28715=CARTESIAN_POINT('Ctrl Pts',(6.66635996946198,1.1627268628336,80.7520054002744));
#28716=CARTESIAN_POINT('Ctrl Pts',(6.63486665545255,1.34329013571311,80.7606405300779));
#28717=CARTESIAN_POINT('Ctrl Pts',(6.59605794024985,1.52243054607268,80.7692756598815));
#28718=CARTESIAN_POINT('Ctrl Pts',(6.55009878553166,1.69955726581269,80.777910789685));
#28719=CARTESIAN_POINT('Ctrl Pts',(6.50407136954502,1.87694706468546,80.7865587448966));
#28720=CARTESIAN_POINT('Ctrl Pts',(6.45087237543878,2.05231690311487,80.7952067001081));
#28721=CARTESIAN_POINT('Ctrl Pts',(6.39071620493619,2.22509222010369,80.8038546553197));
#28722=CARTESIAN_POINT('Ctrl Pts',(6.38396889421377,2.24447125868193,80.8048246379572));
#28723=CARTESIAN_POINT('Ctrl Pts',(6.37713410730476,2.26381767877992,80.8057946205947));
#28724=CARTESIAN_POINT('Ctrl Pts',(6.37021218380461,2.28313068686557,80.8067646032322));
#28725=CARTESIAN_POINT('Ctrl Pts',(6.3115102399365,2.44691624683938,80.8149906210925));
#28726=CARTESIAN_POINT('Ctrl Pts',(6.24641018884347,2.60865229056004,80.8232166389527));
#28727=CARTESIAN_POINT('Ctrl Pts',(6.17507486429063,2.7678040791223,80.831442656813));
#28728=CARTESIAN_POINT('Ctrl Pts',(6.10381704099951,2.92678295945859,80.8396597376317));
#28729=CARTESIAN_POINT('Ctrl Pts',(6.02633758133013,3.08318285169219,80.8478768184504));
#28730=CARTESIAN_POINT('Ctrl Pts',(5.94284863313208,3.23648561308099,80.856093899269));
#28731=CARTESIAN_POINT('Ctrl Pts',(5.85944769074041,3.38962677783419,80.8643023184524));
#28732=CARTESIAN_POINT('Ctrl Pts',(5.77005005594519,3.53967700554285,80.8725107376357));
#28733=CARTESIAN_POINT('Ctrl Pts',(5.6749152518394,3.68613969952858,80.880719156819));
#28734=CARTESIAN_POINT('Ctrl Pts',(5.57983763741589,3.83251434839754,80.8889226415633));
#28735=CARTESIAN_POINT('Ctrl Pts',(5.47902991569958,3.97530545848919,80.8971261263077));
#28736=CARTESIAN_POINT('Ctrl Pts',(5.37279691093228,4.11404209432482,80.9053296110521));
#28737=CARTESIAN_POINT('Ctrl Pts',(5.26660849486966,4.25272049885185,80.9135296525844));
#28738=CARTESIAN_POINT('Ctrl Pts',(5.15499954851385,4.38734753453143,80.9217296941167));
#28739=CARTESIAN_POINT('Ctrl Pts',(5.0383175143484,4.51748222183665,80.9299297356491));
#28740=CARTESIAN_POINT('Ctrl Pts',(4.92166328754959,4.64758589577303,80.9381278229683));
#28741=CARTESIAN_POINT('Ctrl Pts',(4.79993862089678,4.77319908793876,80.9463259102875));
#28742=CARTESIAN_POINT('Ctrl Pts',(4.67353047667194,4.89391478099267,80.9545239976067));
#28743=CARTESIAN_POINT('Ctrl Pts',(4.54709857854369,5.01465315825678,80.9627236254642));
#28744=CARTESIAN_POINT('Ctrl Pts',(4.41598169958258,5.13049194577093,80.9709232533216));
#28745=CARTESIAN_POINT('Ctrl Pts',(4.28060315415918,5.24106149902885,80.979122881179));
#28746=CARTESIAN_POINT('Ctrl Pts',(4.14521328827664,5.35164029819871,80.9873231946957));
#28747=CARTESIAN_POINT('Ctrl Pts',(4.00556132715072,5.45694876292595,80.9955235082123));
#28748=CARTESIAN_POINT('Ctrl Pts',(3.86210276485753,5.55665827936898,81.003723821729));
#28749=CARTESIAN_POINT('Ctrl Pts',(3.71855185373349,5.65643198199317,81.0119294140478));
#28750=CARTESIAN_POINT('Ctrl Pts',(3.57118974338493,5.75059933539894,81.0201350063666));
#28751=CARTESIAN_POINT('Ctrl Pts',(3.42050050722433,5.83887534376939,81.0283405986854));
#28752=CARTESIAN_POINT('Ctrl Pts',(3.31496586926094,5.90069911314797,81.0340873543045));
#28753=CARTESIAN_POINT('Ctrl Pts',(3.2077999114992,5.95963419113215,81.0398341099236));
#28754=CARTESIAN_POINT('Ctrl Pts',(3.09917575053255,6.01559628526641,81.0455808655427));
#28755=CARTESIAN_POINT('Ctrl Pts',(3.09917575053266,6.01559628526635,79.0457515827422));
#28756=CARTESIAN_POINT('Ctrl Pts',(2.93382384459277,6.10078395293753,79.0545010306546));
#28757=CARTESIAN_POINT('Ctrl Pts',(2.76495772123002,6.17915010267041,79.063250478567));
#28758=CARTESIAN_POINT('Ctrl Pts',(2.59315093316735,6.25042856433167,79.0719999264794));
#28759=CARTESIAN_POINT('Ctrl Pts',(2.42134553245646,6.3217064504144,79.0807493037394));
#28760=CARTESIAN_POINT('Ctrl Pts',(2.24659977927624,6.38589665313445,79.0894986809994));
#28761=CARTESIAN_POINT('Ctrl Pts',(2.06950718689957,6.44278115439063,79.0982480582594));
#28762=CARTESIAN_POINT('Ctrl Pts',(1.89241596572904,6.49966521519711,79.1069973677741));
#28763=CARTESIAN_POINT('Ctrl Pts',(1.71297821457246,6.54924360009533,79.1157466772888));
#28764=CARTESIAN_POINT('Ctrl Pts',(1.53180337335897,6.59134792173544,79.1244959868034));
#28765=CARTESIAN_POINT('Ctrl Pts',(1.35062987477822,6.63345193135297,79.1332452314795));
#28766=CARTESIAN_POINT('Ctrl Pts',(1.16771959102978,6.66808192368234,79.1419944761557));
#28767=CARTESIAN_POINT('Ctrl Pts',(0.983693746906968,6.69512028363167,79.1507437208318));
#28768=CARTESIAN_POINT('Ctrl Pts',(0.799669205419977,6.72215845218866,79.159492903576));
#28769=CARTESIAN_POINT('Ctrl Pts',(0.614529402873566,6.74160505424578,79.1682420863201));
#28770=CARTESIAN_POINT('Ctrl Pts',(0.42890312736332,6.75339404354122,79.1769912690643));
#28771=CARTESIAN_POINT('Ctrl Pts',(0.243278104164084,6.76518295330329,79.1857403927829));
#28772=CARTESIAN_POINT('Ctrl Pts',(0.0571669005394561,6.76931433552275,
79.1944895165015));
#28773=CARTESIAN_POINT('Ctrl Pts',(-0.128798404777041,6.76577415902474,
79.2032386402201));
#28774=CARTESIAN_POINT('Ctrl Pts',(-0.314762517258607,6.76223400523444,
79.2119877078194));
#28775=CARTESIAN_POINT('Ctrl Pts',(-0.500580446819,6.75102239665093,79.2207367754186));
#28776=CARTESIAN_POINT('Ctrl Pts',(-0.685621118842083,6.73217741012503,
79.2294858430178));
#28777=CARTESIAN_POINT('Ctrl Pts',(-0.870660665414059,6.71333253821778,
79.2382348574036));
#28778=CARTESIAN_POINT('Ctrl Pts',(-1.05492267885453,6.68685441030618,79.2469838717893));
#28779=CARTESIAN_POINT('Ctrl Pts',(-1.23778137635229,6.65283295028182,79.2557328861751));
#28780=CARTESIAN_POINT('Ctrl Pts',(-1.42999922978822,6.61707018861871,79.2649296965425));
#28781=CARTESIAN_POINT('Ctrl Pts',(-1.6206660123367,6.57297172934419,79.2741265069099));
#28782=CARTESIAN_POINT('Ctrl Pts',(-1.80906628500359,6.52070304311301,79.2833233172773));
#28783=CARTESIAN_POINT('Ctrl Pts',(-1.98831342545491,6.47097374915042,79.292073315015));
#28784=CARTESIAN_POINT('Ctrl Pts',(-2.16550875896655,6.41384933989544,79.3008233127528));
#28785=CARTESIAN_POINT('Ctrl Pts',(-2.34005036713955,6.34952386240497,79.3095733104906));
#28786=CARTESIAN_POINT('Ctrl Pts',(-2.51458843547033,6.28519968948618,79.3183231307714));
#28787=CARTESIAN_POINT('Ctrl Pts',(-2.68647261718,6.21367483971123,79.3270729510523));
#28788=CARTESIAN_POINT('Ctrl Pts',(-2.85511905908677,6.13519226743869,79.3358227713332));
#28789=CARTESIAN_POINT('Ctrl Pts',(-3.02376230488837,6.05671118252961,79.3445724257917));
#28790=CARTESIAN_POINT('Ctrl Pts',(-3.18916767379864,5.97127275992654,79.3533220802502));
#28791=CARTESIAN_POINT('Ctrl Pts',(-3.35077334102754,5.87916720438015,79.3620717347088));
#28792=CARTESIAN_POINT('Ctrl Pts',(-3.51237616037333,5.78706327195664,79.3708212349772));
#28793=CARTESIAN_POINT('Ctrl Pts',(-3.67017916302264,5.68829258362321,79.3795707352457));
#28794=CARTESIAN_POINT('Ctrl Pts',(-3.82364636566425,5.58319061741067,79.3883202355141));
#28795=CARTESIAN_POINT('Ctrl Pts',(-3.97711106778758,5.47809036367731,79.3970695932225));
#28796=CARTESIAN_POINT('Ctrl Pts',(-4.12623987481884,5.36665920043257,79.4058189509309));
#28797=CARTESIAN_POINT('Ctrl Pts',(-4.27052628213884,5.24927559512371,79.4145683086394));
#28798=CARTESIAN_POINT('Ctrl Pts',(-4.41481053024921,5.13189374643084,79.4233175354159));
#28799=CARTESIAN_POINT('Ctrl Pts',(-4.55425230136462,5.00855981477414,79.4320667621924));
#28800=CARTESIAN_POINT('Ctrl Pts',(-4.6883780063047,4.87969268192151,79.4408159889689));
#28801=CARTESIAN_POINT('Ctrl Pts',(-4.82250188228825,4.7508273063188,79.4495650964398));
#28802=CARTESIAN_POINT('Ctrl Pts',(-4.95130963052905,4.61642907903591,79.4583142039106));
#28803=CARTESIAN_POINT('Ctrl Pts',(-5.07436379033314,4.47695444731749,79.4670633113815));
#28804=CARTESIAN_POINT('Ctrl Pts',(-5.19741643562745,4.33748153220658,79.4758123111712));
#28805=CARTESIAN_POINT('Ctrl Pts',(-5.31471544462706,4.19293255254673,79.484561310961));
#28806=CARTESIAN_POINT('Ctrl Pts',(-5.42586245275555,4.043798417797,79.4933103107507));
#28807=CARTESIAN_POINT('Ctrl Pts',(-5.53702160019085,3.89464799484439,79.5020602660928));
#28808=CARTESIAN_POINT('Ctrl Pts',(-5.64202723081188,3.74091164443946,79.510810221435));
#28809=CARTESIAN_POINT('Ctrl Pts',(-5.74052265232908,3.58311159163328,79.5195601767772));
#28810=CARTESIAN_POINT('Ctrl Pts',(-5.83901427066855,3.42531763191891,79.5283097942596));
#28811=CARTESIAN_POINT('Ctrl Pts',(-5.93099603115673,3.26346052695733,79.537059411742));
#28812=CARTESIAN_POINT('Ctrl Pts',(-6.01615550622685,3.0980900446721,79.5458090292245));
#28813=CARTESIAN_POINT('Ctrl Pts',(-6.10131214578748,2.93272506863936,79.5545583553756));
#28814=CARTESIAN_POINT('Ctrl Pts',(-6.17964682328712,2.76384720416976,79.5633076815267));
#28815=CARTESIAN_POINT('Ctrl Pts',(-6.25089348288541,2.59203002791648,79.5720570076778));
#28816=CARTESIAN_POINT('Ctrl Pts',(-6.32213814889314,2.42021765937072,79.5808060890094));
#28817=CARTESIAN_POINT('Ctrl Pts',(-6.38629508412575,2.24546640831948,79.5895551703409));
#28818=CARTESIAN_POINT('Ctrl Pts',(-6.44314639819806,2.06836976660059,79.5983042516725));
#28819=CARTESIAN_POINT('Ctrl Pts',(-6.50000285283698,1.89125711158283,79.6070541241069));
#28820=CARTESIAN_POINT('Ctrl Pts',(-6.5495522767325,1.71179891440252,79.6158039965413));
#28821=CARTESIAN_POINT('Ctrl Pts',(-6.59162635926388,1.53060476278419,79.6245538689757));
#28822=CARTESIAN_POINT('Ctrl Pts',(-6.633697520552,1.34942319164681,79.6333031338982));
#28823=CARTESIAN_POINT('Ctrl Pts',(-6.66829431424257,1.16650618642687,79.6420523988208));
#28824=CARTESIAN_POINT('Ctrl Pts',(-6.6952992374542,0.982474997618355,79.6508016637433));
#28825=CARTESIAN_POINT('Ctrl Pts',(-6.72230554731446,0.798434359177552,
79.659551377923));
#28826=CARTESIAN_POINT('Ctrl Pts',(-6.74171916496705,0.613279706240161,
79.6683010921026));
#28827=CARTESIAN_POINT('Ctrl Pts',(-6.75347414817276,0.427639953655215,
79.6770508062823));
#28828=CARTESIAN_POINT('Ctrl Pts',(-6.76248837758739,0.285283364199431,
79.6837604654582));
#28829=CARTESIAN_POINT('Ctrl Pts',(-6.76699999999991,0.142641701107,79.6904701246341));
#28830=CARTESIAN_POINT('Ctrl Pts',(-6.767,4.47431244915746E-12,79.6971797838099));
#28831=CARTESIAN_POINT('',(-6.767,4.30001371423856E-12,79.3028202161898));
#28832=CARTESIAN_POINT('Ctrl Pts',(3.09917575053268,6.01559628526634,78.6513920151221));
#28833=CARTESIAN_POINT('Ctrl Pts',(2.93382384459277,6.10078395293753,78.6601414630345));
#28834=CARTESIAN_POINT('Ctrl Pts',(2.76495772122999,6.17915010267042,78.6688909109469));
#28835=CARTESIAN_POINT('Ctrl Pts',(2.5931509331673,6.2504285643317,78.6776403588593));
#28836=CARTESIAN_POINT('Ctrl Pts',(2.42134553245638,6.32170645041443,78.6863897361194));
#28837=CARTESIAN_POINT('Ctrl Pts',(2.24659977927613,6.38589665313449,78.6951391133794));
#28838=CARTESIAN_POINT('Ctrl Pts',(2.06950718689943,6.44278115439067,78.7038884906394));
#28839=CARTESIAN_POINT('Ctrl Pts',(1.89241596572875,6.4996652151972,78.712637800154));
#28840=CARTESIAN_POINT('Ctrl Pts',(1.71297821457201,6.54924360009545,78.7213871096687));
#28841=CARTESIAN_POINT('Ctrl Pts',(1.53180337335837,6.59134792173558,78.7301364191833));
#28842=CARTESIAN_POINT('Ctrl Pts',(1.35062987477771,6.63345193135307,78.7388856638595));
#28843=CARTESIAN_POINT('Ctrl Pts',(1.16771959102937,6.6680819236824,78.7476349085356));
#28844=CARTESIAN_POINT('Ctrl Pts',(0.983693746906654,6.69512028363171,78.7563841532117));
#28845=CARTESIAN_POINT('Ctrl Pts',(0.799669205419761,6.72215845218868,78.7651333359559));
#28846=CARTESIAN_POINT('Ctrl Pts',(0.614529402873448,6.74160505424579,78.7738825187));
#28847=CARTESIAN_POINT('Ctrl Pts',(0.428903127363302,6.75339404354122,78.7826317014442));
#28848=CARTESIAN_POINT('Ctrl Pts',(0.24327810416391,6.7651829533033,78.7913808251628));
#28849=CARTESIAN_POINT('Ctrl Pts',(0.0571669005391258,6.76931433552276,
78.8001299488814));
#28850=CARTESIAN_POINT('Ctrl Pts',(-0.128798404777528,6.76577415902473,
78.8088790726));
#28851=CARTESIAN_POINT('Ctrl Pts',(-0.314762517258994,6.76223400523441,
78.8176281401992));
#28852=CARTESIAN_POINT('Ctrl Pts',(-0.500580446819287,6.7510223966509,78.8263772077985));
#28853=CARTESIAN_POINT('Ctrl Pts',(-0.68562111884227,6.73217741012501,78.8351262753977));
#28854=CARTESIAN_POINT('Ctrl Pts',(-0.870660665414274,6.71333253821775,
78.8438752897835));
#28855=CARTESIAN_POINT('Ctrl Pts',(-1.05492267885478,6.68685441030614,78.8526243041692));
#28856=CARTESIAN_POINT('Ctrl Pts',(-1.23778137635256,6.65283295028177,78.861373318555));
#28857=CARTESIAN_POINT('Ctrl Pts',(-1.42999922978852,6.61707018861864,78.8705701289224));
#28858=CARTESIAN_POINT('Ctrl Pts',(-1.62066601233703,6.57297172934411,78.8797669392898));
#28859=CARTESIAN_POINT('Ctrl Pts',(-1.80906628500394,6.52070304311292,78.8889637496572));
#28860=CARTESIAN_POINT('Ctrl Pts',(-1.98831342545541,6.47097374915027,78.897713747395));
#28861=CARTESIAN_POINT('Ctrl Pts',(-2.16550875896719,6.41384933989523,78.9064637451327));
#28862=CARTESIAN_POINT('Ctrl Pts',(-2.34005036714033,6.34952386240468,78.9152137428705));
#28863=CARTESIAN_POINT('Ctrl Pts',(-2.51458843547113,6.28519968948586,78.9239635631514));
#28864=CARTESIAN_POINT('Ctrl Pts',(-2.68647261718082,6.21367483971087,78.9327133834322));
#28865=CARTESIAN_POINT('Ctrl Pts',(-2.85511905908761,6.1351922674383,78.9414632037131));
#28866=CARTESIAN_POINT('Ctrl Pts',(-3.02376230488922,6.05671118252918,78.9502128581716));
#28867=CARTESIAN_POINT('Ctrl Pts',(-3.18916767379951,5.97127275992608,78.9589625126302));
#28868=CARTESIAN_POINT('Ctrl Pts',(-3.35077334102842,5.87916720437966,78.9677121670887));
#28869=CARTESIAN_POINT('Ctrl Pts',(-3.51237616037433,5.78706327195604,78.9764616673572));
#28870=CARTESIAN_POINT('Ctrl Pts',(-3.67017916302375,5.6882925836225,78.9852111676256));
#28871=CARTESIAN_POINT('Ctrl Pts',(-3.82364636566547,5.58319061740984,78.993960667894));
#28872=CARTESIAN_POINT('Ctrl Pts',(-3.9771110677888,5.47809036367642,79.0027100256025));
#28873=CARTESIAN_POINT('Ctrl Pts',(-4.12623987482006,5.36665920043164,79.0114593833109));
#28874=CARTESIAN_POINT('Ctrl Pts',(-4.27052628214005,5.24927559512273,79.0202087410194));
#28875=CARTESIAN_POINT('Ctrl Pts',(-4.41481053025052,5.13189374642973,79.0289579677959));
#28876=CARTESIAN_POINT('Ctrl Pts',(-4.55425230136601,5.00855981477288,79.0377071945724));
#28877=CARTESIAN_POINT('Ctrl Pts',(-4.68837800630617,4.87969268192011,79.0464564213489));
#28878=CARTESIAN_POINT('Ctrl Pts',(-4.8225018822897,4.75082730631733,79.0552055288198));
#28879=CARTESIAN_POINT('Ctrl Pts',(-4.95130963053048,4.61642907903439,79.0639546362906));
#28880=CARTESIAN_POINT('Ctrl Pts',(-5.07436379033454,4.47695444731591,79.0727037437615));
#28881=CARTESIAN_POINT('Ctrl Pts',(-5.19741643562883,4.33748153220493,79.0814527435512));
#28882=CARTESIAN_POINT('Ctrl Pts',(-5.31471544462841,4.19293255254502,79.0902017433409));
#28883=CARTESIAN_POINT('Ctrl Pts',(-5.42586245275687,4.04379841779524,79.0989507431307));
#28884=CARTESIAN_POINT('Ctrl Pts',(-5.53702160019206,3.89464799484267,79.1077006984728));
#28885=CARTESIAN_POINT('Ctrl Pts',(-5.64202723081298,3.74091164443779,79.116450653815));
#28886=CARTESIAN_POINT('Ctrl Pts',(-5.74052265233008,3.58311159163166,79.1252006091571));
#28887=CARTESIAN_POINT('Ctrl Pts',(-5.83901427066959,3.42531763191713,79.1339502266396));
#28888=CARTESIAN_POINT('Ctrl Pts',(-5.9309960311578,3.26346052695539,79.142699844122));
#28889=CARTESIAN_POINT('Ctrl Pts',(-6.01615550622794,3.09809004466999,79.1514494616045));
#28890=CARTESIAN_POINT('Ctrl Pts',(-6.10131214578846,2.93272506863731,79.1601987877556));
#28891=CARTESIAN_POINT('Ctrl Pts',(-6.179646823288,2.76384720416778,79.1689481139067));
#28892=CARTESIAN_POINT('Ctrl Pts',(-6.25089348288621,2.59203002791456,79.1776974400578));
#28893=CARTESIAN_POINT('Ctrl Pts',(-6.32213814889385,2.42021765936887,79.1864465213894));
#28894=CARTESIAN_POINT('Ctrl Pts',(-6.38629508412637,2.24546640831771,79.1951956027209));
#28895=CARTESIAN_POINT('Ctrl Pts',(-6.44314639819861,2.06836976659889,79.2039446840525));
#28896=CARTESIAN_POINT('Ctrl Pts',(-6.50000285283749,1.8912571115811,79.2126945564869));
#28897=CARTESIAN_POINT('Ctrl Pts',(-6.54955227673297,1.71179891440076,79.2214444289213));
#28898=CARTESIAN_POINT('Ctrl Pts',(-6.5916263592643,1.53060476278238,79.2301943013557));
#28899=CARTESIAN_POINT('Ctrl Pts',(-6.63369752055234,1.34942319164508,79.2389435662782));
#28900=CARTESIAN_POINT('Ctrl Pts',(-6.66829431424286,1.16650618642523,79.2476928312007));
#28901=CARTESIAN_POINT('Ctrl Pts',(-6.69529923745443,0.982474997616808,
79.2564420961232));
#28902=CARTESIAN_POINT('Ctrl Pts',(-6.72230554731464,0.798434359175971,
79.2651918103029));
#28903=CARTESIAN_POINT('Ctrl Pts',(-6.74171916496719,0.613279706238548,
79.2739415244826));
#28904=CARTESIAN_POINT('Ctrl Pts',(-6.75347414817286,0.427639953653572,
79.2826912386623));
#28905=CARTESIAN_POINT('Ctrl Pts',(-6.76248837758742,0.285283364198275,
79.2894008978381));
#28906=CARTESIAN_POINT('Ctrl Pts',(-6.76699999999991,0.142641701106334,
79.296110557014));
#28907=CARTESIAN_POINT('Ctrl Pts',(-6.767,4.30001365154025E-12,79.3028202161898));
#28908=CARTESIAN_POINT('Ctrl Pts',(-6.76699998814839,-0.000400499275143691,
79.3028202161898));
#28909=CARTESIAN_POINT('Ctrl Pts',(-6.76698906540322,-0.184955680925308,
79.3114483693845));
#28910=CARTESIAN_POINT('Ctrl Pts',(-6.759423854444,-0.369326019158339,79.3200765225791));
#28911=CARTESIAN_POINT('Ctrl Pts',(-6.74437525354799,-0.552893696228719,
79.3287046757738));
#28912=CARTESIAN_POINT('Ctrl Pts',(-6.72930224251752,-0.736759135975562,
79.3373468245805));
#28913=CARTESIAN_POINT('Ctrl Pts',(-6.70672162339215,-0.919819020312296,
79.3459889733872));
#28914=CARTESIAN_POINT('Ctrl Pts',(-6.67675560673779,-1.1014642835315,79.3546311221939));
#28915=CARTESIAN_POINT('Ctrl Pts',(-6.64670872982854,-1.28359969805948,
79.3632965909621));
#28916=CARTESIAN_POINT('Ctrl Pts',(-6.60923663947623,-1.46431256296585,
79.3719620597303));
#28917=CARTESIAN_POINT('Ctrl Pts',(-6.56451244123904,-1.64300499354625,
79.3806275284985));
#28918=CARTESIAN_POINT('Ctrl Pts',(-6.51972457954531,-1.82195178704953,
79.3893053322826));
#28919=CARTESIAN_POINT('Ctrl Pts',(-6.46766407913286,-1.9988721201907,79.3979831360666));
#28920=CARTESIAN_POINT('Ctrl Pts',(-6.40855305186145,-2.17318585985583,
79.4066609398507));
#28921=CARTESIAN_POINT('Ctrl Pts',(-6.34929707638161,-2.34792704031221,
79.4153600227796));
#28922=CARTESIAN_POINT('Ctrl Pts',(-6.28295609962157,-2.52004856631107,
79.4240591057085));
#28923=CARTESIAN_POINT('Ctrl Pts',(-6.20980027758688,-2.68899042625331,
79.4327581886375));
#28924=CARTESIAN_POINT('Ctrl Pts',(-6.15926792524473,-2.80568694273686,
79.4387670763977));
#28925=CARTESIAN_POINT('Ctrl Pts',(-6.10548494151629,-2.92086683827788,
79.444775964158));
#28926=CARTESIAN_POINT('Ctrl Pts',(-6.04855265123554,-3.03435327956907,
79.4507848519183));
#28927=CARTESIAN_POINT('Ctrl Pts',(-5.97061225014743,-3.18971640844865,
79.4590110293621));
#28928=CARTESIAN_POINT('Ctrl Pts',(-5.88657306186628,-3.34229182855461,
79.4672372068058));
#28929=CARTESIAN_POINT('Ctrl Pts',(-5.79665788956477,-3.49156788726019,
79.4754633842496));
#28930=CARTESIAN_POINT('Ctrl Pts',(-5.70684373200964,-3.64067624253122,
79.4836803200358));
#28931=CARTESIAN_POINT('Ctrl Pts',(-5.61116691886959,-3.78649231292714,
79.4918972558221));
#28932=CARTESIAN_POINT('Ctrl Pts',(-5.5098973481489,-3.92852646839267,79.5001141916083));
#28933=CARTESIAN_POINT('Ctrl Pts',(-5.40872122212924,-4.07042956435928,
79.5083235453628));
#28934=CARTESIAN_POINT('Ctrl Pts',(-5.30196282298704,-4.20855740507196,
79.5165328991172));
#28935=CARTESIAN_POINT('Ctrl Pts',(-5.18993683028937,-4.34244685604856,
79.5247422528716));
#28936=CARTESIAN_POINT('Ctrl Pts',(-5.07799172976975,-4.47623962759346,
79.532945678783));
#28937=CARTESIAN_POINT('Ctrl Pts',(-4.96078684111141,-4.60579983139573,
79.5411491046943));
#28938=CARTESIAN_POINT('Ctrl Pts',(-4.83867888205708,-4.73069505213925,
79.5493525306056));
#28939=CARTESIAN_POINT('Ctrl Pts',(-4.71663460008055,-4.85552514229876,
79.5575516785797));
#28940=CARTESIAN_POINT('Ctrl Pts',(-4.58969259155407,-4.97569483994611,
79.5657508265538));
#28941=CARTESIAN_POINT('Ctrl Pts',(-4.45824846587645,-5.0908063817543,79.5739499745278));
#28942=CARTESIAN_POINT('Ctrl Pts',(-4.32682909980619,-5.20589624045902,
79.582147578061));
#28943=CARTESIAN_POINT('Ctrl Pts',(-4.19090957123172,-5.31592960045705,
79.5903451815942));
#28944=CARTESIAN_POINT('Ctrl Pts',(-4.05092103613112,-5.42054681365546,
79.5985427851273));
#28945=CARTESIAN_POINT('Ctrl Pts',(-3.91094260070558,-5.52515647909393,
79.6067397972325));
#28946=CARTESIAN_POINT('Ctrl Pts',(-3.76689603018786,-5.62435056051894,
79.6149368093378));
#28947=CARTESIAN_POINT('Ctrl Pts',(-3.61924408083728,-5.71781088208803,
79.623133821443));
#28948=CARTESIAN_POINT('Ctrl Pts',(-3.47157594793389,-5.81128144747751,
79.6313317319906));
#28949=CARTESIAN_POINT('Ctrl Pts',(-3.32030195203603,-5.89901680906969,
79.6395296425383));
#28950=CARTESIAN_POINT('Ctrl Pts',(-3.16591227150854,-5.98074313853317,
79.647727553086));
#28951=CARTESIAN_POINT('Ctrl Pts',(-3.01147760811152,-6.06249327972296,
79.6559278521711));
#28952=CARTESIAN_POINT('Ctrl Pts',(-2.85392576881812,-6.13823073366157,
79.6641281512563));
#28953=CARTESIAN_POINT('Ctrl Pts',(-2.69376990979961,-6.20772846321891,
79.6723284503414));
#28954=CARTESIAN_POINT('Ctrl Pts',(-2.53344714983676,-6.27729861745533,
79.6805372950875));
#28955=CARTESIAN_POINT('Ctrl Pts',(-2.37051527807995,-6.34061591329752,
79.6887461398335));
#28956=CARTESIAN_POINT('Ctrl Pts',(-2.20550667459669,-6.39750180213413,
79.6969549845795));
#28957=CARTESIAN_POINT('Ctrl Pts',(-2.04040950560559,-6.45441822348558,
79.7051682352807));
#28958=CARTESIAN_POINT('Ctrl Pts',(-1.87323372583407,-6.50489625267868,
79.7133814859819));
#28959=CARTESIAN_POINT('Ctrl Pts',(-1.70452502200897,-6.54880778839518,
79.7215947366831));
#28960=CARTESIAN_POINT('Ctrl Pts',(-1.53556953674757,-6.59278355643406,
79.7298200014521));
#28961=CARTESIAN_POINT('Ctrl Pts',(-1.36507699665651,-6.63017355870686,
79.738045266221));
#28962=CARTESIAN_POINT('Ctrl Pts',(-1.19360264973322,-6.66090096867908,
79.74627053099));
#28963=CARTESIAN_POINT('Ctrl Pts',(-1.03851658083228,-6.68869167501855,
79.7537096844353));
#28964=CARTESIAN_POINT('Ctrl Pts',(-0.882627683050216,-6.71103310593623,
79.7611488378805));
#28965=CARTESIAN_POINT('Ctrl Pts',(-0.726348091822014,-6.7279051308343,
79.7685879913258));
#28966=CARTESIAN_POINT('Ctrl Pts',(-0.55353567822464,-6.74656204772279,
79.7768141330241));
#28967=CARTESIAN_POINT('Ctrl Pts',(-0.379762391741271,-6.75858249991527,
79.7850402747225));
#28968=CARTESIAN_POINT('Ctrl Pts',(-0.205578996589351,-6.7638765716238,
79.7932664164208));
#28969=CARTESIAN_POINT('Ctrl Pts',(-0.0315912802210126,-6.769164695937,
79.8014833168168));
#28970=CARTESIAN_POINT('Ctrl Pts',(0.142805272178604,-6.76774147593213,
79.8097002172129));
#28971=CARTESIAN_POINT('Ctrl Pts',(0.317052893303833,-6.75956851158768,
79.817917117609));
#28972=CARTESIAN_POINT('Ctrl Pts',(0.491139737944541,-6.75140308835322,
79.8261264363557));
#28973=CARTESIAN_POINT('Ctrl Pts',(0.665077568985269,-6.73650034060762,
79.8343357551025));
#28974=CARTESIAN_POINT('Ctrl Pts',(0.838306629016581,-6.71487386298111,
79.8425450738492));
#28975=CARTESIAN_POINT('Ctrl Pts',(1.01141061122818,-6.69326300047524,79.8507484651627));
#28976=CARTESIAN_POINT('Ctrl Pts',(1.18380648732817,-6.66493812222926,79.8589518564762));
#28977=CARTESIAN_POINT('Ctrl Pts',(1.35493754616958,-6.62996479975422,79.8671552477897));
#28978=CARTESIAN_POINT('Ctrl Pts',(1.52597937202656,-6.5950097134425,79.8753543616033));
#28979=CARTESIAN_POINT('Ctrl Pts',(1.69575734395096,-6.55341316082856,79.8835534754169));
#28980=CARTESIAN_POINT('Ctrl Pts',(1.86372280741979,-6.50529217615191,79.8917525892304));
#28981=CARTESIAN_POINT('Ctrl Pts',(2.0316566474713,-6.45718025137335,79.8999501593696));
#28982=CARTESIAN_POINT('Ctrl Pts',(2.19777831266497,-6.40254643402087,79.9081477295087));
#28983=CARTESIAN_POINT('Ctrl Pts',(2.36155192827467,-6.34155828563155,79.9163452996478));
#28984=CARTESIAN_POINT('Ctrl Pts',(2.52531373754777,-6.28057453383937,79.9245422788293));
#28985=CARTESIAN_POINT('Ctrl Pts',(2.68672749790332,-6.21323748764651,79.9327392580107));
#28986=CARTESIAN_POINT('Ctrl Pts',(2.84527507413101,-6.13976373751701,79.9409362371921));
#28987=CARTESIAN_POINT('Ctrl Pts',(3.00384003779941,-6.06628192974005,79.9491341153119));
#28988=CARTESIAN_POINT('Ctrl Pts',(3.15953786560464,-5.98666222807343,79.9573319934317));
#28989=CARTESIAN_POINT('Ctrl Pts',(3.31187284218944,-5.90116829764819,79.9655298715514));
#28990=CARTESIAN_POINT('Ctrl Pts',(3.4642522128568,-5.81564945223172,79.9737301387304));
#28991=CARTESIAN_POINT('Ctrl Pts',(3.61326646751699,-5.72425314367834,79.9819304059094));
#28992=CARTESIAN_POINT('Ctrl Pts',(3.75844677241995,-5.62728770002797,79.9901306730883));
#28993=CARTESIAN_POINT('Ctrl Pts',(3.90377838994009,-5.53022119518294,79.9983394869079));
#28994=CARTESIAN_POINT('Ctrl Pts',(4.04526777584407,-5.42757415846521,80.0065483007275));
#28995=CARTESIAN_POINT('Ctrl Pts',(4.18247643829757,-5.31969734506444,80.0147571145471));
#28996=CARTESIAN_POINT('Ctrl Pts',(4.31975875358718,-5.21176262399869,80.0229703348116));
#28997=CARTESIAN_POINT('Ctrl Pts',(4.45275549164056,-5.09859276199623,80.0311835550761));
#28998=CARTESIAN_POINT('Ctrl Pts',(4.5810633547436,-4.98057702880151,80.0393967753406));
#28999=CARTESIAN_POINT('Ctrl Pts',(4.70955892024492,-4.86238864963156,80.0476220107779));
#29000=CARTESIAN_POINT('Ctrl Pts',(4.83335164838529,-4.73934048509996,80.0558472462152));
#29001=CARTESIAN_POINT('Ctrl Pts',(4.95207616011753,-4.61185761970116,80.0640724816525));
#29002=CARTESIAN_POINT('Ctrl Pts',(5.0594599440381,-4.49655209204032,80.0715120313462));
#29003=CARTESIAN_POINT('Ctrl Pts',(5.16269790830587,-4.3776192024549,80.0789515810399));
#29004=CARTESIAN_POINT('Ctrl Pts',(5.26154981968509,-4.25539451695984,80.0863911307336));
#29005=CARTESIAN_POINT('Ctrl Pts',(5.36987625030378,-4.12145513502538,80.0945437284172));
#29006=CARTESIAN_POINT('Ctrl Pts',(5.47325436973728,-3.98316719419299,80.1026963261008));
#29007=CARTESIAN_POINT('Ctrl Pts',(5.57131138186526,-3.84093458500644,80.1108489237844));
#29008=CARTESIAN_POINT('Ctrl Pts',(5.66925479779108,-3.69886674816893,80.1189920769202));
#29009=CARTESIAN_POINT('Ctrl Pts',(5.76188917176911,-3.5528636374609,80.1271352300561));
#29010=CARTESIAN_POINT('Ctrl Pts',(5.84888078223282,-3.40336342391282,80.1352783831919));
#29011=CARTESIAN_POINT('Ctrl Pts',(5.93578990390099,-3.25400497222527,80.1434138146763));
#29012=CARTESIAN_POINT('Ctrl Pts',(6.01706673200033,-3.10115633339307,80.1515492461607));
#29013=CARTESIAN_POINT('Ctrl Pts',(6.09241984372683,-2.94528597045577,80.1596846776451));
#29014=CARTESIAN_POINT('Ctrl Pts',(6.16771733585885,-2.78953065845901,80.1678141042096));
#29015=CARTESIAN_POINT('Ctrl Pts',(6.23709965942037,-2.63075839119167,80.1759435307741));
#29016=CARTESIAN_POINT('Ctrl Pts',(6.30032049812378,-2.46946363020826,80.1840729573386));
#29017=CARTESIAN_POINT('Ctrl Pts',(6.36350795138381,-2.30825404520829,80.1921980909434));
#29018=CARTESIAN_POINT('Ctrl Pts',(6.42054026663406,-2.14452495895371,80.2003232245483));
#29019=CARTESIAN_POINT('Ctrl Pts',(6.47121859660633,-1.97879227685385,80.2084483581531));
#29020=CARTESIAN_POINT('Ctrl Pts',(6.52208994429173,-1.812428371442,80.2166044378193));
#29021=CARTESIAN_POINT('Ctrl Pts',(6.56655865586342,-1.64404591651449,80.2247605174854));
#29022=CARTESIAN_POINT('Ctrl Pts',(6.60447349218334,-1.47418414421252,80.2329165971516));
#29023=CARTESIAN_POINT('Ctrl Pts',(6.64223605159712,-1.30500458572629,80.241039919652));
#29024=CARTESIAN_POINT('Ctrl Pts',(6.6734972234809,-1.13435793474114,80.2491632421524));
#29025=CARTESIAN_POINT('Ctrl Pts',(6.69815844613823,-0.962788881545214,
80.2572865646528));
#29026=CARTESIAN_POINT('Ctrl Pts',(6.72282295310628,-0.791196979276123,
80.265410968994));
#29027=CARTESIAN_POINT('Ctrl Pts',(6.74088570806473,-0.618682792252615,
80.2735353733351));
#29028=CARTESIAN_POINT('Ctrl Pts',(6.75229985867353,-0.445797732786421,
80.2816597776763));
#29029=CARTESIAN_POINT('Ctrl Pts',(6.76371770093596,-0.27285675748553,80.2897868096757));
#29030=CARTESIAN_POINT('Ctrl Pts',(6.76848263274627,-0.0995450357197435,
80.297913841675));
#29031=CARTESIAN_POINT('Ctrl Pts',(6.76659990900356,0.0735844512996528,
80.3060408736744));
#29032=CARTESIAN_POINT('Ctrl Pts',(6.764705042075,0.247830588355886,80.31422032338));
#29033=CARTESIAN_POINT('Ctrl Pts',(6.75607647505621,0.421891756011707,80.3223997730855));
#29034=CARTESIAN_POINT('Ctrl Pts',(6.74077262160298,0.595208756528067,80.3305792227911));
#29035=CARTESIAN_POINT('Ctrl Pts',(6.72554061072609,0.767712135829498,80.3387202747988));
#29036=CARTESIAN_POINT('Ctrl Pts',(6.70369596187844,0.939477965526954,80.3468613268066));
#29037=CARTESIAN_POINT('Ctrl Pts',(6.67534771068181,1.10996483795442,80.3550023788144));
#29038=CARTESIAN_POINT('Ctrl Pts',(6.64679890047,1.28165787576388,80.3632010273688));
#29039=CARTESIAN_POINT('Ctrl Pts',(6.61165420335213,1.45205342352498,80.3713996759233));
#29040=CARTESIAN_POINT('Ctrl Pts',(6.57007602045649,1.62061410749833,80.3795983244777));
#29041=CARTESIAN_POINT('Ctrl Pts',(6.52849783756082,1.78917479147181,80.3877969730322));
#29042=CARTESIAN_POINT('Ctrl Pts',(6.48048633388413,1.95590027276036,80.3959956215866));
#29043=CARTESIAN_POINT('Ctrl Pts',(6.42625294640687,2.12027405511577,80.404194270141));
#29044=CARTESIAN_POINT('Ctrl Pts',(6.37178269870508,2.28536572755338,80.412428725674));
#29045=CARTESIAN_POINT('Ctrl Pts',(6.31086686766189,2.44859841521295,80.4206631812069));
#29046=CARTESIAN_POINT('Ctrl Pts',(6.24364890358894,2.60943238439179,80.4288976367398));
#29047=CARTESIAN_POINT('Ctrl Pts',(6.17651309793738,2.77006977122549,80.4371220275545));
#29048=CARTESIAN_POINT('Ctrl Pts',(6.10309063599951,2.92831395072693,80.4453464183692));
#29049=CARTESIAN_POINT('Ctrl Pts',(6.02357485675091,3.08363988577108,80.4535708091839));
#29050=CARTESIAN_POINT('Ctrl Pts',(5.94395413507908,3.23917081509647,80.4618060542908));
#29051=CARTESIAN_POINT('Ctrl Pts',(5.85822410089879,3.39177544385225,80.4700412993976));
#29052=CARTESIAN_POINT('Ctrl Pts',(5.76662812388039,3.5409446593913,80.4782765445045));
#29053=CARTESIAN_POINT('Ctrl Pts',(5.67533462049186,3.68962127956145,80.4864845947));
#29054=CARTESIAN_POINT('Ctrl Pts',(5.57821402459683,3.83488482288373,80.4946926448955));
#29055=CARTESIAN_POINT('Ctrl Pts',(5.47555411764076,3.9762540292073,80.5029006950909));
#29056=CARTESIAN_POINT('Ctrl Pts',(5.37295013608146,4.11754622271069,80.5111042738381));
#29057=CARTESIAN_POINT('Ctrl Pts',(5.26481306281275,4.25494801512752,80.5193078525853));
#29058=CARTESIAN_POINT('Ctrl Pts',(5.15147439772318,4.38800644138117,80.5275114313325));
#29059=CARTESIAN_POINT('Ctrl Pts',(5.03817693499965,4.52101649648116,80.5357120278066));
#29060=CARTESIAN_POINT('Ctrl Pts',(4.91968187919999,4.64968605846027,80.5439126242807));
#29061=CARTESIAN_POINT('Ctrl Pts',(4.79636151349017,4.77359458185446,80.5521132207548));
#29062=CARTESIAN_POINT('Ctrl Pts',(4.67216855260053,4.89837986213816,80.5603718433376));
#29063=CARTESIAN_POINT('Ctrl Pts',(4.54308196075631,5.01833617843895,80.5686304659205));
#29064=CARTESIAN_POINT('Ctrl Pts',(4.40952059185325,5.13307092781915,80.5768890885033));
#29065=CARTESIAN_POINT('Ctrl Pts',(4.27689665310766,5.24700038585605,80.5850897461078));
#29066=CARTESIAN_POINT('Ctrl Pts',(4.13986084765876,5.35578113020822,80.5932904037122));
#29067=CARTESIAN_POINT('Ctrl Pts',(3.99885715283741,5.45906864503471,80.6014910613166));
#29068=CARTESIAN_POINT('Ctrl Pts',(3.85635846642072,5.56345126567928,80.6097786663886));
#29069=CARTESIAN_POINT('Ctrl Pts',(3.70980756084845,5.66222327065163,80.6180662714607));
#29070=CARTESIAN_POINT('Ctrl Pts',(3.55969324529376,5.75507367454232,80.6263538765328));
#29071=CARTESIAN_POINT('Ctrl Pts',(3.40957892973918,5.84792407843294,80.6346414816049));
#29072=CARTESIAN_POINT('Ctrl Pts',(3.25590153894876,5.93485270808649,80.642929086677));
#29073=CARTESIAN_POINT('Ctrl Pts',(3.09917575053259,6.01559628526639,80.651216691749));
#29074=CARTESIAN_POINT('Origin',(0.,0.,-3.69717978381041));
#29075=CARTESIAN_POINT('',(3.09917575053248,6.01559628526645,83.0458432482751));
#29076=CARTESIAN_POINT('',(3.09917575053247,6.01559628526645,82.6513920151221));
#29077=CARTESIAN_POINT('',(3.09917575053259,6.01559628526639,-3.69717978381041));
#29078=CARTESIAN_POINT('',(-6.76699738887188,-0.00594466156221417,81.6971797837697));
#29079=CARTESIAN_POINT('Ctrl Pts',(-6.76699738887114,-0.00594466241648763,
81.6971797838099));
#29080=CARTESIAN_POINT('Ctrl Pts',(-6.76678155133687,-0.25163935935655,
81.7087532426108));
#29081=CARTESIAN_POINT('Ctrl Pts',(-6.75318140864,-0.49677316040071,81.7203267014117));
#29082=CARTESIAN_POINT('Ctrl Pts',(-6.72639980188629,-0.740158567594872,
81.7319001602126));
#29083=CARTESIAN_POINT('Ctrl Pts',(-6.70359956999444,-0.947362107477749,
81.7417530994659));
#29084=CARTESIAN_POINT('Ctrl Pts',(-6.67124650991105,-1.1532993901334,81.7516060387192));
#29085=CARTESIAN_POINT('Ctrl Pts',(-6.62949122889958,-1.3572527568377,81.7614589779725));
#29086=CARTESIAN_POINT('Ctrl Pts',(-6.5946355564979,-1.52750503542045,81.7696838255724));
#29087=CARTESIAN_POINT('Ctrl Pts',(-6.5531683641493,-1.69665270370569,81.7779086731722));
#29088=CARTESIAN_POINT('Ctrl Pts',(-6.50517151477902,-1.86414392236962,
81.786133520772));
#29089=CARTESIAN_POINT('Ctrl Pts',(-6.45722872055795,-2.03144650859345,
81.7943491053605));
#29090=CARTESIAN_POINT('Ctrl Pts',(-6.4027710106368,-2.19709601819849,81.8025646899489));
#29091=CARTESIAN_POINT('Ctrl Pts',(-6.34193145251597,-2.3605496079491,81.8107802745373));
#29092=CARTESIAN_POINT('Ctrl Pts',(-6.28114818941145,-2.52385195362786,
81.8189882572219));
#29093=CARTESIAN_POINT('Ctrl Pts',(-6.21399496268251,-2.68496209188757,
81.8271962399065));
#29094=CARTESIAN_POINT('Ctrl Pts',(-6.140654975692,-2.84335109852954,81.8354042225911));
#29095=CARTESIAN_POINT('Ctrl Pts',(-6.06736811968293,-3.0016253606274,81.8436062590219));
#29096=CARTESIAN_POINT('Ctrl Pts',(-5.98790358081624,-3.15718209335518,
81.8518082954528));
#29097=CARTESIAN_POINT('Ctrl Pts',(-5.90249314900087,-3.30951108564358,
81.8600103318836));
#29098=CARTESIAN_POINT('Ctrl Pts',(-5.81712744139058,-3.4617603125808,81.8682080734109));
#29099=CARTESIAN_POINT('Ctrl Pts',(-5.72582221846909,-3.61078485397099,
81.8764058149383));
#29100=CARTESIAN_POINT('Ctrl Pts',(-5.62885584206917,-3.7560978300896,81.8846035564656));
#29101=CARTESIAN_POINT('Ctrl Pts',(-5.53190790230778,-3.90138317722057,
81.8927997393208));
#29102=CARTESIAN_POINT('Ctrl Pts',(-5.4293011468347,-4.04295806315007,81.9009959221759));
#29103=CARTESIAN_POINT('Ctrl Pts',(-5.3213581806263,-4.18036315569372,81.909192105031));
#29104=CARTESIAN_POINT('Ctrl Pts',(-5.21342316058342,-4.31775813323269,
81.9173876845284));
#29105=CARTESIAN_POINT('Ctrl Pts',(-5.10015293308397,-4.45098364597748,
81.9255832640258));
#29106=CARTESIAN_POINT('Ctrl Pts',(-4.98191140900137,-4.57961217930754,
81.9337788435231));
#29107=CARTESIAN_POINT('Ctrl Pts',(-4.86365707654927,-4.70825464616727,
81.9419753107967));
#29108=CARTESIAN_POINT('Ctrl Pts',(-4.74043061752888,-4.83229887729244,
81.9501717780703));
#29109=CARTESIAN_POINT('Ctrl Pts',(-4.61263396174229,-4.95135304083456,
81.9583682453439));
#29110=CARTESIAN_POINT('Ctrl Pts',(-4.48480021133777,-5.07044176137415,
81.9665670917472));
#29111=CARTESIAN_POINT('Ctrl Pts',(-4.35239388431934,-5.18453728471014,
81.9747659381505));
#29112=CARTESIAN_POINT('Ctrl Pts',(-4.21585127287226,-5.29328697928059,
81.9829647845538));
#29113=CARTESIAN_POINT('Ctrl Pts',(-4.07916596111597,-5.40215032785894,
81.991172199549));
#29114=CARTESIAN_POINT('Ctrl Pts',(-3.93833600956304,-5.50565646190259,
81.9993796145442));
#29115=CARTESIAN_POINT('Ctrl Pts',(-3.79382889366723,-5.6034945637143,82.0075870295394));
#29116=CARTESIAN_POINT('Ctrl Pts',(-3.64924432705886,-5.70138510329458,
82.0157988434193));
#29117=CARTESIAN_POINT('Ctrl Pts',(-3.50097897162205,-5.79360136524906,
82.0240106572992));
#29118=CARTESIAN_POINT('Ctrl Pts',(-3.34952627567986,-5.8798777817681,82.0322224711791));
#29119=CARTESIAN_POINT('Ctrl Pts',(-3.19785054251053,-5.96628125348804,
82.0404463782092));
#29120=CARTESIAN_POINT('Ctrl Pts',(-3.04297840675532,-6.04672723307338,
82.0486702852393));
#29121=CARTESIAN_POINT('Ctrl Pts',(-2.88542590258064,-6.12099717045489,
82.0568941922693));
#29122=CARTESIAN_POINT('Ctrl Pts',(-2.7398501112934,-6.18962130918123,82.0644929402527));
#29123=CARTESIAN_POINT('Ctrl Pts',(-2.5919863963532,-6.25297313886653,82.0720916882361));
#29124=CARTESIAN_POINT('Ctrl Pts',(-2.4422535017986,-6.31091806577716,82.0796904362195));
#29125=CARTESIAN_POINT('Ctrl Pts',(-2.28163886038022,-6.37307410493908,
82.0878414185819));
#29126=CARTESIAN_POINT('Ctrl Pts',(-2.11839752773329,-6.42919224847301,
82.0959924009443));
#29127=CARTESIAN_POINT('Ctrl Pts',(-1.95302775807828,-6.47904094570915,
82.1041433833067));
#29128=CARTESIAN_POINT('Ctrl Pts',(-1.78785008071304,-6.52883173907076,
82.1122848975488));
#29129=CARTESIAN_POINT('Ctrl Pts',(-1.6205492343434,-6.57236747812648,82.1204264117909));
#29130=CARTESIAN_POINT('Ctrl Pts',(-1.45164418627425,-6.60946428664655,
82.1285679260331));
#29131=CARTESIAN_POINT('Ctrl Pts',(-1.28289979323479,-6.64652581031905,
82.136701696426));
#29132=CARTESIAN_POINT('Ctrl Pts',(-1.11255459095754,-6.6771605183777,82.144835466819));
#29133=CARTESIAN_POINT('Ctrl Pts',(-0.941143475441524,-6.70123406236746,
82.152969237212));
#29134=CARTESIAN_POINT('Ctrl Pts',(-0.769859347333846,-6.72528977182559,
82.1610969818206));
#29135=CARTESIAN_POINT('Ctrl Pts',(-0.597511238958798,-6.7427939450621,
82.1692247264292));
#29136=CARTESIAN_POINT('Ctrl Pts',(-0.424645027153775,-6.75366312462456,
82.1773524710378));
#29137=CARTESIAN_POINT('Ctrl Pts',(-0.251870536929661,-6.76452653707775,
82.185475903123));
#29138=CARTESIAN_POINT('Ctrl Pts',(-0.078578854923129,-6.76876194406958,
82.1935993352081));
#29139=CARTESIAN_POINT('Ctrl Pts',(0.0946782218924676,-6.7663376382131,
82.2017227672933));
#29140=CARTESIAN_POINT('Ctrl Pts',(0.269034366824355,-6.76389795360663,
82.2098977309255));
#29141=CARTESIAN_POINT('Ctrl Pts',(0.443355093589183,-6.75471372536158,
82.2180726945577));
#29142=CARTESIAN_POINT('Ctrl Pts',(0.617076688796914,-6.73880592984717,
82.2262476581899));
#29143=CARTESIAN_POINT('Ctrl Pts',(0.789664057197207,-6.72300199619345,
82.2343692475546));
#29144=CARTESIAN_POINT('Ctrl Pts',(0.961659728066461,-6.7005620903319,82.2424908369192));
#29145=CARTESIAN_POINT('Ctrl Pts',(1.13251514981973,-6.67155892092911,82.2506124262839));
#29146=CARTESIAN_POINT('Ctrl Pts',(1.30339312799251,-6.64255192251317,82.2587350878649));
#29147=CARTESIAN_POINT('Ctrl Pts',(1.47313019634748,-6.60697999592719,82.2668577494459));
#29148=CARTESIAN_POINT('Ctrl Pts',(1.64118721566619,-6.56496713800868,82.2749804110269));
#29149=CARTESIAN_POINT('Ctrl Pts',(1.80929842498212,-6.5229407330413,82.2831056917607));
#29150=CARTESIAN_POINT('Ctrl Pts',(1.97572815163149,-6.47446934975396,82.2912309724945));
#29151=CARTESIAN_POINT('Ctrl Pts',(2.13995169891577,-6.4197270756869,82.2993562532283));
#29152=CARTESIAN_POINT('Ctrl Pts',(2.30596441665834,-6.36438839957398,82.3075700566648));
#29153=CARTESIAN_POINT('Ctrl Pts',(2.46972223756801,-6.30264151435704,82.3157838601012));
#29154=CARTESIAN_POINT('Ctrl Pts',(2.63070401635478,-6.23471614256294,82.3239976635377));
#29155=CARTESIAN_POINT('Ctrl Pts',(2.79022641175924,-6.16740654952082,82.3321370045827));
#29156=CARTESIAN_POINT('Ctrl Pts',(2.94702258740959,-6.09403024458741,82.3402763456277));
#29157=CARTESIAN_POINT('Ctrl Pts',(3.10061072442964,-6.0148567842927,82.3484156866727));
#29158=CARTESIAN_POINT('Ctrl Pts',(3.25630650258359,-5.93459685179469,82.3566667213049));
#29159=CARTESIAN_POINT('Ctrl Pts',(3.40870521619962,-5.84837969843268,82.3649177559372));
#29160=CARTESIAN_POINT('Ctrl Pts',(3.55733614980349,-5.7565309447011,82.3731687905694));
#29161=CARTESIAN_POINT('Ctrl Pts',(3.70596708340735,-5.66468219096952,82.3814198252017));
#29162=CARTESIAN_POINT('Ctrl Pts',(3.85082995595522,-5.56720210682114,82.3896708598339));
#29163=CARTESIAN_POINT('Ctrl Pts',(3.99148990935795,-5.46445764037875,82.3979218944662));
#29164=CARTESIAN_POINT('Ctrl Pts',(4.13182148536352,-5.3619530358135,82.406153666663));
#29165=CARTESIAN_POINT('Ctrl Pts',(4.26840793867015,-5.25388874326233,82.4143854388598));
#29166=CARTESIAN_POINT('Ctrl Pts',(4.40077994327748,-5.14056659239491,82.4226172110565));
#29167=CARTESIAN_POINT('Ctrl Pts',(4.53299388251097,-5.02737975947629,82.4308391536964));
#29168=CARTESIAN_POINT('Ctrl Pts',(4.66100312434764,-4.90894780072468,82.4390610963364));
#29169=CARTESIAN_POINT('Ctrl Pts',(4.78436756753397,-4.78561552767553,82.4472830389763));
#29170=CARTESIAN_POINT('Ctrl Pts',(4.90760941842082,-4.66240581495707,82.455496811135));
#29171=CARTESIAN_POINT('Ctrl Pts',(5.02621541120786,-4.53430573739926,82.4637105832938));
#29172=CARTESIAN_POINT('Ctrl Pts',(5.13977871639818,-4.40170009728744,82.4719243554526));
#29173=CARTESIAN_POINT('Ctrl Pts',(5.25325191421958,-4.26919967377984,82.480131610353));
#29174=CARTESIAN_POINT('Ctrl Pts',(5.36169016183966,-4.1322010791893,82.4883388652534));
#29175=CARTESIAN_POINT('Ctrl Pts',(5.46472363448574,-3.99112573075479,82.4965461201539));
#29176=CARTESIAN_POINT('Ctrl Pts',(5.5676959854946,-3.85013407120357,82.504748506337));
#29177=CARTESIAN_POINT('Ctrl Pts',(5.66526973794926,-3.70507076416349,82.51295089252));
#29178=CARTESIAN_POINT('Ctrl Pts',(5.75711545423851,-3.55639011450771,82.5211532787031));
#29179=CARTESIAN_POINT('Ctrl Pts',(5.84893375682112,-3.40775384240023,82.5293532166739));
#29180=CARTESIAN_POINT('Ctrl Pts',(5.93502723747499,-3.25550268078992,82.5375531546448));
#29181=CARTESIAN_POINT('Ctrl Pts',(6.01510976560997,-3.10011991827148,82.5457530926156));
#29182=CARTESIAN_POINT('Ctrl Pts',(6.0951810961465,-2.94475888226221,82.553951884024));
#29183=CARTESIAN_POINT('Ctrl Pts',(6.16924298323341,-2.78626743555129,82.5621506754325));
#29184=CARTESIAN_POINT('Ctrl Pts',(6.23705524922844,-2.62515348466941,82.570349466841));
#29185=CARTESIAN_POINT('Ctrl Pts',(6.30487033481908,-2.46403283476073,82.5785485991505));
#29186=CARTESIAN_POINT('Ctrl Pts',(6.36643514249627,-2.30028979378828,82.5867477314601));
#29187=CARTESIAN_POINT('Ctrl Pts',(6.4215576252805,-2.13445231036017,82.5949468637696));
#29188=CARTESIAN_POINT('Ctrl Pts',(6.47669239949277,-1.96857784783767,82.6031478243539));
#29189=CARTESIAN_POINT('Ctrl Pts',(6.5253818746159,-1.80060835273854,82.6113487849383));
#29190=CARTESIAN_POINT('Ctrl Pts',(6.56748384468879,-1.63108704542453,82.6195497455226));
#29191=CARTESIAN_POINT('Ctrl Pts',(6.60962527443976,-1.46140685584918,82.6277583923806));
#29192=CARTESIAN_POINT('Ctrl Pts',(6.64516677720358,-1.29017229653161,82.6359670392386));
#29193=CARTESIAN_POINT('Ctrl Pts',(6.67401708183124,-1.11793782985677,82.6441756860966));
#29194=CARTESIAN_POINT('Ctrl Pts',(6.70288116040432,-0.945621133611937,
82.6523882519931));
#29195=CARTESIAN_POINT('Ctrl Pts',(6.72504762597267,-0.772303933532483,
82.6606008178896));
#29196=CARTESIAN_POINT('Ctrl Pts',(6.74047712353641,-0.598545860467189,
82.6688133837861));
#29197=CARTESIAN_POINT('Ctrl Pts',(6.75592779259387,-0.424549366290701,
82.6770372185062));
#29198=CARTESIAN_POINT('Ctrl Pts',(6.76462300101409,-0.250111148233967,
82.6852610532263));
#29199=CARTESIAN_POINT('Ctrl Pts',(6.76657554106495,-0.0757921306048062,
82.6934848879465));
#29200=CARTESIAN_POINT('Ctrl Pts',(6.76836955755702,0.0843742088110088,
82.7010410428687));
#29201=CARTESIAN_POINT('Ctrl Pts',(6.76447192498461,0.244439721655318,82.7085971977909));
#29202=CARTESIAN_POINT('Ctrl Pts',(6.75493109053418,0.403973962198986,82.716153352713));
#29203=CARTESIAN_POINT('Ctrl Pts',(6.74401451191755,0.586512301794816,82.7247990701999));
#29204=CARTESIAN_POINT('Ctrl Pts',(6.72568476538189,0.768771136426194,82.7334447876867));
#29205=CARTESIAN_POINT('Ctrl Pts',(6.69996462305992,0.950138437147746,82.7420905051736));
#29206=CARTESIAN_POINT('Ctrl Pts',(6.6742775001551,1.1312728992448,82.7507251233225));
#29207=CARTESIAN_POINT('Ctrl Pts',(6.64121894316698,1.3115178092047,82.7593597414714));
#29208=CARTESIAN_POINT('Ctrl Pts',(6.60086358361558,1.4902647249726,82.7679943596203));
#29209=CARTESIAN_POINT('Ctrl Pts',(6.55908302548745,1.67532430534764,82.776933919805));
#29210=CARTESIAN_POINT('Ctrl Pts',(6.50948085777193,1.85877783126783,82.7858734799897));
#29211=CARTESIAN_POINT('Ctrl Pts',(6.45219850249737,2.03995673590661,82.7948130401743));
#29212=CARTESIAN_POINT('Ctrl Pts',(6.39702369992608,2.21446964211677,82.8034236928945));
#29213=CARTESIAN_POINT('Ctrl Pts',(6.33472383417263,2.38687197320314,82.8120343456147));
#29214=CARTESIAN_POINT('Ctrl Pts',(6.26547711874044,2.55657690565725,82.8206449983349));
#29215=CARTESIAN_POINT('Ctrl Pts',(6.19629594990227,2.72612120117369,82.8292475005031));
#29216=CARTESIAN_POINT('Ctrl Pts',(6.12018115631522,2.89297290712752,82.8378500026712));
#29217=CARTESIAN_POINT('Ctrl Pts',(6.03736026261713,3.05656180362375,82.8464525048394));
#29218=CARTESIAN_POINT('Ctrl Pts',(5.95463258205344,3.2199665843357,82.8550453250764));
#29219=CARTESIAN_POINT('Ctrl Pts',(5.86521399602658,3.3801156100352,82.8636381453133));
#29220=CARTESIAN_POINT('Ctrl Pts',(5.76937957983948,3.5364598490201,82.8722309655503));
#29221=CARTESIAN_POINT('Ctrl Pts',(5.75808503033728,3.55488577382723,82.873243670979));
#29222=CARTESIAN_POINT('Ctrl Pts',(5.74670142053278,3.57325887594856,82.8742563764078));
#29223=CARTESIAN_POINT('Ctrl Pts',(5.7352292438198,3.59157827714143,82.8752690818365));
#29224=CARTESIAN_POINT('Ctrl Pts',(5.637860041778,3.74706276109426,82.8838643399086));
#29225=CARTESIAN_POINT('Ctrl Pts',(5.53422167700175,3.89849375004495,82.8924595979808));
#29226=CARTESIAN_POINT('Ctrl Pts',(5.42468356813408,4.04537973317909,82.9010548560529));
#29227=CARTESIAN_POINT('Ctrl Pts',(5.31504288136061,4.19240326895767,82.9096581632285));
#29228=CARTESIAN_POINT('Ctrl Pts',(5.19949160519025,4.33487305858242,82.9182614704041));
#29229=CARTESIAN_POINT('Ctrl Pts',(5.07843915550385,4.47233101903754,82.9268647775797));
#29230=CARTESIAN_POINT('Ctrl Pts',(4.95236783620994,4.61548802632587,82.9358247803614));
#29231=CARTESIAN_POINT('Ctrl Pts',(4.82032972472659,4.75320848801093,82.9447847831431));
#29232=CARTESIAN_POINT('Ctrl Pts',(4.68282829878418,4.88501874347541,82.9537447859248));
#29233=CARTESIAN_POINT('Ctrl Pts',(4.55043958001625,5.01192790621184,82.9623716294669));
#29234=CARTESIAN_POINT('Ctrl Pts',(4.41298675734103,5.13335829386179,82.970998473009));
#29235=CARTESIAN_POINT('Ctrl Pts',(4.27095204001356,5.24892919288344,82.9796253165512));
#29236=CARTESIAN_POINT('Ctrl Pts',(4.12878157333259,5.36461054852528,82.9882604051791));
#29237=CARTESIAN_POINT('Ctrl Pts',(3.98202071308302,5.47442105199867,82.9968954938071));
#29238=CARTESIAN_POINT('Ctrl Pts',(3.83118140321319,5.57802277296117,83.005530582435));
#29239=CARTESIAN_POINT('Ctrl Pts',(3.68011806664266,5.68177836330795,83.0141784959056));
#29240=CARTESIAN_POINT('Ctrl Pts',(3.52496443168327,5.77930657784367,83.0228264093763));
#29241=CARTESIAN_POINT('Ctrl Pts',(3.36625910512639,5.87031418555716,83.0314743228469));
#29242=CARTESIAN_POINT('Ctrl Pts',(3.34845481171687,5.88052383752905,83.0324444855512));
#29243=CARTESIAN_POINT('Ctrl Pts',(3.33060584155262,5.89065147415317,83.0334146482556));
#29244=CARTESIAN_POINT('Ctrl Pts',(3.3127129717843,5.90069671874195,83.03438481096));
#29245=CARTESIAN_POINT('Ctrl Pts',(3.24226969262992,5.94024431384009,83.038204290065));
#29246=CARTESIAN_POINT('Ctrl Pts',(3.17107508926453,5.97855445657467,83.0420237691701));
#29247=CARTESIAN_POINT('Ctrl Pts',(3.09917575053248,6.01559628526645,83.0458432482751));
#29248=CARTESIAN_POINT('Ctrl Pts',(3.09917575053255,6.01559628526641,81.0455808655427));
#29249=CARTESIAN_POINT('Ctrl Pts',(2.94387255360249,6.09560695737296,81.0537971731457));
#29250=CARTESIAN_POINT('Ctrl Pts',(2.78558799776598,6.16953832751457,81.0620134807487));
#29251=CARTESIAN_POINT('Ctrl Pts',(2.62484427732996,6.23718538443168,81.0702297883517));
#29252=CARTESIAN_POINT('Ctrl Pts',(2.46398711339998,6.30488018267562,81.0784518945429));
#29253=CARTESIAN_POINT('Ctrl Pts',(2.3006676600825,6.36628170274451,81.0866740007341));
#29254=CARTESIAN_POINT('Ctrl Pts',(2.13542368240621,6.42123467073262,81.0948961069253));
#29255=CARTESIAN_POINT('Ctrl Pts',(1.96995434617089,6.47626258318682,81.1031294263663));
#29256=CARTESIAN_POINT('Ctrl Pts',(1.80255558755721,6.5248242846923,81.1113627458073));
#29257=CARTESIAN_POINT('Ctrl Pts',(1.63377659615256,6.56681528854468,81.1195960652483));
#29258=CARTESIAN_POINT('Ctrl Pts',(1.5968775088955,6.57599551709247,81.1213960639919));
#29259=CARTESIAN_POINT('Ctrl Pts',(1.55991247486456,6.58486188688256,81.1231960627355));
#29260=CARTESIAN_POINT('Ctrl Pts',(1.52288726532626,6.59341363613016,81.1249960614791));
#29261=CARTESIAN_POINT('Ctrl Pts',(1.35516514076932,6.63215258103748,81.1331499549272));
#29262=CARTESIAN_POINT('Ctrl Pts',(1.18568915885699,6.66455107448763,81.1413038483754));
#29263=CARTESIAN_POINT('Ctrl Pts',(1.01498429781996,6.6904481072032,81.1494577418236));
#29264=CARTESIAN_POINT('Ctrl Pts',(0.844487744228896,6.71631353833046,81.1576016852521));
#29265=CARTESIAN_POINT('Ctrl Pts',(0.672765653975801,6.73569324650873,81.1657456286807));
#29266=CARTESIAN_POINT('Ctrl Pts',(0.500357038199068,6.74847626018827,81.1738895721092));
#29267=CARTESIAN_POINT('Ctrl Pts',(0.328122520375613,6.76124636560039,81.1820252917963));
#29268=CARTESIAN_POINT('Ctrl Pts',(0.15520321906578,6.76743301108239,81.1901610114834));
#29269=CARTESIAN_POINT('Ctrl Pts',(-0.017852813039725,6.76697645016344,
81.1982967311705));
#29270=CARTESIAN_POINT('Ctrl Pts',(-0.190770495782425,6.76652025424137,
81.2064259467697));
#29271=CARTESIAN_POINT('Ctrl Pts',(-0.363824327734731,6.75943142743707,
81.2145551623689));
#29272=CARTESIAN_POINT('Ctrl Pts',(-0.536462301573337,6.74570212794715,
81.2226843779682));
#29273=CARTESIAN_POINT('Ctrl Pts',(-0.708998559514368,6.73198091756989,
81.2308088039464));
#29274=CARTESIAN_POINT('Ctrl Pts',(-0.8811190837007,6.71162705495622,81.2389332299247));
#29275=CARTESIAN_POINT('Ctrl Pts',(-1.0522730425815,6.68468476772512,81.2470576559029));
#29276=CARTESIAN_POINT('Ctrl Pts',(-1.22446597091993,6.65757893058998,81.2552314002289));
#29277=CARTESIAN_POINT('Ctrl Pts',(-1.39568018537786,6.62380441962481,81.2634051445548));
#29278=CARTESIAN_POINT('Ctrl Pts',(-1.5653605731913,6.58345921806297,81.2715788888808));
#29279=CARTESIAN_POINT('Ctrl Pts',(-1.73395442124339,6.543372364954,81.2797002930493));
#29280=CARTESIAN_POINT('Ctrl Pts',(-1.90103367393275,6.49679883350736,81.2878216972178));
#29281=CARTESIAN_POINT('Ctrl Pts',(-2.06606496300445,6.44388582833723,81.2959431013864));
#29282=CARTESIAN_POINT('Ctrl Pts',(-2.23110901142692,6.39096873221201,81.3040651334591));
#29283=CARTESIAN_POINT('Ctrl Pts',(-2.39410443230724,6.33171129775786,81.3121871655319));
#29284=CARTESIAN_POINT('Ctrl Pts',(-2.55453415242879,6.26631025916168,81.3203091976047));
#29285=CARTESIAN_POINT('Ctrl Pts',(-2.71500682563224,6.20089171024282,81.3284334042515));
#29286=CARTESIAN_POINT('Ctrl Pts',(-2.87291209150143,6.12932642004497,81.3365576108983));
#29287=CARTESIAN_POINT('Ctrl Pts',(-3.02775399318628,6.05185878526131,81.3446818175451));
#29288=CARTESIAN_POINT('Ctrl Pts',(-3.18427188053063,5.97355265234789,81.3528939593935));
#29289=CARTESIAN_POINT('Ctrl Pts',(-3.33765935799626,5.88921582712286,81.3611061012419));
#29290=CARTESIAN_POINT('Ctrl Pts',(-3.48743157806289,5.79914735011362,81.3693182430903));
#29291=CARTESIAN_POINT('Ctrl Pts',(-3.63583660969516,5.70990105882087,81.3774554208008));
#29292=CARTESIAN_POINT('Ctrl Pts',(-3.78069184137684,5.61502757559133,81.3855925985113));
#29293=CARTESIAN_POINT('Ctrl Pts',(-3.92155680569367,5.51486003627632,81.3937297762218));
#29294=CARTESIAN_POINT('Ctrl Pts',(-4.06436835781731,5.41330829960881,81.4019794001391));
#29295=CARTESIAN_POINT('Ctrl Pts',(-4.20307824269482,5.30631535989489,81.4102290240565));
#29296=CARTESIAN_POINT('Ctrl Pts',(-4.33726443674413,5.19426859199201,81.4184786479738));
#29297=CARTESIAN_POINT('Ctrl Pts',(-4.47145063079335,5.08222182408921,81.4267282718911));
#29298=CARTESIAN_POINT('Ctrl Pts',(-4.60111289085595,4.96512153283837,81.4349778958085));
#29299=CARTESIAN_POINT('Ctrl Pts',(-4.72587030010071,4.84339126094785,81.4432275197258));
#29300=CARTESIAN_POINT('Ctrl Pts',(-4.84862596813934,4.72361415963656,81.4513447778604));
#29301=CARTESIAN_POINT('Ctrl Pts',(-4.967020259715,4.59897661286981,81.4594620359949));
#29302=CARTESIAN_POINT('Ctrl Pts',(-5.08063812871043,4.46983279386308,81.4675792941295));
#29303=CARTESIAN_POINT('Ctrl Pts',(-5.19412536666736,4.34083745670469,81.4756872195256));
#29304=CARTESIAN_POINT('Ctrl Pts',(-5.30284687153531,4.20734643475976,81.4837951449216));
#29305=CARTESIAN_POINT('Ctrl Pts',(-5.40642239704789,4.06975255570888,81.4919030703177));
#29306=CARTESIAN_POINT('Ctrl Pts',(-5.50990108083009,3.93228732509373,81.500003414912));
#29307=CARTESIAN_POINT('Ctrl Pts',(-5.60824314329255,3.79072716765027,81.5081037595063));
#29308=CARTESIAN_POINT('Ctrl Pts',(-5.70110683920205,3.64549993937782,81.5162041041006));
#29309=CARTESIAN_POINT('Ctrl Pts',(-5.79389713109863,3.50038750581859,81.5242980457859));
#29310=CARTESIAN_POINT('Ctrl Pts',(-5.88121748434763,3.35161408544836,81.5323919874712));
#29311=CARTESIAN_POINT('Ctrl Pts',(-5.96276803091265,3.19963848106721,81.5404859291564));
#29312=CARTESIAN_POINT('Ctrl Pts',(-6.04428338719127,3.04772845644327,81.5485763781842));
#29313=CARTESIAN_POINT('Ctrl Pts',(-6.12003371792392,2.89261932275003,81.556666827212));
#29314=CARTESIAN_POINT('Ctrl Pts',(-6.18976379603621,2.73479672906039,81.5647572762398));
#29315=CARTESIAN_POINT('Ctrl Pts',(-6.25947732487724,2.57701159193161,81.5728458051344));
#29316=CARTESIAN_POINT('Ctrl Pts',(-6.32317329671697,2.41651461460409,81.580934334029));
#29317=CARTESIAN_POINT('Ctrl Pts',(-6.38064360341805,2.25381370262947,81.5890228629236));
#29318=CARTESIAN_POINT('Ctrl Pts',(-6.43811142968165,2.0911198128801,81.5971110427147));
#29319=CARTESIAN_POINT('Ctrl Pts',(-6.48935400421463,1.92622252658037,81.6051992225057));
#29320=CARTESIAN_POINT('Ctrl Pts',(-6.53421233085119,1.75964718490734,81.6132874022967));
#29321=CARTESIAN_POINT('Ctrl Pts',(-6.57909237290122,1.59299120597718,81.621379497485));
#29322=CARTESIAN_POINT('Ctrl Pts',(-6.61758189679574,1.42465590580469,81.6294715926733));
#29323=CARTESIAN_POINT('Ctrl Pts',(-6.64957240512015,1.25517960032207,81.6375636878615));
#29324=CARTESIAN_POINT('Ctrl Pts',(-6.68157167014302,1.08565690442609,81.645657998083));
#29325=CARTESIAN_POINT('Ctrl Pts',(-6.707068317244,0.914992945643581,81.6537523083045));
#29326=CARTESIAN_POINT('Ctrl Pts',(-6.72600549102029,0.743733241669988,
81.6618466185259));
#29327=CARTESIAN_POINT('Ctrl Pts',(-6.74495917228062,0.572324251067659,
81.6699479845361));
#29328=CARTESIAN_POINT('Ctrl Pts',(-6.75734193290791,0.400318846176341,
81.6780493505463));
#29329=CARTESIAN_POINT('Ctrl Pts',(-6.76314897039875,0.228265205833898,
81.6861507165564));
#29330=CARTESIAN_POINT('Ctrl Pts',(-6.76578417235999,0.150188201649751,
81.6898270722942));
#29331=CARTESIAN_POINT('Ctrl Pts',(-6.76706595052292,0.0721012471304621,
81.6935034280319));
#29332=CARTESIAN_POINT('Ctrl Pts',(-6.76699738887189,-0.00594466156220883,
81.6971797837697));
#29333=CARTESIAN_POINT('',(-6.767,4.06094923584722E-12,81.3028202161898));
#29334=CARTESIAN_POINT('Ctrl Pts',(3.09917575053259,6.01559628526639,80.651216691749));
#29335=CARTESIAN_POINT('Ctrl Pts',(2.94383946288018,6.09562400538604,80.659430820505));
#29336=CARTESIAN_POINT('Ctrl Pts',(2.7855089613724,6.16957580012018,80.6676449492608));
#29337=CARTESIAN_POINT('Ctrl Pts',(2.62470545272606,6.2372438052741,80.6758590780168));
#29338=CARTESIAN_POINT('Ctrl Pts',(2.46368391518074,6.30500355954956,80.684084344076));
#29339=CARTESIAN_POINT('Ctrl Pts',(2.30018300496955,6.36646237140818,80.6923096101353));
#29340=CARTESIAN_POINT('Ctrl Pts',(2.13474098897898,6.42146166460356,80.7005348761945));
#29341=CARTESIAN_POINT('Ctrl Pts',(1.99084271420704,6.46929898910123,80.7076890539793));
#29342=CARTESIAN_POINT('Ctrl Pts',(1.84547632817944,6.51225032196516,80.714843231764));
#29343=CARTESIAN_POINT('Ctrl Pts',(1.69900208345931,6.55024281385056,80.7219974095488));
#29344=CARTESIAN_POINT('Ctrl Pts',(1.52198592333032,6.59615726823219,80.730643332815));
#29345=CARTESIAN_POINT('Ctrl Pts',(1.34294978917248,6.63493281563262,80.7392892560813));
#29346=CARTESIAN_POINT('Ctrl Pts',(1.16248299663846,6.66640249928899,80.7479351793476));
#29347=CARTESIAN_POINT('Ctrl Pts',(0.982247045968157,6.69783192888907,80.7565700432882));
#29348=CARTESIAN_POINT('Ctrl Pts',(0.800584385052222,6.72197407749631,80.7652049072287));
#29349=CARTESIAN_POINT('Ctrl Pts',(0.61809689604195,6.73871243095469,80.7738397711693));
#29350=CARTESIAN_POINT('Ctrl Pts',(0.429549570213807,6.75600661260222,80.7827613718429));
#29351=CARTESIAN_POINT('Ctrl Pts',(0.24012199781765,6.76539672476705,80.7916829725165));
#29352=CARTESIAN_POINT('Ctrl Pts',(0.0504896816497254,6.76681164153746,
80.8006045731902));
#29353=CARTESIAN_POINT('Ctrl Pts',(-0.132541039503159,6.76817730136851,
80.809215589699));
#29354=CARTESIAN_POINT('Ctrl Pts',(-0.315762144546805,6.76211363697309,
80.8178266062079));
#29355=CARTESIAN_POINT('Ctrl Pts',(-0.498560400104501,6.74860922912622,
80.8264376227167));
#29356=CARTESIAN_POINT('Ctrl Pts',(-0.681186277478519,6.73511755589375,
80.8350405190639));
#29357=CARTESIAN_POINT('Ctrl Pts',(-0.863389797227727,6.71419915086027,
80.8436434154111));
#29358=CARTESIAN_POINT('Ctrl Pts',(-1.04455831853247,6.68589462369731,80.8522463117583));
#29359=CARTESIAN_POINT('Ctrl Pts',(-1.2255239892674,6.65762178851607,80.860839575624));
#29360=CARTESIAN_POINT('Ctrl Pts',(-1.40545667279565,6.62197937676768,80.8694328394897));
#29361=CARTESIAN_POINT('Ctrl Pts',(-1.58374922023413,6.57905976621339,80.8780261033554));
#29362=CARTESIAN_POINT('Ctrl Pts',(-1.6036179751965,6.57427684489988,80.8789837286545));
#29363=CARTESIAN_POINT('Ctrl Pts',(-1.62346636815287,6.56940360340689,80.8799413539537));
#29364=CARTESIAN_POINT('Ctrl Pts',(-1.64329356408214,6.56444020935877,80.8808989792528));
#29365=CARTESIAN_POINT('Ctrl Pts',(-1.82126542019569,6.51988804704001,80.889494766199));
#29366=CARTESIAN_POINT('Ctrl Pts',(-1.99731995182512,6.46812021392288,80.8980905531452));
#29367=CARTESIAN_POINT('Ctrl Pts',(-2.1708754615811,6.40933606002253,80.9066863400914));
#29368=CARTESIAN_POINT('Ctrl Pts',(-2.3445929232905,6.35049705215316,80.9152901481283));
#29369=CARTESIAN_POINT('Ctrl Pts',(-2.51580641932027,6.28462875294149,80.9238939561653));
#29370=CARTESIAN_POINT('Ctrl Pts',(-2.68395367229331,6.21197888639226,80.9324977642022));
#29371=CARTESIAN_POINT('Ctrl Pts',(-2.85870835083578,6.13647420909016,80.9414396629317));
#29372=CARTESIAN_POINT('Ctrl Pts',(-3.03015059433496,6.05364437954267,80.9503815616612));
#29373=CARTESIAN_POINT('Ctrl Pts',(-3.19767795007734,5.96381964244302,80.9593234603907));
#29374=CARTESIAN_POINT('Ctrl Pts',(-3.35931003947585,5.87715582641876,80.9679506948411));
#29375=CARTESIAN_POINT('Ctrl Pts',(-3.51729784406443,5.7839812063096,80.9765779292915));
#29376=CARTESIAN_POINT('Ctrl Pts',(-3.67113009209778,5.68463656242808,80.9852051637419));
#29377=CARTESIAN_POINT('Ctrl Pts',(-3.82510885017376,5.58519730257237,80.9938406147821));
#29378=CARTESIAN_POINT('Ctrl Pts',(-3.97492390079849,5.47957646234283,81.0024760658224));
#29379=CARTESIAN_POINT('Ctrl Pts',(-4.12009545277081,5.36815633714754,81.0111115168626));
#29380=CARTESIAN_POINT('Ctrl Pts',(-4.26548148184185,5.25657159936208,81.0197597259567));
#29381=CARTESIAN_POINT('Ctrl Pts',(-4.40621006613223,5.1391706470642,81.0284079350509));
#29382=CARTESIAN_POINT('Ctrl Pts',(-4.54183567309202,5.01637495793813,81.037056144145));
#29383=CARTESIAN_POINT('Ctrl Pts',(-4.55618205641998,5.00338571448542,81.0379709457488));
#29384=CARTESIAN_POINT('Ctrl Pts',(-4.57047137642931,4.99033614058141,81.0388857473526));
#29385=CARTESIAN_POINT('Ctrl Pts',(-4.58470313105571,4.97722675795347,81.0398005489564));
#29386=CARTESIAN_POINT('Ctrl Pts',(-4.71032631150992,4.86151071430702,81.0478754694404));
#29387=CARTESIAN_POINT('Ctrl Pts',(-4.83176307243518,4.74085362904437,81.0559503899244));
#29388=CARTESIAN_POINT('Ctrl Pts',(-4.94859208424996,4.61559588609083,81.0640253104084));
#29389=CARTESIAN_POINT('Ctrl Pts',(-5.06529578359498,4.49047249638468,81.0720915696171));
#29390=CARTESIAN_POINT('Ctrl Pts',(-5.17740131799069,4.36075854015743,81.0801578288258));
#29391=CARTESIAN_POINT('Ctrl Pts',(-5.28452114638662,4.22683395148103,81.0882240880345));
#29392=CARTESIAN_POINT('Ctrl Pts',(-5.39154949671538,4.09302373156997,81.0962834588285));
#29393=CARTESIAN_POINT('Ctrl Pts',(-5.49360038454914,3.95501032620842,81.1043428296225));
#29394=CARTESIAN_POINT('Ctrl Pts',(-5.59032388366367,3.81320965536115,81.1124022004165));
#29395=CARTESIAN_POINT('Ctrl Pts',(-5.68698497174893,3.67150048167745,81.1204563708855));
#29396=CARTESIAN_POINT('Ctrl Pts',(-5.7783253060897,3.52600921521733,81.1285105413546));
#29397=CARTESIAN_POINT('Ctrl Pts',(-5.86403602602228,3.37718380984999,81.1365647118237));
#29398=CARTESIAN_POINT('Ctrl Pts',(-5.94971711686435,3.22840985150594,81.1446160980698));
#29399=CARTESIAN_POINT('Ctrl Pts',(-6.02977227964826,3.07630437018704,81.152667484316));
#29400=CARTESIAN_POINT('Ctrl Pts',(-6.10393667416835,2.92134319752792,81.1607188705622));
#29401=CARTESIAN_POINT('Ctrl Pts',(-6.17809008621871,2.76640497195007,81.1687690645367));
#29402=CARTESIAN_POINT('Ctrl Pts',(-6.24635430532472,2.60861223298746,81.1768192585112));
#29403=CARTESIAN_POINT('Ctrl Pts',(-6.308511115388,2.44846411185176,81.1848694524858));
#29404=CARTESIAN_POINT('Ctrl Pts',(-6.37067100353014,2.28830805999141,81.1929200451154));
#29405=CARTESIAN_POINT('Ctrl Pts',(-6.4267227466436,2.12579674180012,81.2009706377451));
#29406=CARTESIAN_POINT('Ctrl Pts',(-6.47649686715468,1.96144776370305,81.2090212303748));
#29407=CARTESIAN_POINT('Ctrl Pts',(-6.52630621734081,1.7969824608767,81.2170775211415));
#29408=CARTESIAN_POINT('Ctrl Pts',(-6.56982895997579,1.63067725702817,81.2251338119083));
#29409=CARTESIAN_POINT('Ctrl Pts',(-6.60694580497785,1.46306395283513,81.233190102675));
#29410=CARTESIAN_POINT('Ctrl Pts',(-6.64407584250108,1.29539107347988,81.2412492569068));
#29411=CARTESIAN_POINT('Ctrl Pts',(-6.67479537818248,1.12640953403713,81.2493084111385));
#29412=CARTESIAN_POINT('Ctrl Pts',(-6.69903664510372,0.956659305896044,
81.2573675653703));
#29413=CARTESIAN_POINT('Ctrl Pts',(-6.72330692248817,0.786705931081017,
81.2654363643041));
#29414=CARTESIAN_POINT('Ctrl Pts',(-6.74108340262473,0.615982400497209,
81.2735051632379));
#29415=CARTESIAN_POINT('Ctrl Pts',(-6.7523503267723,0.445032655586101,81.2815739621717));
#29416=CARTESIAN_POINT('Ctrl Pts',(-6.7621241711247,0.29673697373359,81.2885734931757));
#29417=CARTESIAN_POINT('Ctrl Pts',(-6.76700025229275,0.148271235916897,
81.2955730241797));
#29418=CARTESIAN_POINT('Ctrl Pts',(-6.76699999999021,-1.15140253983646E-5,
81.3025725551836));
#29419=CARTESIAN_POINT('Ctrl Pts',(-6.767,4.06094923160091E-12,81.3028202161898));
#29420=CARTESIAN_POINT('Ctrl Pts',(-6.76700000000011,-0.186007249411735,
81.3115697279958));
#29421=CARTESIAN_POINT('Ctrl Pts',(-6.75932637295459,-0.372014355523709,
81.3203192398017));
#29422=CARTESIAN_POINT('Ctrl Pts',(-6.74400518266958,-0.55738953715135,
81.3290687516077));
#29423=CARTESIAN_POINT('Ctrl Pts',(-6.72868405709685,-0.742763935807834,
81.3378182264582));
#29424=CARTESIAN_POINT('Ctrl Pts',(-6.70571545653039,-0.927506129691614,
81.3465677013088));
#29425=CARTESIAN_POINT('Ctrl Pts',(-6.67517739415705,-1.11098863924648,
81.3553171761593));
#29426=CARTESIAN_POINT('Ctrl Pts',(-6.6446394582313,-1.29447038906349,81.3640666147813));
#29427=CARTESIAN_POINT('Ctrl Pts',(-6.60653217027189,-1.47669218228075,
81.3728160534033));
#29428=CARTESIAN_POINT('Ctrl Pts',(-6.56098496116745,-1.65703510503991,
81.3815654920253));
#29429=CARTESIAN_POINT('Ctrl Pts',(-6.51543793687553,-1.83737729603892,
81.3903148951455));
#29430=CARTESIAN_POINT('Ctrl Pts',(-6.46245112202678,-2.01584035396928,
81.3990642982657));
#29431=CARTESIAN_POINT('Ctrl Pts',(-6.40220448416285,-2.1918181363802,81.407813701386));
#29432=CARTESIAN_POINT('Ctrl Pts',(-6.34195808575226,-2.36779521935841,
81.4165630697313));
#29433=CARTESIAN_POINT('Ctrl Pts',(-6.27445201489269,-2.54128677544744,
81.4253124380765));
#29434=CARTESIAN_POINT('Ctrl Pts',(-6.19991555136212,-2.71170355237777,
81.4340618064218));
#29435=CARTESIAN_POINT('Ctrl Pts',(-6.12537937789079,-2.88211966612984,
81.4428111407189));
#29436=CARTESIAN_POINT('Ctrl Pts',(-6.04381298133671,-3.04946076210335,
81.4515604750159));
#29437=CARTESIAN_POINT('Ctrl Pts',(-5.95549339426377,-3.21315848206723,
81.4603098093129));
#29438=CARTESIAN_POINT('Ctrl Pts',(-5.86717414355229,-3.37685557859519,
81.4690591102885));
#29439=CARTESIAN_POINT('Ctrl Pts',(-5.77210188986302,-3.53690907467208,
81.4778084112641));
#29440=CARTESIAN_POINT('Ctrl Pts',(-5.67059953467127,-3.69277536784814,
81.4865577122397));
#29441=CARTESIAN_POINT('Ctrl Pts',(-5.56909755761821,-3.84864108035713,
81.4953069806204));
#29442=CARTESIAN_POINT('Ctrl Pts',(-5.46116568338121,-4.0003193810421,81.5040562490012));
#29443=CARTESIAN_POINT('Ctrl Pts',(-5.34717048686161,-4.14729511663159,
81.512805517382));
#29444=CARTESIAN_POINT('Ctrl Pts',(-5.23317570555567,-4.2942703168798,81.5215547538946));
#29445=CARTESIAN_POINT('Ctrl Pts',(-5.11311782178858,-4.43654275987068,
81.5303039904072));
#29446=CARTESIAN_POINT('Ctrl Pts',(-4.98740459172071,-4.57362924147588,
81.5390532269198));
#29447=CARTESIAN_POINT('Ctrl Pts',(-4.86169180910878,-4.71071523514387,
81.5478024322909));
#29448=CARTESIAN_POINT('Ctrl Pts',(-4.73032391415469,-4.84261509316487,
81.5565516376621));
#29449=CARTESIAN_POINT('Ctrl Pts',(-4.5937470723732,-4.96888084331499,81.5653008430332));
#29450=CARTESIAN_POINT('Ctrl Pts',(-4.45717070537429,-5.09514615452701,
81.5740500179894));
#29451=CARTESIAN_POINT('Ctrl Pts',(-4.31538563819536,-5.21577720253611,
81.5827991929456));
#29452=CARTESIAN_POINT('Ctrl Pts',(-4.16887341290675,-5.33036429028629,
81.5915483679019));
#29453=CARTESIAN_POINT('Ctrl Pts',(-4.02236168477388,-5.44495098921139,
81.6002975131698));
#29454=CARTESIAN_POINT('Ctrl Pts',(-3.87112305634513,-5.55349359238706,
81.6090466584377));
#29455=CARTESIAN_POINT('Ctrl Pts',(-3.71567117316832,-5.65562346102408,
81.6177958037056));
#29456=CARTESIAN_POINT('Ctrl Pts',(-3.56021980457387,-5.75775299158717,
81.6265449200118));
#29457=CARTESIAN_POINT('Ctrl Pts',(-3.40055544862459,-5.85346967275312,
81.6352940363179));
#29458=CARTESIAN_POINT('Ctrl Pts',(-3.23722036323458,-5.94244842803531,
81.6440431526241));
#29459=CARTESIAN_POINT('Ctrl Pts',(-3.07388580496141,-6.03142689616426,
81.652792240695));
#29460=CARTESIAN_POINT('Ctrl Pts',(-2.90688079257841,-6.11366734484757,
81.6615413287659));
#29461=CARTESIAN_POINT('Ctrl Pts',(-2.73677251094791,-6.18889046787224,
81.6702904168369));
#29462=CARTESIAN_POINT('Ctrl Pts',(-2.5666647641681,-6.26411335438203,81.6790394773991));
#29463=CARTESIAN_POINT('Ctrl Pts',(-2.39345402972247,-6.33231884350233,
81.6877885379614));
#29464=CARTESIAN_POINT('Ctrl Pts',(-2.2177285647418,-6.39327529620994,81.6965375985236));
#29465=CARTESIAN_POINT('Ctrl Pts',(-2.04200363768409,-6.45423156232038,
81.7052866323036));
#29466=CARTESIAN_POINT('Ctrl Pts',(-1.86376426620231,-6.50793874252016,
81.7140356660836));
#29467=CARTESIAN_POINT('Ctrl Pts',(-1.68361578194824,-6.55421443796088,
81.7227846998636));
#29468=CARTESIAN_POINT('Ctrl Pts',(-1.50346783420042,-6.60048999558639,
81.7315337075878));
#29469=CARTESIAN_POINT('Ctrl Pts',(-1.3214110625746,-6.63933404145452,81.740282715312));
#29470=CARTESIAN_POINT('Ctrl Pts',(-1.13806375959297,-6.67061465526987,
81.7490317230362));
#29471=CARTESIAN_POINT('Ctrl Pts',(-0.95471698742188,-6.70189517852441,
81.7577807054311));
#29472=CARTESIAN_POINT('Ctrl Pts',(-0.770079973812807,-6.72561226535794,
81.766529687826));
#29473=CARTESIAN_POINT('Ctrl Pts',(-0.584779770555591,-6.74168536939755,
81.7752786702209));
#29474=CARTESIAN_POINT('Ctrl Pts',(-0.391490647557044,-6.75845143942376,
81.7844048508969));
#29475=CARTESIAN_POINT('Ctrl Pts',(-0.197480213107461,-6.76689975924017,
81.793531031573));
#29476=CARTESIAN_POINT('Ctrl Pts',(-0.00346532630091309,-6.76699911271707,
81.802657212249));
#29477=CARTESIAN_POINT('Ctrl Pts',(0.184486595292899,-6.76709536139782,
81.8114981997789));
#29478=CARTESIAN_POINT('Ctrl Pts',(0.372442378182036,-6.75935659726787,
81.8203391873089));
#29479=CARTESIAN_POINT('Ctrl Pts',(0.55975021771886,-6.74380965729043,81.8291801748388));
#29480=CARTESIAN_POINT('Ctrl Pts',(0.745129914454533,-6.72842275717289,
81.8379301534366));
#29481=CARTESIAN_POINT('Ctrl Pts',(0.929874656310971,-6.70538772273517,
81.8466801320343));
#29482=CARTESIAN_POINT('Ctrl Pts',(1.11335688289457,-6.67478280180796,81.8554301106321));
#29483=CARTESIAN_POINT('Ctrl Pts',(1.29683723118525,-6.64417819418088,81.864179999657));
#29484=CARTESIAN_POINT('Ctrl Pts',(1.47905480729892,-6.60600390230151,81.872929888682));
#29485=CARTESIAN_POINT('Ctrl Pts',(1.65939064804455,-6.56038959797224,81.8816797777069));
#29486=CARTESIAN_POINT('Ctrl Pts',(1.83972470263919,-6.51477574543354,81.8904295800679));
#29487=CARTESIAN_POINT('Ctrl Pts',(2.0181767812551,-6.46172209820206,81.8991793824288));
#29488=CARTESIAN_POINT('Ctrl Pts',(2.1941407234735,-6.40140886724127,81.9079291847898));
#29489=CARTESIAN_POINT('Ctrl Pts',(2.37010298131777,-6.34109621361494,81.9166789033953));
#29490=CARTESIAN_POINT('Ctrl Pts',(2.54357687926603,-6.27352420826097,81.9254286220008));
#29491=CARTESIAN_POINT('Ctrl Pts',(2.71397317789672,-6.19892237325628,81.9341783406062));
#29492=CARTESIAN_POINT('Ctrl Pts',(2.8843679020691,-6.12432122757101,81.9429279783645));
#29493=CARTESIAN_POINT('Ctrl Pts',(3.05168482125974,-6.0426904971756,81.9516776161228));
#29494=CARTESIAN_POINT('Ctrl Pts',(3.21535561997114,-5.95430745235078,81.960427253881));
#29495=CARTESIAN_POINT('Ctrl Pts',(3.37902496075009,-5.86592519481673,81.9691768137));
#29496=CARTESIAN_POINT('Ctrl Pts',(3.53904799384607,-5.77079087940396,81.9779263735191));
#29497=CARTESIAN_POINT('Ctrl Pts',(3.6948811881472,-5.66922763747197,81.9866759333381));
#29498=CARTESIAN_POINT('Ctrl Pts',(3.85071304610564,-5.56766526649237,81.9954254181255));
#29499=CARTESIAN_POINT('Ctrl Pts',(4.00235489705696,-5.45967423580913,82.004174902913));
#29500=CARTESIAN_POINT('Ctrl Pts',(4.14929168607379,-5.34562133936542,82.0129243877004));
#29501=CARTESIAN_POINT('Ctrl Pts',(4.29622726385489,-5.23156938308751,82.0216738003637));
#29502=CARTESIAN_POINT('Ctrl Pts',(4.43845763091805,-5.1114558367743,82.030423213027));
#29503=CARTESIAN_POINT('Ctrl Pts',(4.57549970660707,-4.98568866204446,82.0391726256903));
#29504=CARTESIAN_POINT('Ctrl Pts',(4.71254069815039,-4.85992248226409,82.0479219691366));
#29505=CARTESIAN_POINT('Ctrl Pts',(4.84439326931058,-4.72850295734264,82.0566713125829));
#29506=CARTESIAN_POINT('Ctrl Pts',(4.97060959434444,-4.59187644221957,82.0654206560292));
#29507=CARTESIAN_POINT('Ctrl Pts',(5.09682496280273,-4.45525096256941,82.0741699331655));
#29508=CARTESIAN_POINT('Ctrl Pts',(5.21740397615609,-4.31341878218604,82.0829192103018));
#29509=CARTESIAN_POINT('Ctrl Pts',(5.33193710451716,-4.16686161438956,82.0916684874381));
#29510=CARTESIAN_POINT('Ctrl Pts',(5.44646940289169,-4.02030550864803,82.1004177011711));
#29511=CARTESIAN_POINT('Ctrl Pts',(5.55495572749456,-3.86902470980433,82.1091669149041));
#29512=CARTESIAN_POINT('Ctrl Pts',(5.65702762491252,-3.71353301466092,82.117916128637));
#29513=CARTESIAN_POINT('Ctrl Pts',(5.7590988165496,-3.55804239467207,82.1266652818731));
#29514=CARTESIAN_POINT('Ctrl Pts',(5.85475551250599,-3.39834117619869,82.1354144351093));
#29515=CARTESIAN_POINT('Ctrl Pts',(5.94367283727921,-3.23497174692288,82.1441635883454));
#29516=CARTESIAN_POINT('Ctrl Pts',(6.03258957676142,-3.07160339301297,82.1529126839909));
#29517=CARTESIAN_POINT('Ctrl Pts',(6.11476689685121,-2.90456712829848,82.1616617796364));
#29518=CARTESIAN_POINT('Ctrl Pts',(6.18992570525104,-2.73443024476261,82.1704108752819));
#29519=CARTESIAN_POINT('Ctrl Pts',(6.26508404388558,-2.56429442463373,82.179159916243));
#29520=CARTESIAN_POINT('Ctrl Pts',(6.33322384283191,-2.39105828656321,82.187908957204));
#29521=CARTESIAN_POINT('Ctrl Pts',(6.39411368719924,-2.21531017132395,82.1966579981651));
#29522=CARTESIAN_POINT('Ctrl Pts',(6.45500317120789,-2.03956309619835,82.2054069873475));
#29523=CARTESIAN_POINT('Ctrl Pts',(6.5086426926998,-1.86130434438959,82.2141559765299));
#29524=CARTESIAN_POINT('Ctrl Pts',(6.55485008446248,-1.68113930720276,82.2229049657123));
#29525=CARTESIAN_POINT('Ctrl Pts',(6.60199664749329,-1.49731239212169,82.2318317792416));
#29526=CARTESIAN_POINT('Ctrl Pts',(6.64140563640842,-1.31150116499997,82.240758592771));
#29527=CARTESIAN_POINT('Ctrl Pts',(6.67293772282118,-1.12436255155982,82.2496854063004));
#29528=CARTESIAN_POINT('Ctrl Pts',(6.70384494949825,-0.940932395054639,
82.2584353204559));
#29529=CARTESIAN_POINT('Ctrl Pts',(6.72718449348892,-0.756227260510083,
82.2671852346114));
#29530=CARTESIAN_POINT('Ctrl Pts',(6.74287707373903,-0.57087456454513,82.2759351487669));
#29531=CARTESIAN_POINT('Ctrl Pts',(6.7585693453865,-0.385525513636003,82.2846848908509));
#29532=CARTESIAN_POINT('Ctrl Pts',(6.76661493004092,-0.199529212421841,
82.2934346329349));
#29533=CARTESIAN_POINT('Ctrl Pts',(6.76698649908906,-0.0135174386041215,
82.3021843750189));
#29534=CARTESIAN_POINT('Ctrl Pts',(6.76735806132399,0.172490924442033,82.3109339566648));
#29535=CARTESIAN_POINT('Ctrl Pts',(6.76005588896309,0.358514472897615,82.3196835383107));
#29536=CARTESIAN_POINT('Ctrl Pts',(6.74510478454615,0.543921359658378,82.3284331199566));
#29537=CARTESIAN_POINT('Ctrl Pts',(6.73015393440729,0.729325093146674,82.3371825527956));
#29538=CARTESIAN_POINT('Ctrl Pts',(6.70755443556948,0.914111900252648,82.3459319856346));
#29539=CARTESIAN_POINT('Ctrl Pts',(6.67738304682378,1.09765415591175,82.3546814184737));
#29540=CARTESIAN_POINT('Ctrl Pts',(6.64721213111929,1.28119353390919,82.363430714135));
#29541=CARTESIAN_POINT('Ctrl Pts',(6.60946960955571,1.46348811672309,82.3721800097964));
#29542=CARTESIAN_POINT('Ctrl Pts',(6.56428366991267,1.64391876347888,82.3809293054577));
#29543=CARTESIAN_POINT('Ctrl Pts',(6.51909837867808,1.82434682109394,82.3896784755685));
#29544=CARTESIAN_POINT('Ctrl Pts',(6.46646995272017,2.00291071820135,82.3984276456794));
#29545=CARTESIAN_POINT('Ctrl Pts',(6.4065771328165,2.17900400212406,82.4071768157902));
#29546=CARTESIAN_POINT('Ctrl Pts',(6.34668509279169,2.35509499309363,82.415925871976));
#29547=CARTESIAN_POINT('Ctrl Pts',(6.27952894037644,2.52871516397829,82.4246749281617));
#29548=CARTESIAN_POINT('Ctrl Pts',(6.20533675061573,2.69927486771129,82.4334239843475));
#29549=CARTESIAN_POINT('Ctrl Pts',(6.12832117908046,2.87632521635649,82.4425059856298));
#29550=CARTESIAN_POINT('Ctrl Pts',(6.0437236662621,3.0500772891974,82.4515879869121));
#29551=CARTESIAN_POINT('Ctrl Pts',(5.95185378007998,3.21989527477954,82.4606699881943));
#29552=CARTESIAN_POINT('Ctrl Pts',(5.86334450817511,3.3835012928651,82.4694197685015));
#29553=CARTESIAN_POINT('Ctrl Pts',(5.76808562057404,3.5434556712472,82.4781695488086));
#29554=CARTESIAN_POINT('Ctrl Pts',(5.66640068804642,3.69921508465067,82.4869193291157));
#29555=CARTESIAN_POINT('Ctrl Pts',(5.56471941108085,3.85496889852051,82.4956687948692));
#29556=CARTESIAN_POINT('Ctrl Pts',(5.45661270815278,4.00652780919414,82.5044182606227));
#29557=CARTESIAN_POINT('Ctrl Pts',(5.3424477644928,4.15337704569015,82.5131677263762));
#29558=CARTESIAN_POINT('Ctrl Pts',(5.22828631819768,4.30022178356039,82.5219169240957));
#29559=CARTESIAN_POINT('Ctrl Pts',(5.10806717844249,4.44235690972472,82.5306661218154));
#29560=CARTESIAN_POINT('Ctrl Pts',(4.98219864544905,4.57929969070442,82.539415319535));
#29561=CARTESIAN_POINT('Ctrl Pts',(4.85633329944209,4.71623900429811,82.5481642957252));
#29562=CARTESIAN_POINT('Ctrl Pts',(4.7248190403383,4.8479860248344,82.5569132719154));
#29563=CARTESIAN_POINT('Ctrl Pts',(4.58810250737377,4.97409332258961,82.5656622481057));
#29564=CARTESIAN_POINT('Ctrl Pts',(4.45137708685819,5.10020881821981,82.5744117930418));
#29565=CARTESIAN_POINT('Ctrl Pts',(4.30944892636227,5.22068366307788,82.583161337978));
#29566=CARTESIAN_POINT('Ctrl Pts',(4.16280009466835,5.33510865604715,82.5919108829142));
#29567=CARTESIAN_POINT('Ctrl Pts',(4.01615988348973,5.44952692272755,82.6006599135225));
#29568=CARTESIAN_POINT('Ctrl Pts',(3.86479978232426,5.5578958728849,82.6094089441308));
#29569=CARTESIAN_POINT('Ctrl Pts',(3.70923383581274,5.65984746713743,82.618157974739));
#29570=CARTESIAN_POINT('Ctrl Pts',(3.55366577799753,5.76180044505251,82.6269071240871));
#29571=CARTESIAN_POINT('Ctrl Pts',(3.3938920002706,5.85733573570932,82.6356562734351));
#29572=CARTESIAN_POINT('Ctrl Pts',(3.23045513626267,5.94612887621805,82.6444054227831));
#29573=CARTESIAN_POINT('Ctrl Pts',(3.18695122151726,5.9697639920661,82.6467342868961));
#29574=CARTESIAN_POINT('Ctrl Pts',(3.14318791262733,5.99292165435297,82.6490631510091));
#29575=CARTESIAN_POINT('Ctrl Pts',(3.09917575053247,6.01559628526645,82.6513920151221));
#29576=CARTESIAN_POINT('Origin',(0.,0.,-3.69717978381041));
#29577=CARTESIAN_POINT('',(3.09917575053258,6.01559628526639,85.045900138346));
#29578=CARTESIAN_POINT('',(3.0991757505325,6.01559628526643,84.6515000956437));
#29579=CARTESIAN_POINT('',(3.09917575053259,6.01559628526639,-3.69717978381041));
#29580=CARTESIAN_POINT('',(-6.76699958812818,0.00236098985609753,83.697179783854));
#29581=CARTESIAN_POINT('Ctrl Pts',(-6.76699958812818,0.00236098985609753,
83.697179783854));
#29582=CARTESIAN_POINT('Ctrl Pts',(-6.76705954036394,-0.169472342533521,
83.7053053883323));
#29583=CARTESIAN_POINT('Ctrl Pts',(-6.76057027671101,-0.341565259567424,
83.7134309928107));
#29584=CARTESIAN_POINT('Ctrl Pts',(-6.7474986903799,-0.513371623019327,
83.721556597289));
#29585=CARTESIAN_POINT('Ctrl Pts',(-6.73444109820115,-0.684994054363445,
83.7296735026742));
#29586=CARTESIAN_POINT('Ctrl Pts',(-6.714815238025,-0.856330178927854,83.7377904080594));
#29587=CARTESIAN_POINT('Ctrl Pts',(-6.68863998106626,-1.02683212049583,
83.7459073134446));
#29588=CARTESIAN_POINT('Ctrl Pts',(-6.66248716249329,-1.19718790157549,
83.7540172607222));
#29589=CARTESIAN_POINT('Ctrl Pts',(-6.62979617995887,-1.3667105614629,83.7621272079997));
#29590=CARTESIAN_POINT('Ctrl Pts',(-6.59063783953794,-1.53485565055829,
83.7702371552773));
#29591=CARTESIAN_POINT('Ctrl Pts',(-6.5515047181622,-1.70289244960474,83.7783418795264));
#29592=CARTESIAN_POINT('Ctrl Pts',(-6.50591261572719,-1.86955308703234,
83.7864466037756));
#29593=CARTESIAN_POINT('Ctrl Pts',(-6.4539837074203,-2.03430167486372,83.7945513280247));
#29594=CARTESIAN_POINT('Ctrl Pts',(-6.40205093456113,-2.19906252329428,
83.8026566554278));
#29595=CARTESIAN_POINT('Ctrl Pts',(-6.34378049746849,-2.36191067871605,
83.810761982831));
#29596=CARTESIAN_POINT('Ctrl Pts',(-6.27934513209687,-2.5223230784361,83.8188673102341));
#29597=CARTESIAN_POINT('Ctrl Pts',(-6.21494644312632,-2.68264417193828,
83.8269680241112));
#29598=CARTESIAN_POINT('Ctrl Pts',(-6.14438997264112,-2.84053193721467,
83.8350687379883));
#29599=CARTESIAN_POINT('Ctrl Pts',(-6.06789701064579,-2.99548240992932,
83.8431694518654));
#29600=CARTESIAN_POINT('Ctrl Pts',(-5.99140149515836,-3.1504380552088,83.8512704361609));
#29601=CARTESIAN_POINT('Ctrl Pts',(-5.90896925641487,-3.3024558822472,83.8593714204564));
#29602=CARTESIAN_POINT('Ctrl Pts',(-5.82086826400484,-3.45105515068961,
83.8674724047519));
#29603=CARTESIAN_POINT('Ctrl Pts',(-5.73274732437067,-3.59968806396205,
83.8755752232169));
#29604=CARTESIAN_POINT('Ctrl Pts',(-5.63895526377698,-3.7449005609918,83.8836780416819));
#29605=CARTESIAN_POINT('Ctrl Pts',(-5.53980417666195,-3.88623965862102,
83.8917808601469));
#29606=CARTESIAN_POINT('Ctrl Pts',(-5.44055444879911,-4.02771936786319,
83.8998917397244));
#29607=CARTESIAN_POINT('Ctrl Pts',(-5.33593525564391,-4.16531767772288,
83.908002619302));
#29608=CARTESIAN_POINT('Ctrl Pts',(-5.22630043182655,-4.29861289211876,
83.9161134988795));
#29609=CARTESIAN_POINT('Ctrl Pts',(-5.11661090070204,-4.43197462025528,
83.9242284257512));
#29610=CARTESIAN_POINT('Ctrl Pts',(-5.00190099635135,-4.56102869939972,
83.9323433526228));
#29611=CARTESIAN_POINT('Ctrl Pts',(-4.88256219763481,-4.68538956611161,
83.9404582794945));
#29612=CARTESIAN_POINT('Ctrl Pts',(-4.76304615833491,-4.80993513212333,
83.9485852585603));
#29613=CARTESIAN_POINT('Ctrl Pts',(-4.63888775218856,-4.92977330168086,
83.9567122376262));
#29614=CARTESIAN_POINT('Ctrl Pts',(-4.51051328349653,-5.0445573561415,83.964839216692));
#29615=CARTESIAN_POINT('Ctrl Pts',(-4.38288106340056,-5.15867774044919,
83.9729192063614));
#29616=CARTESIAN_POINT('Ctrl Pts',(-4.25108173245525,-5.26780214352434,
83.9809991960309));
#29617=CARTESIAN_POINT('Ctrl Pts',(-4.11556217166761,-5.37163262064138,
83.9890791857002));
#29618=CARTESIAN_POINT('Ctrl Pts',(-3.9776130062326,-5.47732457818439,83.9973040340184));
#29619=CARTESIAN_POINT('Ctrl Pts',(-3.83539619312975,-5.57784743904191,
84.0055288823365));
#29620=CARTESIAN_POINT('Ctrl Pts',(-3.68933537476457,-5.67283822195828,
84.0137537306546));
#29621=CARTESIAN_POINT('Ctrl Pts',(-3.54343905326622,-5.76772202419124,
84.0219693159699));
#29622=CARTESIAN_POINT('Ctrl Pts',(-3.39370764507189,-5.85708596087453,
84.0301849012852));
#29623=CARTESIAN_POINT('Ctrl Pts',(-3.24059755518394,-5.94060741720373,
84.0384004866005));
#29624=CARTESIAN_POINT('Ctrl Pts',(-3.08762913833998,-6.02405159097783,
84.0466084700197));
#29625=CARTESIAN_POINT('Ctrl Pts',(-2.93128857886769,-6.10166387994605,
84.054816453439));
#29626=CARTESIAN_POINT('Ctrl Pts',(-2.77206100954629,-6.17316505200964,
84.0630244368582));
#29627=CARTESIAN_POINT('Ctrl Pts',(-2.61294879211668,-6.244614425283,84.0712264740308));
#29628=CARTESIAN_POINT('Ctrl Pts',(-2.45095405664261,-6.30996135338351,
84.0794285112033));
#29629=CARTESIAN_POINT('Ctrl Pts',(-2.28658635047751,-6.36897259075669,
84.0876305483758));
#29630=CARTESIAN_POINT('Ctrl Pts',(-2.12230471346516,-6.42795292761223,
84.0958282906512));
#29631=CARTESIAN_POINT('Ctrl Pts',(-1.95565291804444,-6.48060406200328,
84.1040260329266));
#29632=CARTESIAN_POINT('Ctrl Pts',(-1.78716037693843,-6.52674090087092,
84.112223775202));
#29633=CARTESIAN_POINT('Ctrl Pts',(-1.61869987190167,-6.57286896758191,
84.1204199588123));
#29634=CARTESIAN_POINT('Ctrl Pts',(-1.44839966234766,-6.6124851052086,84.1286161424226));
#29635=CARTESIAN_POINT('Ctrl Pts',(-1.27680450356384,-6.64545402961145,
84.136812326033));
#29636=CARTESIAN_POINT('Ctrl Pts',(-1.10522197657826,-6.67842052704141,
84.1450079062898));
#29637=CARTESIAN_POINT('Ctrl Pts',(-0.932345042418501,-6.70474071717392,
84.1532034865466));
#29638=CARTESIAN_POINT('Ctrl Pts',(-0.758728781423026,-6.7243304228927,
84.1613990668035));
#29639=CARTESIAN_POINT('Ctrl Pts',(-0.585093713582004,-6.74392225065102,
84.1695955348401));
#29640=CARTESIAN_POINT('Ctrl Pts',(-0.410719515987915,-6.756782101216,84.1777920028767));
#29641=CARTESIAN_POINT('Ctrl Pts',(-0.236166577896974,-6.76287766764152,
84.1859884709134));
#29642=CARTESIAN_POINT('Ctrl Pts',(-0.0615629735190617,-6.7689750033854,
84.1941873180827));
#29643=CARTESIAN_POINT('Ctrl Pts',(0.113219116175861,-6.76830413158267,
84.202386165252));
#29644=CARTESIAN_POINT('Ctrl Pts',(0.287619060212619,-6.76088487375746,
84.2105850124214));
#29645=CARTESIAN_POINT('Ctrl Pts',(0.462201269150256,-6.75345786208634,
84.2187924281833));
#29646=CARTESIAN_POINT('Ctrl Pts',(0.636400175535817,-6.73926838925261,
84.2269998439452));
#29647=CARTESIAN_POINT('Ctrl Pts',(0.809659020699853,-6.71838829409252,
84.2352072597071));
#29648=CARTESIAN_POINT('Ctrl Pts',(0.983010726510958,-6.69749700793582,
84.2434190743552));
#29649=CARTESIAN_POINT('Ctrl Pts',(1.15542101269726,-6.66990800744151,84.2516308890033));
#29650=CARTESIAN_POINT('Ctrl Pts',(1.3263431798735,-6.63574432669034,84.2598427036514));
#29651=CARTESIAN_POINT('Ctrl Pts',(1.49751705592626,-6.60153033472536,84.268066611445));
#29652=CARTESIAN_POINT('Ctrl Pts',(1.66719808446835,-6.56072239677405,84.2762905192386));
#29653=CARTESIAN_POINT('Ctrl Pts',(1.83485334187446,-6.51349385612761,84.2845144270322));
#29654=CARTESIAN_POINT('Ctrl Pts',(1.98976370446868,-6.46985555650297,84.2921131660038));
#29655=CARTESIAN_POINT('Ctrl Pts',(2.14294455581183,-6.42073633812895,84.2997119049754));
#29656=CARTESIAN_POINT('Ctrl Pts',(2.29399148015313,-6.36630914180146,84.307310643947));
#29657=CARTESIAN_POINT('Ctrl Pts',(2.4560158360759,-6.307926414261,84.3154616261208));
#29658=CARTESIAN_POINT('Ctrl Pts',(2.61606447431989,-6.24326258603041,84.3236126082945));
#29659=CARTESIAN_POINT('Ctrl Pts',(2.77360937151675,-6.17246952639173,84.3317635904682));
#29660=CARTESIAN_POINT('Ctrl Pts',(2.93097126571379,-6.10175869945311,84.3399051045207));
#29661=CARTESIAN_POINT('Ctrl Pts',(3.085834877959,-6.02493296170729,84.3480466185731));
#29662=CARTESIAN_POINT('Ctrl Pts',(3.23768780522581,-5.94219375953798,84.3561881326256));
#29663=CARTESIAN_POINT('Ctrl Pts',(3.38939629666913,-5.85953325525758,84.3643219028281));
#29664=CARTESIAN_POINT('Ctrl Pts',(3.53809948528631,-5.7709706581231,84.3724556730306));
#29665=CARTESIAN_POINT('Ctrl Pts',(3.6833054159758,-5.67675525389666,84.3805894432331));
#29666=CARTESIAN_POINT('Ctrl Pts',(3.82840377296752,-5.58260964777952,84.3887171876505));
#29667=CARTESIAN_POINT('Ctrl Pts',(3.97000972541076,-5.48281977134684,84.3968449320678));
#29668=CARTESIAN_POINT('Ctrl Pts',(4.10765639577838,-5.37768053478644,84.4049726764852));
#29669=CARTESIAN_POINT('Ctrl Pts',(4.24523003179267,-5.27259708436407,84.4130961083786));
#29670=CARTESIAN_POINT('Ctrl Pts',(4.37884827947522,-5.16217014790846,84.4212195402721));
#29671=CARTESIAN_POINT('Ctrl Pts',(4.50807372315223,-5.04673759042655,84.4293429721656));
#29672=CARTESIAN_POINT('Ctrl Pts',(4.63811892223137,-4.93057277418906,84.4375179359167));
#29673=CARTESIAN_POINT('Ctrl Pts',(4.76371508083713,-4.80933881944455,84.4456928996679));
#29674=CARTESIAN_POINT('Ctrl Pts',(4.88445032991293,-4.68342118270538,84.4538678634191));
#29675=CARTESIAN_POINT('Ctrl Pts',(5.00439729499601,-4.55832566592044,84.4619894525915));
#29676=CARTESIAN_POINT('Ctrl Pts',(5.11954639866066,-4.42860773038687,84.4701110417639));
#29677=CARTESIAN_POINT('Ctrl Pts',(5.22953113968924,-4.29468195085743,84.4782326309363));
#29678=CARTESIAN_POINT('Ctrl Pts',(5.3395304009595,-4.16073849037818,84.486355292325));
#29679=CARTESIAN_POINT('Ctrl Pts',(5.44436370926848,-4.02258636226382,84.4944779537137));
#29680=CARTESIAN_POINT('Ctrl Pts',(5.54370529895975,-3.8806726940423,84.5026006151025));
#29681=CARTESIAN_POINT('Ctrl Pts',(5.64307892135534,-3.73871326574602,84.5107258956441));
#29682=CARTESIAN_POINT('Ctrl Pts',(5.73695708914281,-3.59299018173878,84.5188511761856));
#29683=CARTESIAN_POINT('Ctrl Pts',(5.82505778500283,-3.44397891999616,84.5269764567273));
#29684=CARTESIAN_POINT('Ctrl Pts',(5.91411831968266,-3.29334421144404,84.5351902605161));
#29685=CARTESIAN_POINT('Ctrl Pts',(5.99727456068421,-3.13934958800305,84.5434040643051));
#29686=CARTESIAN_POINT('Ctrl Pts',(6.07428365112252,-2.98251020546547,84.5516178680939));
#29687=CARTESIAN_POINT('Ctrl Pts',(6.1505946091245,-2.82709266364331,84.5597572089484));
#29688=CARTESIAN_POINT('Ctrl Pts',(6.22086932399302,-2.66888208901893,84.5678965498029));
#29689=CARTESIAN_POINT('Ctrl Pts',(6.28492075025478,-2.50839792756589,84.5760358906574));
#29690=CARTESIAN_POINT('Ctrl Pts',(6.34985114028735,-2.34571147692215,84.5842869259135));
#29691=CARTESIAN_POINT('Ctrl Pts',(6.40838607023891,-2.18068895703612,84.5925379611696));
#29692=CARTESIAN_POINT('Ctrl Pts',(6.46038363836647,-2.0138848639202,84.6007889964257));
#29693=CARTESIAN_POINT('Ctrl Pts',(6.51238120649402,-1.84708077080427,84.6090400316818));
#29694=CARTESIAN_POINT('Ctrl Pts',(6.55784137760392,-1.67849549255858,84.6172910669379));
#29695=CARTESIAN_POINT('Ctrl Pts',(6.59667642144928,-1.50869121780939,84.625542102194));
#29696=CARTESIAN_POINT('Ctrl Pts',(6.63542079932329,-1.33928337545691,84.6337738742267));
#29697=CARTESIAN_POINT('Ctrl Pts',(6.66769207561833,-1.16813340032523,84.6420056462593));
#29698=CARTESIAN_POINT('Ctrl Pts',(6.69333379840906,-0.995776914311138,
84.650237418292));
#29699=CARTESIAN_POINT('Ctrl Pts',(6.71894490242042,-0.823626239164798,
84.6584593607663));
#29700=CARTESIAN_POINT('Ctrl Pts',(6.73794216399962,-0.650272272811426,
84.6666813032406));
#29701=CARTESIAN_POINT('Ctrl Pts',(6.75021937948532,-0.476263927692286,
84.6749032457149));
#29702=CARTESIAN_POINT('Ctrl Pts',(6.76248439459687,-0.302428501824886,
84.6831170177067));
#29703=CARTESIAN_POINT('Ctrl Pts',(6.76804263775274,-0.127940347185809,
84.6913307896984));
#29704=CARTESIAN_POINT('Ctrl Pts',(6.76683924795597,0.0466432451993053,
84.6995445616902));
#29705=CARTESIAN_POINT('Ctrl Pts',(6.765636812995,0.221088313337655,84.7077518164225));
#29706=CARTESIAN_POINT('Ctrl Pts',(6.75768343356095,0.395628311704875,84.7159590711548));
#29707=CARTESIAN_POINT('Ctrl Pts',(6.74297619637966,0.569702567185123,84.724166325887));
#29708=CARTESIAN_POINT('Ctrl Pts',(6.72827768384473,0.743673558109239,84.7323687119009));
#29709=CARTESIAN_POINT('Ctrl Pts',(6.70683332513476,0.917179000461351,84.7405710979149));
#29710=CARTESIAN_POINT('Ctrl Pts',(6.67869226460581,1.08965987110408,84.7487734839288));
#29711=CARTESIAN_POINT('Ctrl Pts',(6.65055960350104,1.26208926038941,84.7569734217294));
#29712=CARTESIAN_POINT('Ctrl Pts',(6.61573427590793,1.43349433330917,84.76517335953));
#29713=CARTESIAN_POINT('Ctrl Pts',(6.57431712866856,1.60332257880166,84.7733732973307));
#29714=CARTESIAN_POINT('Ctrl Pts',(6.5329057726154,1.77312707792195,84.7815720885683));
#29715=CARTESIAN_POINT('Ctrl Pts',(6.48490451671685,1.94135484044307,84.7897708798059));
#29716=CARTESIAN_POINT('Ctrl Pts',(6.4304650454848,2.10746489859218,84.7979696710436));
#29717=CARTESIAN_POINT('Ctrl Pts',(6.37602331069314,2.27358186349499,84.8061688031819));
#29718=CARTESIAN_POINT('Ctrl Pts',(6.31514293880859,2.43758060795791,84.8143679353203));
#29719=CARTESIAN_POINT('Ctrl Pts',(6.24802509593879,2.59893659032287,84.8225670674586));
#29720=CARTESIAN_POINT('Ctrl Pts',(6.18089228687033,2.76032855247479,84.8307680278715));
#29721=CARTESIAN_POINT('Ctrl Pts',(6.10751937426341,2.91907624795365,84.8389689882843));
#29722=CARTESIAN_POINT('Ctrl Pts',(6.02815516936708,3.07467628442947,84.8471699486972));
#29723=CARTESIAN_POINT('Ctrl Pts',(5.94871658110543,3.23042215559701,84.8553785953841));
#29724=CARTESIAN_POINT('Ctrl Pts',(5.86327564463281,3.38301415390006,84.8635872420711));
#29725=CARTESIAN_POINT('Ctrl Pts',(5.77212699995609,3.53197379610579,84.871795888758));
#29726=CARTESIAN_POINT('Ctrl Pts',(5.68093483835623,3.68100455582867,84.8800084544835));
#29727=CARTESIAN_POINT('Ctrl Pts',(5.58402973400538,3.82639920367978,84.8882210202089));
#29728=CARTESIAN_POINT('Ctrl Pts',(5.48174891426729,3.96770939471749,84.8964335859344));
#29729=CARTESIAN_POINT('Ctrl Pts',(5.37932775048582,4.10921348372778,84.904657420485));
#29730=CARTESIAN_POINT('Ctrl Pts',(5.27151635082524,4.24662163302956,84.9128812550357));
#29731=CARTESIAN_POINT('Ctrl Pts',(5.15869216372487,4.37951871327475,84.9211050895863));
#29732=CARTESIAN_POINT('Ctrl Pts',(5.05502795934412,4.50162613050687,84.9286612465378));
#29733=CARTESIAN_POINT('Ctrl Pts',(4.94713247315765,4.61992548729601,84.9362174034893));
#29734=CARTESIAN_POINT('Ctrl Pts',(4.8353245216795,4.73412354824469,84.9437735604408));
#29735=CARTESIAN_POINT('Ctrl Pts',(4.70742503518454,4.86475713164338,84.9524172085999));
#29736=CARTESIAN_POINT('Ctrl Pts',(4.57411421330692,4.99032140237557,84.961060856759));
#29737=CARTESIAN_POINT('Ctrl Pts',(4.43581024301684,5.11036950600902,84.9697045049181));
#29738=CARTESIAN_POINT('Ctrl Pts',(4.29766488250379,5.2302799360608,84.9783382403676));
#29739=CARTESIAN_POINT('Ctrl Pts',(4.15453801777997,5.34468661122237,84.986971975817));
#29740=CARTESIAN_POINT('Ctrl Pts',(4.00688479438301,5.45317918690944,84.9956057112664));
#29741=CARTESIAN_POINT('Ctrl Pts',(3.85946199251083,5.56150245356185,85.0042259732647));
#29742=CARTESIAN_POINT('Ctrl Pts',(3.7075271693073,5.66392985430469,85.012846235263));
#29743=CARTESIAN_POINT('Ctrl Pts',(3.5515684951563,5.76009116457485,85.0214664972613));
#29744=CARTESIAN_POINT('Ctrl Pts',(3.4042165055845,5.8509457481065,85.0296110442896));
#29745=CARTESIAN_POINT('Ctrl Pts',(3.25327297297308,5.93620691929752,85.0377555913178));
#29746=CARTESIAN_POINT('Ctrl Pts',(3.09917575053258,6.01559628526639,85.045900138346));
#29747=CARTESIAN_POINT('Ctrl Pts',(3.09917575053248,6.01559628526645,83.0458432482751));
#29748=CARTESIAN_POINT('Ctrl Pts',(2.94443066306348,6.09531942489478,83.0540637081377));
#29749=CARTESIAN_POINT('Ctrl Pts',(2.78641930583546,6.16916464564878,83.0622841680003));
#29750=CARTESIAN_POINT('Ctrl Pts',(2.62562779814772,6.23685559120892,83.0705046278629));
#29751=CARTESIAN_POINT('Ctrl Pts',(2.46499034721999,6.30448168105682,83.0787172115794));
#29752=CARTESIAN_POINT('Ctrl Pts',(2.30157837857246,6.36596510034565,83.0869297952959));
#29753=CARTESIAN_POINT('Ctrl Pts',(2.13590237013809,6.4210754601732,83.0951423790124));
#29754=CARTESIAN_POINT('Ctrl Pts',(1.97035191792235,6.47614405506175,83.1033487388889));
#29755=CARTESIAN_POINT('Ctrl Pts',(1.80254118186197,6.52484909757285,83.1115550987655));
#29756=CARTESIAN_POINT('Ctrl Pts',(1.63300045841467,6.56700833734947,83.119761458642));
#29757=CARTESIAN_POINT('Ctrl Pts',(1.46355427379626,6.60914406840751,83.1279632425109));
#29758=CARTESIAN_POINT('Ctrl Pts',(1.29238037032785,6.6447411816277,83.1361650263798));
#29759=CARTESIAN_POINT('Ctrl Pts',(1.12002413070589,6.67366727868842,83.1443668102486));
#29760=CARTESIAN_POINT('Ctrl Pts',(0.94772949597837,6.70258303676078,83.1525656625727));
#29761=CARTESIAN_POINT('Ctrl Pts',(0.774253720049908,6.72483247038091,83.1607645148969));
#29762=CARTESIAN_POINT('Ctrl Pts',(0.600152393710189,6.74033427244702,83.168963367221));
#29763=CARTESIAN_POINT('Ctrl Pts',(0.426044884804798,6.75583662500239,83.1771625106971));
#29764=CARTESIAN_POINT('Ctrl Pts',(0.251312137196352,6.76459082661305,83.1853616541731));
#29765=CARTESIAN_POINT('Ctrl Pts',(0.0765152981278561,6.76656740224705,
83.1935607976492));
#29766=CARTESIAN_POINT('Ctrl Pts',(-0.0982951202571675,6.76854413143387,
83.2017605780863));
#29767=CARTESIAN_POINT('Ctrl Pts',(-0.273169281501512,6.7637421810302,83.2099603585233));
#29768=CARTESIAN_POINT('Ctrl Pts',(-0.447545774774762,6.75218422286309,
83.2181601389603));
#29769=CARTESIAN_POINT('Ctrl Pts',(-0.621967448440341,6.74062327006594,
83.2263620439343));
#29770=CARTESIAN_POINT('Ctrl Pts',(-0.795890839602391,6.72230284607982,
83.2345639489083));
#29771=CARTESIAN_POINT('Ctrl Pts',(-0.968759337792764,6.69729754045909,
83.2427658538822));
#29772=CARTESIAN_POINT('Ctrl Pts',(-1.14170398633059,6.67228121974463,83.2509713718795));
#29773=CARTESIAN_POINT('Ctrl Pts',(-1.31359246179592,6.64057420256431,83.2591768898768));
#29774=CARTESIAN_POINT('Ctrl Pts',(-1.48387796937551,6.60230226299902,83.2673824078741));
#29775=CARTESIAN_POINT('Ctrl Pts',(-1.65436318438348,6.56398543887052,83.2755975491383));
#29776=CARTESIAN_POINT('Ctrl Pts',(-1.8232413270061,6.51908839371184,83.2838126904025));
#29777=CARTESIAN_POINT('Ctrl Pts',(-1.98997945991885,6.46778716015772,83.2920278316668));
#29778=CARTESIAN_POINT('Ctrl Pts',(-2.15682885394968,6.41645169428671,83.3002484547352));
#29779=CARTESIAN_POINT('Ctrl Pts',(-2.32153505488385,6.35870364082029,83.3084690778037));
#29780=CARTESIAN_POINT('Ctrl Pts',(-2.48358487767961,6.29476728365403,83.3166897008721));
#29781=CARTESIAN_POINT('Ctrl Pts',(-2.64586607277502,6.23073963911865,83.3249220612226));
#29782=CARTESIAN_POINT('Ctrl Pts',(-2.80548298759804,6.16050618757545,83.333154421573));
#29783=CARTESIAN_POINT('Ctrl Pts',(-2.96194590614325,6.08433771655398,83.3413867819234));
#29784=CARTESIAN_POINT('Ctrl Pts',(-3.03308785002088,6.04970476236241,83.3451299443512));
#29785=CARTESIAN_POINT('Ctrl Pts',(-3.10357810974098,6.01384539589727,83.3488731067789));
#29786=CARTESIAN_POINT('Ctrl Pts',(-3.173372661103,5.97678801311909,83.3526162692066));
#29787=CARTESIAN_POINT('Ctrl Pts',(-3.32540914264454,5.89606431789096,83.3607701613693));
#29788=CARTESIAN_POINT('Ctrl Pts',(-3.4746125070392,5.80940338777875,83.368924053532));
#29789=CARTESIAN_POINT('Ctrl Pts',(-3.62048080640333,5.71702787560679,83.3770779456947));
#29790=CARTESIAN_POINT('Ctrl Pts',(-3.76617110568685,5.62476508736927,83.3852218878308));
#29791=CARTESIAN_POINT('Ctrl Pts',(-3.90853413530418,5.52680179125117,83.3933658299669));
#29792=CARTESIAN_POINT('Ctrl Pts',(-4.04709016103704,5.42340762145325,83.401509772103));
#29793=CARTESIAN_POINT('Ctrl Pts',(-4.18550627298595,5.32011785902022,83.4096454904916));
#29794=CARTESIAN_POINT('Ctrl Pts',(-4.32012274346839,5.21140835769521,83.4177812088803));
#29795=CARTESIAN_POINT('Ctrl Pts',(-4.45048659910675,5.09759335678821,83.4259169272689));
#29796=CARTESIAN_POINT('Ctrl Pts',(-4.5807462354779,4.98386934518137,83.4340461415648));
#29797=CARTESIAN_POINT('Ctrl Pts',(-4.70675975210336,4.86504820021443,83.4421753558607));
#29798=CARTESIAN_POINT('Ctrl Pts',(-4.82810522284315,4.74148594400054,83.4503045701566));
#29799=CARTESIAN_POINT('Ctrl Pts',(-4.94937919844588,4.61799648902423,83.4584289948276));
#29800=CARTESIAN_POINT('Ctrl Pts',(-5.06599034981524,4.48977174597194,83.4665534194986));
#29801=CARTESIAN_POINT('Ctrl Pts',(-5.17755177970986,4.35720628022398,83.4746778441695));
#29802=CARTESIAN_POINT('Ctrl Pts',(-5.28979045899961,4.22383605711877,83.4828515893064));
#29803=CARTESIAN_POINT('Ctrl Pts',(-5.39691762335385,4.08607248377964,83.4910253344432));
#29804=CARTESIAN_POINT('Ctrl Pts',(-5.49857838956078,3.94435352039536,83.4991990795801));
#29805=CARTESIAN_POINT('Ctrl Pts',(-5.59958814987847,3.80354208390882,83.5073204824376));
#29806=CARTESIAN_POINT('Ctrl Pts',(-5.69520112075932,3.65882608189352,83.5154418852951));
#29807=CARTESIAN_POINT('Ctrl Pts',(-5.78511111085763,3.51066638047987,83.5235632881526));
#29808=CARTESIAN_POINT('Ctrl Pts',(-5.87502805232226,3.36249522413938,83.5316853189141));
#29809=CARTESIAN_POINT('Ctrl Pts',(-5.95924094480983,3.21088015091966,83.5398073496757));
#29810=CARTESIAN_POINT('Ctrl Pts',(-6.03748837610024,3.05630873905999,83.5479293804373));
#29811=CARTESIAN_POINT('Ctrl Pts',(-6.11575675718707,2.90169594258798,83.5560535857736));
#29812=CARTESIAN_POINT('Ctrl Pts',(-6.18805633157849,2.74412555780631,83.5641777911099));
#29813=CARTESIAN_POINT('Ctrl Pts',(-6.2541728822409,2.58410730408832,83.5723019964463));
#29814=CARTESIAN_POINT('Ctrl Pts',(-6.32100509892106,2.42235696324146,83.5805141406969));
#29815=CARTESIAN_POINT('Ctrl Pts',(-6.38151950865884,2.25810580514608,83.5887262849475));
#29816=CARTESIAN_POINT('Ctrl Pts',(-6.43554611128877,2.0918975236555,83.5969384291981));
#29817=CARTESIAN_POINT('Ctrl Pts',(-6.48907951049594,1.92720654085356,83.6050756056096));
#29818=CARTESIAN_POINT('Ctrl Pts',(-6.53624302383644,1.76059438769159,83.6132127820211));
#29819=CARTESIAN_POINT('Ctrl Pts',(-6.57692251569119,1.59260140103992,83.6213499584327));
#29820=CARTESIAN_POINT('Ctrl Pts',(-6.61816417802968,1.42228683429307,83.6295995866028));
#29821=CARTESIAN_POINT('Ctrl Pts',(-6.65274121710189,1.25055337442426,83.6378492147729));
#29822=CARTESIAN_POINT('Ctrl Pts',(-6.6805889866268,1.07797021840157,83.6460988429431));
#29823=CARTESIAN_POINT('Ctrl Pts',(-6.70843675615168,0.905387062379014,
83.6543484711132));
#29824=CARTESIAN_POINT('Ctrl Pts',(-6.7295552724162,0.731954599804787,83.6625980992834));
#29825=CARTESIAN_POINT('Ctrl Pts',(-6.74393464102174,0.558242382506881,
83.6708477274535));
#29826=CARTESIAN_POINT('Ctrl Pts',(-6.7592338495307,0.373417895013728,83.6796250795723));
#29827=CARTESIAN_POINT('Ctrl Pts',(-6.76693482715002,0.187976924734993,
83.6884024316911));
#29828=CARTESIAN_POINT('Ctrl Pts',(-6.76699958812785,0.00236099078895365,
83.6971797838099));
#29829=CARTESIAN_POINT('',(-6.767,4.20685398138092E-12,83.3028202161898));
#29830=CARTESIAN_POINT('Ctrl Pts',(3.09917575053247,6.01559628526645,82.6513920151221));
#29831=CARTESIAN_POINT('Ctrl Pts',(2.93382384459258,6.10078395293762,82.6601414630345));
#29832=CARTESIAN_POINT('Ctrl Pts',(2.76495772122983,6.1791501026705,82.6688909109469));
#29833=CARTESIAN_POINT('Ctrl Pts',(2.59315093316715,6.25042856433176,82.6776403588593));
#29834=CARTESIAN_POINT('Ctrl Pts',(2.42134553245614,6.32170645041453,82.6863897361194));
#29835=CARTESIAN_POINT('Ctrl Pts',(2.2465997792758,6.38589665313461,82.6951391133794));
#29836=CARTESIAN_POINT('Ctrl Pts',(2.069507186899,6.44278115439081,82.7038884906394));
#29837=CARTESIAN_POINT('Ctrl Pts',(1.89241596572847,6.49966521519728,82.712637800154));
#29838=CARTESIAN_POINT('Ctrl Pts',(1.71297821457188,6.54924360009549,82.7213871096687));
#29839=CARTESIAN_POINT('Ctrl Pts',(1.53180337335839,6.59134792173557,82.7301364191834));
#29840=CARTESIAN_POINT('Ctrl Pts',(1.35062987477776,6.63345193135306,82.7388856638595));
#29841=CARTESIAN_POINT('Ctrl Pts',(1.16771959102944,6.66808192368239,82.7476349085356));
#29842=CARTESIAN_POINT('Ctrl Pts',(0.983693746906752,6.6951202836317,82.7563841532117));
#29843=CARTESIAN_POINT('Ctrl Pts',(0.79966920541976,6.72215845218868,82.7651333359559));
#29844=CARTESIAN_POINT('Ctrl Pts',(0.614529402873345,6.7416050542458,82.7738825187001));
#29845=CARTESIAN_POINT('Ctrl Pts',(0.428903127363098,6.75339404354123,82.7826317014442));
#29846=CARTESIAN_POINT('Ctrl Pts',(0.243278104163605,6.76518295330332,82.7913808251629));
#29847=CARTESIAN_POINT('Ctrl Pts',(0.0571669005387212,6.76931433552276,
82.8001299488815));
#29848=CARTESIAN_POINT('Ctrl Pts',(-0.128798404778032,6.76577415902472,
82.8088790726001));
#29849=CARTESIAN_POINT('Ctrl Pts',(-0.314762517259342,6.76223400523439,
82.8176281401993));
#29850=CARTESIAN_POINT('Ctrl Pts',(-0.500580446819479,6.75102239665088,
82.8263772077985));
#29851=CARTESIAN_POINT('Ctrl Pts',(-0.685621118842307,6.73217741012501,
82.8351262753977));
#29852=CARTESIAN_POINT('Ctrl Pts',(-0.870660665414156,6.71333253821776,
82.8438752897835));
#29853=CARTESIAN_POINT('Ctrl Pts',(-1.0549226788545,6.68685441030618,82.8526243041692));
#29854=CARTESIAN_POINT('Ctrl Pts',(-1.23778137635213,6.65283295028184,82.861373318555));
#29855=CARTESIAN_POINT('Ctrl Pts',(-1.42999922978807,6.61707018861874,82.8705701289224));
#29856=CARTESIAN_POINT('Ctrl Pts',(-1.62066601233655,6.57297172934423,82.8797669392898));
#29857=CARTESIAN_POINT('Ctrl Pts',(-1.80906628500344,6.52070304311305,82.8889637496572));
#29858=CARTESIAN_POINT('Ctrl Pts',(-1.98831342545476,6.47097374915046,82.8977137473949));
#29859=CARTESIAN_POINT('Ctrl Pts',(-2.16550875896641,6.41384933989549,82.9064637451327));
#29860=CARTESIAN_POINT('Ctrl Pts',(-2.3400503671394,6.34952386240502,82.9152137428704));
#29861=CARTESIAN_POINT('Ctrl Pts',(-2.51458843547019,6.28519968948624,82.9239635631513));
#29862=CARTESIAN_POINT('Ctrl Pts',(-2.68647261717986,6.21367483971129,82.9327133834322));
#29863=CARTESIAN_POINT('Ctrl Pts',(-2.85511905908664,6.13519226743875,82.941463203713));
#29864=CARTESIAN_POINT('Ctrl Pts',(-3.02376230488812,6.05671118252973,82.9502128581716));
#29865=CARTESIAN_POINT('Ctrl Pts',(-3.18916767379829,5.97127275992673,82.9589625126301));
#29866=CARTESIAN_POINT('Ctrl Pts',(-3.35077334102708,5.87916720438042,82.9677121670886));
#29867=CARTESIAN_POINT('Ctrl Pts',(-3.51237616037299,5.78706327195685,82.9764616673571));
#29868=CARTESIAN_POINT('Ctrl Pts',(-3.67017916302241,5.68829258362337,82.9852111676255));
#29869=CARTESIAN_POINT('Ctrl Pts',(-3.82364636566413,5.58319061741075,82.993960667894));
#29870=CARTESIAN_POINT('Ctrl Pts',(-3.97711106778746,5.47809036367739,83.0027100256024));
#29871=CARTESIAN_POINT('Ctrl Pts',(-4.12623987481873,5.36665920043266,83.0114593833109));
#29872=CARTESIAN_POINT('Ctrl Pts',(-4.27052628213873,5.2492755951238,83.0202087410193));
#29873=CARTESIAN_POINT('Ctrl Pts',(-4.41481053024921,5.13189374643086,83.0289579677958));
#29874=CARTESIAN_POINT('Ctrl Pts',(-4.55425230136471,5.00855981477407,83.0377071945723));
#29875=CARTESIAN_POINT('Ctrl Pts',(-4.68837800630488,4.87969268192134,83.0464564213488));
#29876=CARTESIAN_POINT('Ctrl Pts',(-4.82250188228852,4.75082730631854,83.0552055288197));
#29877=CARTESIAN_POINT('Ctrl Pts',(-4.9513096305294,4.61642907903555,83.0639546362905));
#29878=CARTESIAN_POINT('Ctrl Pts',(-5.07436379033356,4.47695444731702,83.0727037437614));
#29879=CARTESIAN_POINT('Ctrl Pts',(-5.19741643562803,4.3374815322059,83.0814527435511));
#29880=CARTESIAN_POINT('Ctrl Pts',(-5.31471544462778,4.19293255254584,83.0902017433409));
#29881=CARTESIAN_POINT('Ctrl Pts',(-5.42586245275639,4.04379841779588,83.0989507431306));
#29882=CARTESIAN_POINT('Ctrl Pts',(-5.5370216001915,3.89464799484345,83.1077006984728));
#29883=CARTESIAN_POINT('Ctrl Pts',(-5.64202723081236,3.74091164443871,83.1164506538149));
#29884=CARTESIAN_POINT('Ctrl Pts',(-5.74052265232941,3.58311159163274,83.1252006091571));
#29885=CARTESIAN_POINT('Ctrl Pts',(-5.83901427066893,3.42531763191825,83.1339502266395));
#29886=CARTESIAN_POINT('Ctrl Pts',(-5.93099603115716,3.26346052695655,83.142699844122));
#29887=CARTESIAN_POINT('Ctrl Pts',(-6.01615550622732,3.09809004467119,83.1514494616044));
#29888=CARTESIAN_POINT('Ctrl Pts',(-6.10131214578787,2.93272506863855,83.1601987877555));
#29889=CARTESIAN_POINT('Ctrl Pts',(-6.17964682328743,2.76384720416906,83.1689481139066));
#29890=CARTESIAN_POINT('Ctrl Pts',(-6.25089348288566,2.59203002791589,83.1776974400577));
#29891=CARTESIAN_POINT('Ctrl Pts',(-6.32213814889342,2.42021765937,83.1864465213893));
#29892=CARTESIAN_POINT('Ctrl Pts',(-6.38629508412605,2.24546640831863,83.1951956027209));
#29893=CARTESIAN_POINT('Ctrl Pts',(-6.44314639819838,2.06836976659961,83.2039446840525));
#29894=CARTESIAN_POINT('Ctrl Pts',(-6.50000285283727,1.89125711158184,83.2126945564869));
#29895=CARTESIAN_POINT('Ctrl Pts',(-6.54955227673276,1.71179891440153,83.2214444289213));
#29896=CARTESIAN_POINT('Ctrl Pts',(-6.59162635926411,1.53060476278319,83.2301943013557));
#29897=CARTESIAN_POINT('Ctrl Pts',(-6.63369752055217,1.34942319164592,83.2389435662782));
#29898=CARTESIAN_POINT('Ctrl Pts',(-6.6682943142427,1.1665061864261,83.2476928312007));
#29899=CARTESIAN_POINT('Ctrl Pts',(-6.6952992374543,0.982474997617712,83.2564420961232));
#29900=CARTESIAN_POINT('Ctrl Pts',(-6.72230554731453,0.798434359176906,
83.2651918103029));
#29901=CARTESIAN_POINT('Ctrl Pts',(-6.7417191649671,0.613279706239515,83.2739415244826));
#29902=CARTESIAN_POINT('Ctrl Pts',(-6.7534741481728,0.427639953654568,83.2826912386623));
#29903=CARTESIAN_POINT('Ctrl Pts',(-6.76248837758741,0.28528336419891,83.2894008978381));
#29904=CARTESIAN_POINT('Ctrl Pts',(-6.76699999999991,0.142641701106605,
83.296110557014));
#29905=CARTESIAN_POINT('Ctrl Pts',(-6.767,4.20685394936554E-12,83.3028202161898));
#29906=CARTESIAN_POINT('Ctrl Pts',(-6.7669999999934,9.4528375515739E-6,
83.3030260662099));
#29907=CARTESIAN_POINT('Ctrl Pts',(-6.76700024064021,-0.172262306021359,
83.3111539611311));
#29908=CARTESIAN_POINT('Ctrl Pts',(-6.76041772040418,-0.344752167752305,
83.3192818560524));
#29909=CARTESIAN_POINT('Ctrl Pts',(-6.74722842698908,-0.516911553392345,
83.3274097509736));
#29910=CARTESIAN_POINT('Ctrl Pts',(-6.73405087020116,-0.688917741248305,
83.3355304132047));
#29911=CARTESIAN_POINT('Ctrl Pts',(-6.71427827240309,-0.86059367454886,
83.3436510754358));
#29912=CARTESIAN_POINT('Ctrl Pts',(-6.68793865670865,-1.03139009307926,
83.3517717376669));
#29913=CARTESIAN_POINT('Ctrl Pts',(-6.66161689176405,-1.20207076033316,
83.3598868964042));
#29914=CARTESIAN_POINT('Ctrl Pts',(-6.62873702647889,-1.3718727380254,83.3680020551416));
#29915=CARTESIAN_POINT('Ctrl Pts',(-6.58937896398752,-1.54025123566215,
83.3761172138789));
#29916=CARTESIAN_POINT('Ctrl Pts',(-6.55003922871389,-1.70855132726992,
83.3842285937646));
#29917=CARTESIAN_POINT('Ctrl Pts',(-6.50422738748251,-1.87542890197709,
83.3923399736502));
#29918=CARTESIAN_POINT('Ctrl Pts',(-6.45207454880868,-2.04034874877197,
83.4004513535359));
#29919=CARTESIAN_POINT('Ctrl Pts',(-6.39992661755151,-2.20525307713245,
83.4085619701664));
#29920=CARTESIAN_POINT('Ctrl Pts',(-6.34143897963039,-2.3681996918337,83.416672586797));
#29921=CARTESIAN_POINT('Ctrl Pts',(-6.27679285263599,-2.52866772927915,
83.4247832034275));
#29922=CARTESIAN_POINT('Ctrl Pts',(-6.2121466358495,-2.68913598961127,83.4328938313236));
#29923=CARTESIAN_POINT('Ctrl Pts',(-6.14134204957303,-2.84712532466732,
83.4410044592196));
#29924=CARTESIAN_POINT('Ctrl Pts',(-6.06460870400489,-3.00213428535569,
83.4491150871156));
#29925=CARTESIAN_POINT('Ctrl Pts',(-5.98786051374254,-3.15717323379719,
83.457227284079));
#29926=CARTESIAN_POINT('Ctrl Pts',(-5.90518144343929,-3.30923033050929,
83.4653394810424));
#29927=CARTESIAN_POINT('Ctrl Pts',(-5.8168473212674,-3.45782825499826,83.4734516780058));
#29928=CARTESIAN_POINT('Ctrl Pts',(-5.72847914218544,-3.60648347089429,
83.4815670025983));
#29929=CARTESIAN_POINT('Ctrl Pts',(-5.63445175782866,-3.751676543635,83.4896823271907));
#29930=CARTESIAN_POINT('Ctrl Pts',(-5.53508456923408,-3.89295874771706,
83.4977976517831));
#29931=CARTESIAN_POINT('Ctrl Pts',(-5.43560601373181,-4.03439929543753,
83.5059220717179));
#29932=CARTESIAN_POINT('Ctrl Pts',(-5.33077591489073,-4.17191992138808,
83.5140464916528));
#29933=CARTESIAN_POINT('Ctrl Pts',(-5.22095475603217,-4.30510399821713,
83.5221709115876));
#29934=CARTESIAN_POINT('Ctrl Pts',(-5.11106353898663,-4.43837303713411,
83.5303005143318));
#29935=CARTESIAN_POINT('Ctrl Pts',(-4.99617516256445,-4.56729974242824,
83.538430117076));
#29936=CARTESIAN_POINT('Ctrl Pts',(-4.87668701817062,-4.69150431384286,
83.5465597198202));
#29937=CARTESIAN_POINT('Ctrl Pts',(-4.75703022003002,-4.81588419609222,
83.5547007972422));
#29938=CARTESIAN_POINT('Ctrl Pts',(-4.63276095352074,-4.93552838194434,
83.5628418746643));
#29939=CARTESIAN_POINT('Ctrl Pts',(-4.5043103695593,-5.05009674112096,83.5709829520863));
#29940=CARTESIAN_POINT('Ctrl Pts',(-4.44518089304723,-5.10283583263801,
83.5747305227969));
#29941=CARTESIAN_POINT('Ctrl Pts',(-4.38516580405952,-5.15449993889306,
83.5784780935075));
#29942=CARTESIAN_POINT('Ctrl Pts',(-4.32430916763142,-5.20505900281052,
83.582225664218));
#29943=CARTESIAN_POINT('Ctrl Pts',(-4.19187303624,-5.31508557057706,83.5903811226225));
#29944=CARTESIAN_POINT('Ctrl Pts',(-4.05501891968798,-5.42023379748667,
83.5985365810269));
#29945=CARTESIAN_POINT('Ctrl Pts',(-3.9141437135064,-5.52012391074859,83.6066920394314));
#29946=CARTESIAN_POINT('Ctrl Pts',(-3.7734399709696,-5.61989244461155,83.6148375715708));
#29947=CARTESIAN_POINT('Ctrl Pts',(-3.62872517580127,-5.71441539486231,
83.6229831037104));
#29948=CARTESIAN_POINT('Ctrl Pts',(-3.48043123136945,-5.80335139757263,
83.6311286358498));
#29949=CARTESIAN_POINT('Ctrl Pts',(-3.33228659692088,-5.8921978549335,83.6392659666479));
#29950=CARTESIAN_POINT('Ctrl Pts',(-3.18057029859005,-5.97546837700233,
83.647403297446));
#29951=CARTESIAN_POINT('Ctrl Pts',(-3.02574532241725,-6.0528633095313,83.6555406282441));
#29952=CARTESIAN_POINT('Ctrl Pts',(-2.87104369505901,-6.13019658163946,
83.6636714760435));
#29953=CARTESIAN_POINT('Ctrl Pts',(-2.71323864664276,-6.20166342213866,
83.6718023238429));
#29954=CARTESIAN_POINT('Ctrl Pts',(-2.55282000760788,-6.26700877682144,
83.6799331716424));
#29955=CARTESIAN_POINT('Ctrl Pts',(-2.39249547513759,-6.33231579788614,
83.6880592496336));
#29956=CARTESIAN_POINT('Ctrl Pts',(-2.22956074306105,-6.39150834710923,
83.6961853276247));
#29957=CARTESIAN_POINT('Ctrl Pts',(-2.06452797813734,-6.44437842056844,
83.7043114056159));
#29958=CARTESIAN_POINT('Ctrl Pts',(-1.89891003708618,-6.49743596167905,
83.7124662971996));
#29959=CARTESIAN_POINT('Ctrl Pts',(-1.73117949273514,-6.54412594728098,
83.7206211887834));
#29960=CARTESIAN_POINT('Ctrl Pts',(-1.56187240709269,-6.58428762919441,
83.7287760803671));
#29961=CARTESIAN_POINT('Ctrl Pts',(-1.39322555997764,-6.62429269456917,
83.7368991707206));
#29962=CARTESIAN_POINT('Ctrl Pts',(-1.22301480775866,-6.65782021271982,
83.7450222610741));
#29963=CARTESIAN_POINT('Ctrl Pts',(-1.05178294598792,-6.68476189811791,
83.7531453514276));
#29964=CARTESIAN_POINT('Ctrl Pts',(-0.880537638310403,-6.71170569910002,
83.7612690796432));
#29965=CARTESIAN_POINT('Ctrl Pts',(-0.708271422746935,-6.73206258032306,
83.7693928078588));
#29966=CARTESIAN_POINT('Ctrl Pts',(-0.53553480070528,-6.74577582470938,
83.7775165360745));
#29967=CARTESIAN_POINT('Ctrl Pts',(-0.362751751659414,-6.75949275485063,
83.7856424477319));
#29968=CARTESIAN_POINT('Ctrl Pts',(-0.189498408909942,-6.76656246368741,
83.7937683593893));
#29969=CARTESIAN_POINT('Ctrl Pts',(-0.016327835848695,-6.76698030156557,
83.8018942710468));
#29970=CARTESIAN_POINT('Ctrl Pts',(0.157950181193301,-6.7674008115608,83.8100721487617));
#29971=CARTESIAN_POINT('Ctrl Pts',(0.332143990632475,-6.76108407555866,
83.8182500264766));
#29972=CARTESIAN_POINT('Ctrl Pts',(0.505693297731611,-6.74807848862395,
83.8264279041915));
#29973=CARTESIAN_POINT('Ctrl Pts',(0.678414291462611,-6.73513497454738,
83.8345667506619));
#29974=CARTESIAN_POINT('Ctrl Pts',(0.850496564956195,-6.71556642097293,
83.8427055971324));
#29975=CARTESIAN_POINT('Ctrl Pts',(1.02139668540423,-6.68947216236418,83.8508444436028));
#29976=CARTESIAN_POINT('Ctrl Pts',(1.19352617743568,-6.66319019446686,83.8590418369399));
#29977=CARTESIAN_POINT('Ctrl Pts',(1.36445607369074,-6.63028835353182,83.8672392302771));
#29978=CARTESIAN_POINT('Ctrl Pts',(1.53364567701199,-6.59091950621326,83.8754366236142));
#29979=CARTESIAN_POINT('Ctrl Pts',(1.70283528033337,-6.55155065889467,83.8836340169514));
#29980=CARTESIAN_POINT('Ctrl Pts',(1.87028424783008,-6.5057149624111,83.8918314102885));
#29981=CARTESIAN_POINT('Ctrl Pts',(2.03547175042119,-6.45361478190613,83.9000288036257));
#29982=CARTESIAN_POINT('Ctrl Pts',(2.20123993080568,-6.40133145547683,83.9082550129701));
#29983=CARTESIAN_POINT('Ctrl Pts',(2.36522410994082,-6.34258403290148,83.9164812223145));
#29984=CARTESIAN_POINT('Ctrl Pts',(2.52688374619929,-6.2775112531316,83.9247074316589));
#29985=CARTESIAN_POINT('Ctrl Pts',(2.68836176478388,-6.21251157984128,83.9329243992096));
#29986=CARTESIAN_POINT('Ctrl Pts',(2.84752011107338,-6.14120083256944,83.9411413667603));
#29987=CARTESIAN_POINT('Ctrl Pts',(3.00383250907188,-6.06376774435194,83.9493583343111));
#29988=CARTESIAN_POINT('Ctrl Pts',(3.16000066993979,-5.98640610744987,83.9575677196621));
#29989=CARTESIAN_POINT('Ctrl Pts',(3.31332779313841,-5.90293353875851,83.9657771050131));
#29990=CARTESIAN_POINT('Ctrl Pts',(3.46330665181681,-5.81358719169855,83.9739864903641));
#29991=CARTESIAN_POINT('Ctrl Pts',(3.61317720992924,-5.72430536213152,83.9821899476724));
#29992=CARTESIAN_POINT('Ctrl Pts',(3.75970401250557,-5.62915838531564,83.9903934049807));
#29993=CARTESIAN_POINT('Ctrl Pts',(3.90240348740468,-5.52842979710259,83.9985968622889));
#29994=CARTESIAN_POINT('Ctrl Pts',(4.04502854338574,-5.42775373965433,84.0067960414286));
#29995=CARTESIAN_POINT('Ctrl Pts',(4.1838299557433,-5.32150207607723,84.0149952205683));
#29996=CARTESIAN_POINT('Ctrl Pts',(4.31835218954205,-5.21000224252134,84.0231943997079));
#29997=CARTESIAN_POINT('Ctrl Pts',(4.45284907645434,-5.09852341793581,84.0313920339456));
#29998=CARTESIAN_POINT('Ctrl Pts',(4.58306811105026,-4.98179861693386,84.0395896681833));
#29999=CARTESIAN_POINT('Ctrl Pts',(4.70858574603637,-4.8601964232141,84.047787302421));
#30000=CARTESIAN_POINT('Ctrl Pts',(4.83409432102289,-4.73860300687311,84.0559843449446));
#30001=CARTESIAN_POINT('Ctrl Pts',(4.95490191401302,-4.61213314789168,84.0641813874681));
#30002=CARTESIAN_POINT('Ctrl Pts',(5.07062090631274,-4.48119321436425,84.0723784299916));
#30003=CARTESIAN_POINT('Ctrl Pts',(5.18635257762259,-4.35023893411024,84.0805763706424));
#30004=CARTESIAN_POINT('Ctrl Pts',(5.29699429988119,-4.21481387235973,84.0887743112933));
#30005=CARTESIAN_POINT('Ctrl Pts',(5.40219788516575,-4.07535851300357,84.0969722519441));
#30006=CARTESIAN_POINT('Ctrl Pts',(5.50743211796276,-3.93586252803708,84.1051725807881));
#30007=CARTESIAN_POINT('Ctrl Pts',(5.60722484225888,-3.79233419308536,84.1133729096322));
#30008=CARTESIAN_POINT('Ctrl Pts',(5.70127041924144,-3.64524410796898,84.1215732384762));
#30009=CARTESIAN_POINT('Ctrl Pts',(5.79541399415545,-3.49800075116729,84.1297821122757));
#30010=CARTESIAN_POINT('Ctrl Pts',(5.88379826381659,-3.34718853190313,84.1379909860751));
#30011=CARTESIAN_POINT('Ctrl Pts',(5.96616241037227,-3.19330472912638,84.1461998598746));
#30012=CARTESIAN_POINT('Ctrl Pts',(6.04857076085715,-3.03933833860964,84.1544131392861));
#30013=CARTESIAN_POINT('Ctrl Pts',(6.124952390527,-2.88229740050623,84.1626264186976));
#30014=CARTESIAN_POINT('Ctrl Pts',(6.19509417591534,-2.72270034185545,84.1708396981091));
#30015=CARTESIAN_POINT('Ctrl Pts',(6.26533855468863,-2.56286984742335,84.1790649907326));
#30016=CARTESIAN_POINT('Ctrl Pts',(6.3293247184793,-2.40047609452752,84.1872902833561));
#30017=CARTESIAN_POINT('Ctrl Pts',(6.38688864992689,-2.23605509177101,84.1955155759796));
#30018=CARTESIAN_POINT('Ctrl Pts',(6.43894831037641,-2.08735604778603,84.2029543649975));
#30019=CARTESIAN_POINT('Ctrl Pts',(6.4857558052422,-1.93699928768334,84.2103931540153));
#30020=CARTESIAN_POINT('Ctrl Pts',(6.52722583053317,-1.78538846115365,84.2178319430332));
#30021=CARTESIAN_POINT('Ctrl Pts',(6.5730855482026,-1.61772929886722,84.2260581440487));
#30022=CARTESIAN_POINT('Ctrl Pts',(6.61254544186901,-1.44806772476172,84.2342843450642));
#30023=CARTESIAN_POINT('Ctrl Pts',(6.64542929212861,-1.27693324935919,84.2425105460797));
#30024=CARTESIAN_POINT('Ctrl Pts',(6.67827620431295,-1.10599100747197,84.250727506692));
#30025=CARTESIAN_POINT('Ctrl Pts',(6.70456171515487,-0.933579507830849,
84.2589444673044));
#30026=CARTESIAN_POINT('Ctrl Pts',(6.72415935584308,-0.760243353951828,
84.2671614279168));
#30027=CARTESIAN_POINT('Ctrl Pts',(6.74373891611447,-0.587067116767038,
84.275370807715));
#30028=CARTESIAN_POINT('Ctrl Pts',(6.75664285418664,-0.412968278389496,
84.2835801875132));
#30029=CARTESIAN_POINT('Ctrl Pts',(6.76279572049965,-0.238501662031088,
84.2917895673114));
#30030=CARTESIAN_POINT('Ctrl Pts',(6.76894414482621,-0.0641609997087456,
84.2999930204484));
#30031=CARTESIAN_POINT('Ctrl Pts',(6.76835119268485,0.11054655477672,84.3081964735854));
#30032=CARTESIAN_POINT('Ctrl Pts',(6.76099321579686,0.285060933747276,84.3163999267224));
#30033=CARTESIAN_POINT('Ctrl Pts',(6.7536390749184,0.459484331347476,84.3245991030691));
#30034=CARTESIAN_POINT('Ctrl Pts',(6.73952695053793,0.633714396599412,84.3327982794158));
#30035=CARTESIAN_POINT('Ctrl Pts',(6.71868528349019,0.807190845718842,84.3409974557625));
#30036=CARTESIAN_POINT('Ctrl Pts',(6.69784753811664,0.980634652626396,84.3491950893104));
#30037=CARTESIAN_POINT('Ctrl Pts',(6.67028280889954,1.15332476940956,84.3573927228583));
#30038=CARTESIAN_POINT('Ctrl Pts',(6.63607145211147,1.32470550782849,84.3655903564062));
#30039=CARTESIAN_POINT('Ctrl Pts',(6.60186255938082,1.49607390262771,84.3737873995233));
#30040=CARTESIAN_POINT('Ctrl Pts',(6.5610080618249,1.66613275496902,84.3819844426404));
#30041=CARTESIAN_POINT('Ctrl Pts',(6.5136395392399,1.83433610683828,84.3901814857575));
#30042=CARTESIAN_POINT('Ctrl Pts',(6.46626581920114,2.00255791461657,84.3983794282853));
#30043=CARTESIAN_POINT('Ctrl Pts',(6.41237674740521,2.16892347098477,84.406577370813));
#30044=CARTESIAN_POINT('Ctrl Pts',(6.35215394081282,2.3329014793206,84.4147753133407));
#30045=CARTESIAN_POINT('Ctrl Pts',(6.29191358091049,2.4969272827853,84.4229756453457));
#30046=CARTESIAN_POINT('Ctrl Pts',(6.22533593260335,2.65856381545149,84.4311759773506));
#30047=CARTESIAN_POINT('Ctrl Pts',(6.15265097727443,2.81729923008614,84.4393763093556));
#30048=CARTESIAN_POINT('Ctrl Pts',(6.07989026457699,2.97620008992537,84.4475851883229));
#30049=CARTESIAN_POINT('Ctrl Pts',(6.00100967714827,3.13219346419249,84.4557940672902));
#30050=CARTESIAN_POINT('Ctrl Pts',(5.91628590282751,3.28479072636363,84.4640029462574));
#30051=CARTESIAN_POINT('Ctrl Pts',(5.83151664681926,3.43746990628509,84.4722162319414));
#30052=CARTESIAN_POINT('Ctrl Pts',(5.74089813662695,3.58674903336307,84.4804295176253));
#30053=CARTESIAN_POINT('Ctrl Pts',(5.6447506740265,3.73216811358724,84.4886428033093));
#30054=CARTESIAN_POINT('Ctrl Pts',(5.54846255953812,3.87779992400336,84.4968681040179));
#30055=CARTESIAN_POINT('Ctrl Pts',(5.44662953819703,4.01956011156837,84.5050934047265));
#30056=CARTESIAN_POINT('Ctrl Pts',(5.3396132927531,4.15702043341796,84.5133187054352));
#30057=CARTESIAN_POINT('Ctrl Pts',(5.2428300073079,4.28133671373381,84.5207574977704));
#30058=CARTESIAN_POINT('Ctrl Pts',(5.1418079929839,4.40213642242927,84.5281962901057));
#30059=CARTESIAN_POINT('Ctrl Pts',(5.03684032101293,4.51912918388249,84.5356350824409));
#30060=CARTESIAN_POINT('Ctrl Pts',(4.92177755845788,4.64737352882208,84.5437892882083));
#30061=CARTESIAN_POINT('Ctrl Pts',(4.80163369204816,4.77142116902336,84.5519434939756));
#30062=CARTESIAN_POINT('Ctrl Pts',(4.67674849922026,4.89083964928733,84.5600976997429));
#30063=CARTESIAN_POINT('Ctrl Pts',(4.55204628327325,5.01008316228302,84.5682399582881));
#30064=CARTESIAN_POINT('Ctrl Pts',(4.42261684266922,5.12471077770117,84.5763822168333));
#30065=CARTESIAN_POINT('Ctrl Pts',(4.28883968130011,5.23432356547678,84.5845244753785));
#30066=CARTESIAN_POINT('Ctrl Pts',(4.1551752339486,5.34384399894047,84.5926598736595));
#30067=CARTESIAN_POINT('Ctrl Pts',(4.01717063548316,5.44835778210296,84.6007952719405));
#30068=CARTESIAN_POINT('Ctrl Pts',(3.87524213227022,5.5475028090374,84.6089306702215));
#30069=CARTESIAN_POINT('Ctrl Pts',(3.73342452133133,5.64657037149324,84.6170597121132));
#30070=CARTESIAN_POINT('Ctrl Pts',(3.58768941014001,5.74027732374158,84.6251887540049));
#30071=CARTESIAN_POINT('Ctrl Pts',(3.43848581699641,5.82830200712991,84.6333177958966));
#30072=CARTESIAN_POINT('Ctrl Pts',(3.32724415243864,5.89393053588032,84.639378562479));
#30073=CARTESIAN_POINT('Ctrl Pts',(3.21407517135522,5.95640123927637,84.6454393290614));
#30074=CARTESIAN_POINT('Ctrl Pts',(3.0991757505325,6.01559628526643,84.6515000956437));
#30075=CARTESIAN_POINT('Origin',(0.,0.,-3.69717978381041));
#30076=CARTESIAN_POINT('',(3.09917575053243,6.01559628526647,87.0457515827423));
#30077=CARTESIAN_POINT('',(3.09917575053262,6.01559628526637,86.651392015122));
#30078=CARTESIAN_POINT('',(3.09917575053259,6.01559628526639,-3.69717978381041));
#30079=CARTESIAN_POINT('',(-6.76699862563876,0.0030496394260042,85.6971797838099));
#30080=CARTESIAN_POINT('Ctrl Pts',(-6.767,4.52674774247449E-12,85.6971797838099));
#30081=CARTESIAN_POINT('Ctrl Pts',(-6.76700000000013,-0.186007249411268,
85.7059292956159));
#30082=CARTESIAN_POINT('Ctrl Pts',(-6.75932637295462,-0.372014355523239,
85.7146788074218));
#30083=CARTESIAN_POINT('Ctrl Pts',(-6.74400518266962,-0.557389537150879,
85.7234283192278));
#30084=CARTESIAN_POINT('Ctrl Pts',(-6.72868405709692,-0.742763935807108,
85.7321777940783));
#30085=CARTESIAN_POINT('Ctrl Pts',(-6.70571545653052,-0.927506129690636,
85.7409272689289));
#30086=CARTESIAN_POINT('Ctrl Pts',(-6.67517739415725,-1.11098863924525,
85.7496767437794));
#30087=CARTESIAN_POINT('Ctrl Pts',(-6.64463945823152,-1.2944703890624,85.7584261824014));
#30088=CARTESIAN_POINT('Ctrl Pts',(-6.60653217027211,-1.47669218227978,
85.7671756210234));
#30089=CARTESIAN_POINT('Ctrl Pts',(-6.56098496116766,-1.65703510503907,
85.7759250596454));
#30090=CARTESIAN_POINT('Ctrl Pts',(-6.51543793687577,-1.83737729603809,
85.7846744627656));
#30091=CARTESIAN_POINT('Ctrl Pts',(-6.46245112202704,-2.01584035396844,
85.7934238658858));
#30092=CARTESIAN_POINT('Ctrl Pts',(-6.40220448416313,-2.19181813637937,
85.8021732690061));
#30093=CARTESIAN_POINT('Ctrl Pts',(-6.34195808575257,-2.36779521935759,
85.8109226373514));
#30094=CARTESIAN_POINT('Ctrl Pts',(-6.27445201489302,-2.54128677544663,
85.8196720056966));
#30095=CARTESIAN_POINT('Ctrl Pts',(-6.19991555136247,-2.71170355237696,
85.8284213740419));
#30096=CARTESIAN_POINT('Ctrl Pts',(-6.12537937789111,-2.88211966612917,
85.837170708339));
#30097=CARTESIAN_POINT('Ctrl Pts',(-6.043812981337,-3.0494607621028,85.845920042636));
#30098=CARTESIAN_POINT('Ctrl Pts',(-5.95549339426401,-3.2131584820668,85.8546693769331));
#30099=CARTESIAN_POINT('Ctrl Pts',(-5.8671741435526,-3.37685557859464,85.8634186779086));
#30100=CARTESIAN_POINT('Ctrl Pts',(-5.77210188986342,-3.53690907467143,
85.8721679788842));
#30101=CARTESIAN_POINT('Ctrl Pts',(-5.67059953467176,-3.6927753678474,85.8809172798598));
#30102=CARTESIAN_POINT('Ctrl Pts',(-5.56909755761879,-3.84864108035629,
85.8896665482405));
#30103=CARTESIAN_POINT('Ctrl Pts',(-5.46116568338188,-4.00031938104117,
85.8984158166213));
#30104=CARTESIAN_POINT('Ctrl Pts',(-5.34717048686239,-4.14729511663058,
85.907165085002));
#30105=CARTESIAN_POINT('Ctrl Pts',(-5.23317570555648,-4.29427031687881,
85.9159143215146));
#30106=CARTESIAN_POINT('Ctrl Pts',(-5.11311782178942,-4.43654275986971,
85.9246635580273));
#30107=CARTESIAN_POINT('Ctrl Pts',(-4.98740459172158,-4.57362924147493,
85.9334127945399));
#30108=CARTESIAN_POINT('Ctrl Pts',(-4.86169180910993,-4.71071523514267,
85.942161999911));
#30109=CARTESIAN_POINT('Ctrl Pts',(-4.73032391415615,-4.84261509316343,
85.9509112052821));
#30110=CARTESIAN_POINT('Ctrl Pts',(-4.59374707237499,-4.96888084331333,
85.9596604106532));
#30111=CARTESIAN_POINT('Ctrl Pts',(-4.45717070537613,-5.0951461545254,85.9684095856095));
#30112=CARTESIAN_POINT('Ctrl Pts',(-4.31538563819724,-5.21577720253455,
85.9771587605657));
#30113=CARTESIAN_POINT('Ctrl Pts',(-4.16887341290867,-5.33036429028479,
85.9859079355219));
#30114=CARTESIAN_POINT('Ctrl Pts',(-4.02236168477565,-5.44495098921009,
85.9946570807898));
#30115=CARTESIAN_POINT('Ctrl Pts',(-3.87112305634672,-5.55349359238596,
86.0034062260577));
#30116=CARTESIAN_POINT('Ctrl Pts',(-3.71567117316973,-5.65562346102315,
86.0121553713256));
#30117=CARTESIAN_POINT('Ctrl Pts',(-3.5602198045754,-5.75775299158621,86.0209044876318));
#30118=CARTESIAN_POINT('Ctrl Pts',(-3.40055544862626,-5.85346967275215,
86.029653603938));
#30119=CARTESIAN_POINT('Ctrl Pts',(-3.2372203632364,-5.94244842803432,86.0384027202441));
#30120=CARTESIAN_POINT('Ctrl Pts',(-3.0738858049628,-6.03142689616357,86.0471518083151));
#30121=CARTESIAN_POINT('Ctrl Pts',(-2.90688079257937,-6.11366734484714,
86.055900896386));
#30122=CARTESIAN_POINT('Ctrl Pts',(-2.7367725109484,-6.18889046787202,86.064649984457));
#30123=CARTESIAN_POINT('Ctrl Pts',(-2.56666476416872,-6.26411335438177,
86.0733990450192));
#30124=CARTESIAN_POINT('Ctrl Pts',(-2.39345402972321,-6.33231884350204,
86.0821481055815));
#30125=CARTESIAN_POINT('Ctrl Pts',(-2.21772856474267,-6.39327529620964,
86.0908971661437));
#30126=CARTESIAN_POINT('Ctrl Pts',(-2.04200363768498,-6.4542315623201,86.0996461999237));
#30127=CARTESIAN_POINT('Ctrl Pts',(-1.8637642662032,-6.50793874251991,86.1083952337037));
#30128=CARTESIAN_POINT('Ctrl Pts',(-1.68361578194914,-6.55421443796065,
86.1171442674837));
#30129=CARTESIAN_POINT('Ctrl Pts',(-1.50346783420095,-6.60048999558628,
86.1258932752079));
#30130=CARTESIAN_POINT('Ctrl Pts',(-1.32141106257476,-6.6393340414545,86.1346422829321));
#30131=CARTESIAN_POINT('Ctrl Pts',(-1.13806375959275,-6.67061465526991,
86.1433912906564));
#30132=CARTESIAN_POINT('Ctrl Pts',(-0.954716987421285,-6.70189517852451,
86.1521402730513));
#30133=CARTESIAN_POINT('Ctrl Pts',(-0.770079973811828,-6.72561226535806,
86.1608892554462));
#30134=CARTESIAN_POINT('Ctrl Pts',(-0.584779770554227,-6.74168536939767,
86.1696382378411));
#30135=CARTESIAN_POINT('Ctrl Pts',(-0.391490647555678,-6.75845143942384,
86.1787644185171));
#30136=CARTESIAN_POINT('Ctrl Pts',(-0.197480213106098,-6.76689975924021,
86.1878905991932));
#30137=CARTESIAN_POINT('Ctrl Pts',(-0.00346532629955176,-6.76699911271707,
86.1970167798692));
#30138=CARTESIAN_POINT('Ctrl Pts',(0.184486595294258,-6.76709536139778,
86.2058577673991));
#30139=CARTESIAN_POINT('Ctrl Pts',(0.372442378183392,-6.7593565972678,86.2146987549291));
#30140=CARTESIAN_POINT('Ctrl Pts',(0.559750217720212,-6.74380965729032,
86.223539742459));
#30141=CARTESIAN_POINT('Ctrl Pts',(0.74512991445588,-6.72842275717274,86.2322897210568));
#30142=CARTESIAN_POINT('Ctrl Pts',(0.929874656312314,-6.70538772273499,
86.2410396996545));
#30143=CARTESIAN_POINT('Ctrl Pts',(1.11335688289591,-6.67478280180774,86.2497896782523));
#30144=CARTESIAN_POINT('Ctrl Pts',(1.2968372311867,-6.6441781941806,86.2585395672772));
#30145=CARTESIAN_POINT('Ctrl Pts',(1.47905480730049,-6.60600390230117,86.2672894563022));
#30146=CARTESIAN_POINT('Ctrl Pts',(1.65939064804622,-6.56038959797181,86.2760393453271));
#30147=CARTESIAN_POINT('Ctrl Pts',(1.83972470264086,-6.51477574543307,86.2847891476881));
#30148=CARTESIAN_POINT('Ctrl Pts',(2.01817678125675,-6.46172209820154,86.293538950049));
#30149=CARTESIAN_POINT('Ctrl Pts',(2.19414072347513,-6.40140886724072,86.30228875241));
#30150=CARTESIAN_POINT('Ctrl Pts',(2.37010298131926,-6.34109621361438,86.3110384710155));
#30151=CARTESIAN_POINT('Ctrl Pts',(2.54357687926739,-6.27352420826041,86.3197881896209));
#30152=CARTESIAN_POINT('Ctrl Pts',(2.71397317789794,-6.19892237325574,86.3285379082264));
#30153=CARTESIAN_POINT('Ctrl Pts',(2.88436790207019,-6.12432122757049,86.3372875459847));
#30154=CARTESIAN_POINT('Ctrl Pts',(3.0516848212607,-6.04269049717511,86.346037183743));
#30155=CARTESIAN_POINT('Ctrl Pts',(3.21535561997198,-5.95430745235033,86.3547868215012));
#30156=CARTESIAN_POINT('Ctrl Pts',(3.37902496075091,-5.86592519481626,86.3635363813202));
#30157=CARTESIAN_POINT('Ctrl Pts',(3.53904799384687,-5.77079087940347,86.3722859411393));
#30158=CARTESIAN_POINT('Ctrl Pts',(3.69488118814798,-5.66922763747145,86.3810355009583));
#30159=CARTESIAN_POINT('Ctrl Pts',(3.85071304610652,-5.56766526649177,86.3897849857457));
#30160=CARTESIAN_POINT('Ctrl Pts',(4.00235489705792,-5.45967423580842,86.3985344705331));
#30161=CARTESIAN_POINT('Ctrl Pts',(4.14929168607484,-5.34562133936461,86.4072839553206));
#30162=CARTESIAN_POINT('Ctrl Pts',(4.2962272638558,-5.23156938308675,86.4160333679839));
#30163=CARTESIAN_POINT('Ctrl Pts',(4.43845763091885,-5.1114558367736,86.4247827806471));
#30164=CARTESIAN_POINT('Ctrl Pts',(4.57549970660775,-4.98568866204383,86.4335321933104));
#30165=CARTESIAN_POINT('Ctrl Pts',(4.71254069815106,-4.85992248226345,86.4422815367568));
#30166=CARTESIAN_POINT('Ctrl Pts',(4.84439326931123,-4.72850295734197,86.4510308802031));
#30167=CARTESIAN_POINT('Ctrl Pts',(4.97060959434507,-4.59187644221889,86.4597802236494));
#30168=CARTESIAN_POINT('Ctrl Pts',(5.09682496280325,-4.45525096256881,86.4685295007857));
#30169=CARTESIAN_POINT('Ctrl Pts',(5.21740397615651,-4.31341878218553,86.477278777922));
#30170=CARTESIAN_POINT('Ctrl Pts',(5.33193710451749,-4.16686161438914,86.4860280550583));
#30171=CARTESIAN_POINT('Ctrl Pts',(5.44646940289209,-4.0203055086475,86.4947772687913));
#30172=CARTESIAN_POINT('Ctrl Pts',(5.55495572749501,-3.86902470980369,86.5035264825242));
#30173=CARTESIAN_POINT('Ctrl Pts',(5.65702762491302,-3.71353301466016,86.5122756962572));
#30174=CARTESIAN_POINT('Ctrl Pts',(5.75909881655015,-3.55804239467118,86.5210248494933));
#30175=CARTESIAN_POINT('Ctrl Pts',(5.85475551250658,-3.39834117619768,86.5297740027294));
#30176=CARTESIAN_POINT('Ctrl Pts',(5.94367283727983,-3.23497174692174,86.5385231559655));
#30177=CARTESIAN_POINT('Ctrl Pts',(6.03258957676214,-3.07160339301159,86.5472722516111));
#30178=CARTESIAN_POINT('Ctrl Pts',(6.11476689685199,-2.90456712829685,86.5560213472566));
#30179=CARTESIAN_POINT('Ctrl Pts',(6.18992570525187,-2.73443024476072,86.5647704429022));
#30180=CARTESIAN_POINT('Ctrl Pts',(6.2650840438863,-2.56429442463194,86.5735194838632));
#30181=CARTESIAN_POINT('Ctrl Pts',(6.33322384283255,-2.39105828656153,86.5822685248242));
#30182=CARTESIAN_POINT('Ctrl Pts',(6.39411368719979,-2.21531017132237,86.5910175657853));
#30183=CARTESIAN_POINT('Ctrl Pts',(6.45500317120843,-2.03956309619663,86.5997665549677));
#30184=CARTESIAN_POINT('Ctrl Pts',(6.50864269270033,-1.86130434438774,86.6085155441501));
#30185=CARTESIAN_POINT('Ctrl Pts',(6.55485008446299,-1.68113930720078,86.6172645333325));
#30186=CARTESIAN_POINT('Ctrl Pts',(6.60199664749375,-1.49731239211969,86.6261913468619));
#30187=CARTESIAN_POINT('Ctrl Pts',(6.64140563640882,-1.31150116499796,86.6351181603912));
#30188=CARTESIAN_POINT('Ctrl Pts',(6.67293772282152,-1.1243625515578,86.6440449739206));
#30189=CARTESIAN_POINT('Ctrl Pts',(6.70384494949855,-0.940932395052489,
86.6527948880761));
#30190=CARTESIAN_POINT('Ctrl Pts',(6.72718449348918,-0.756227260507799,
86.6615448022317));
#30191=CARTESIAN_POINT('Ctrl Pts',(6.74287707373924,-0.570874564542713,
86.6702947163872));
#30192=CARTESIAN_POINT('Ctrl Pts',(6.75856934538665,-0.385525513633454,
86.6790444584712));
#30193=CARTESIAN_POINT('Ctrl Pts',(6.766614930041,-0.199529212419166,86.6877942005552));
#30194=CARTESIAN_POINT('Ctrl Pts',(6.76698649908906,-0.0135174386013192,
86.6965439426391));
#30195=CARTESIAN_POINT('Ctrl Pts',(6.76735806132392,0.172490924444834,86.705293524285));
#30196=CARTESIAN_POINT('Ctrl Pts',(6.76005588896294,0.358514472900411,86.7140431059309));
#30197=CARTESIAN_POINT('Ctrl Pts',(6.74510478454593,0.543921359661166,86.7227926875768));
#30198=CARTESIAN_POINT('Ctrl Pts',(6.730153934407,0.729325093149327,86.7315421204159));
#30199=CARTESIAN_POINT('Ctrl Pts',(6.70755443556913,0.914111900255165,86.7402915532549));
#30200=CARTESIAN_POINT('Ctrl Pts',(6.67738304682339,1.09765415591413,86.7490409860939));
#30201=CARTESIAN_POINT('Ctrl Pts',(6.64721213111883,1.28119353391156,86.7577902817553));
#30202=CARTESIAN_POINT('Ctrl Pts',(6.60946960955518,1.46348811672544,86.7665395774166));
#30203=CARTESIAN_POINT('Ctrl Pts',(6.56428366991208,1.64391876348121,86.7752888730779));
#30204=CARTESIAN_POINT('Ctrl Pts',(6.51909837867743,1.82434682109625,86.7840380431888));
#30205=CARTESIAN_POINT('Ctrl Pts',(6.46646995271946,2.00291071820365,86.7927872132996));
#30206=CARTESIAN_POINT('Ctrl Pts',(6.40657713281573,2.17900400212633,86.8015363834104));
#30207=CARTESIAN_POINT('Ctrl Pts',(6.34668509279086,2.35509499309588,86.8102854395962));
#30208=CARTESIAN_POINT('Ctrl Pts',(6.27952894037554,2.52871516398052,86.819034495782));
#30209=CARTESIAN_POINT('Ctrl Pts',(6.20533675061478,2.69927486771349,86.8277835519678));
#30210=CARTESIAN_POINT('Ctrl Pts',(6.12832117907949,2.87632521635854,86.83686555325));
#30211=CARTESIAN_POINT('Ctrl Pts',(6.04372366626113,3.0500772891993,86.8459475545323));
#30212=CARTESIAN_POINT('Ctrl Pts',(5.95185378007903,3.2198952747813,86.8550295558146));
#30213=CARTESIAN_POINT('Ctrl Pts',(5.86334450817404,3.38350129286694,86.8637793361217));
#30214=CARTESIAN_POINT('Ctrl Pts',(5.76808562057286,3.54345567124912,86.8725291164288));
#30215=CARTESIAN_POINT('Ctrl Pts',(5.66640068804512,3.69921508465267,86.8812788967359));
#30216=CARTESIAN_POINT('Ctrl Pts',(5.56471941107956,3.85496889852236,86.8900283624894));
#30217=CARTESIAN_POINT('Ctrl Pts',(5.45661270815152,4.00652780919585,86.8987778282429));
#30218=CARTESIAN_POINT('Ctrl Pts',(5.34244776449158,4.15337704569173,86.9075272939964));
#30219=CARTESIAN_POINT('Ctrl Pts',(5.22828631819634,4.30022178356203,86.916276491716));
#30220=CARTESIAN_POINT('Ctrl Pts',(5.10806717844102,4.44235690972642,86.9250256894356));
#30221=CARTESIAN_POINT('Ctrl Pts',(4.98219864544745,4.57929969070617,86.9337748871552));
#30222=CARTESIAN_POINT('Ctrl Pts',(4.85633329944053,4.71623900429972,86.9425238633454));
#30223=CARTESIAN_POINT('Ctrl Pts',(4.72481904033678,4.84798602483587,86.9512728395357));
#30224=CARTESIAN_POINT('Ctrl Pts',(4.58810250737231,4.97409332259096,86.9600218157259));
#30225=CARTESIAN_POINT('Ctrl Pts',(4.4513770868568,5.10020881822102,86.9687713606621));
#30226=CARTESIAN_POINT('Ctrl Pts',(4.30944892636094,5.22068366307898,86.9775209055983));
#30227=CARTESIAN_POINT('Ctrl Pts',(4.16280009466709,5.33510865604813,86.9862704505344));
#30228=CARTESIAN_POINT('Ctrl Pts',(4.01615988348845,5.4495269227285,86.9950194811427));
#30229=CARTESIAN_POINT('Ctrl Pts',(3.86479978232295,5.55789587288581,87.003768511751));
#30230=CARTESIAN_POINT('Ctrl Pts',(3.70923383581141,5.6598474671383,87.0125175423592));
#30231=CARTESIAN_POINT('Ctrl Pts',(3.55366577799618,5.76180044505335,87.0212666917073));
#30232=CARTESIAN_POINT('Ctrl Pts',(3.39389200026922,5.85733573571011,87.0300158410553));
#30233=CARTESIAN_POINT('Ctrl Pts',(3.23045513626128,5.94612887621881,87.0387649904033));
#30234=CARTESIAN_POINT('Ctrl Pts',(3.18695122151632,5.9697639920666,87.0410938545163));
#30235=CARTESIAN_POINT('Ctrl Pts',(3.14318791262683,5.99292165435323,87.0434227186293));
#30236=CARTESIAN_POINT('Ctrl Pts',(3.09917575053243,6.01559628526647,87.0457515827423));
#30237=CARTESIAN_POINT('Ctrl Pts',(3.09917575053258,6.01559628526639,85.045900138346));
#30238=CARTESIAN_POINT('Ctrl Pts',(2.93640024297169,6.09945661795675,85.0545033613981));
#30239=CARTESIAN_POINT('Ctrl Pts',(2.7701058164934,6.17676461498262,85.0631065844503));
#30240=CARTESIAN_POINT('Ctrl Pts',(2.60083589136805,6.24723472155255,85.0717098075024));
#30241=CARTESIAN_POINT('Ctrl Pts',(2.43176061199912,6.3176237936021,85.080303137593));
#30242=CARTESIAN_POINT('Ctrl Pts',(2.25971694099547,6.3811905450431,85.0888964676836));
#30243=CARTESIAN_POINT('Ctrl Pts',(2.08527064437643,6.4376964311547,85.0974897977742));
#30244=CARTESIAN_POINT('Ctrl Pts',(2.04873372809135,6.44953131025782,85.0992896283709));
#30245=CARTESIAN_POINT('Ctrl Pts',(2.01209149180469,6.4610566140694,85.1010894589676));
#30246=CARTESIAN_POINT('Ctrl Pts',(1.97534925110199,6.47227041587191,85.1028892895643));
#30247=CARTESIAN_POINT('Ctrl Pts',(1.79988327660372,6.52582296529399,85.1114845473258));
#30248=CARTESIAN_POINT('Ctrl Pts',(1.62234168686871,6.57220438954524,85.1200798050874));
#30249=CARTESIAN_POINT('Ctrl Pts',(1.4433256820181,6.61128580350502,85.1286750628489));
#30250=CARTESIAN_POINT('Ctrl Pts',(1.26414203626826,6.65040381555213,85.137278369705));
#30251=CARTESIAN_POINT('Ctrl Pts',(1.0834815177399,6.68220810696158,85.145881676561));
#30252=CARTESIAN_POINT('Ctrl Pts',(0.901953607722654,6.7066212573483,85.1544849834171));
#30253=CARTESIAN_POINT('Ctrl Pts',(0.712899487659699,6.7320465854088,85.1634449863563));
#30254=CARTESIAN_POINT('Ctrl Pts',(0.52290489829983,6.74945479681724,85.1724049892955));
#30255=CARTESIAN_POINT('Ctrl Pts',(0.332660554966909,6.75881838453802,85.1813649922347));
#30256=CARTESIAN_POINT('Ctrl Pts',(0.149490065854732,6.76783380603551,85.189991835441));
#30257=CARTESIAN_POINT('Ctrl Pts',(-0.0339116426335964,6.76939210650464,
85.1986186786473));
#30258=CARTESIAN_POINT('Ctrl Pts',(-0.216930857746648,6.7635220117153,85.2072455218536));
#30259=CARTESIAN_POINT('Ctrl Pts',(-0.400124992964936,6.7576463065992,85.2158806101413));
#30260=CARTESIAN_POINT('Ctrl Pts',(-0.582935600874554,6.74432805375582,
85.224515698429));
#30261=CARTESIAN_POINT('Ctrl Pts',(-0.764754570328876,6.72364777833886,
85.2331507867167));
#30262=CARTESIAN_POINT('Ctrl Pts',(-0.946843577441532,6.70293678856265,
85.2417986998435));
#30263=CARTESIAN_POINT('Ctrl Pts',(-1.12793770097154,6.67484196857731,85.2504466129702));
#30264=CARTESIAN_POINT('Ctrl Pts',(-1.30743800710944,6.63949507549826,85.2590945260969));
#30265=CARTESIAN_POINT('Ctrl Pts',(-1.32757520874287,6.63552969221641,85.2600646902938));
#30266=CARTESIAN_POINT('Ctrl Pts',(-1.34769236653319,6.63147309036324,85.2610348544906));
#30267=CARTESIAN_POINT('Ctrl Pts',(-1.36778864671266,6.62732549509408,85.2620050186875));
#30268=CARTESIAN_POINT('Ctrl Pts',(-1.5381571931178,6.59216377507559,85.2702296982062));
#30269=CARTESIAN_POINT('Ctrl Pts',(-1.70739353262312,6.55038200664134,85.278454377725));
#30270=CARTESIAN_POINT('Ctrl Pts',(-1.87494565224324,6.50206642546308,85.2866790572437));
#30271=CARTESIAN_POINT('Ctrl Pts',(-2.04232165562978,6.45380162942678,85.2948950916937));
#30272=CARTESIAN_POINT('Ctrl Pts',(-2.20801662288681,6.39901679531064,85.3031111261437));
#30273=CARTESIAN_POINT('Ctrl Pts',(-2.37148799781839,6.33784929421672,85.3113271605938));
#30274=CARTESIAN_POINT('Ctrl Pts',(-2.53482028944595,6.27673383512803,85.3195362047483));
#30275=CARTESIAN_POINT('Ctrl Pts',(-2.69593242280624,6.20924664933658,85.3277452489029));
#30276=CARTESIAN_POINT('Ctrl Pts',(-2.85429620588865,6.13557512944383,85.3359542930574));
#30277=CARTESIAN_POINT('Ctrl Pts',(-3.01255696284828,6.06195153775099,85.3441579966854));
#30278=CARTESIAN_POINT('Ctrl Pts',(-3.16807260722118,5.98215177668911,85.3523617003134));
#30279=CARTESIAN_POINT('Ctrl Pts',(-3.32033408548818,5.89641166818815,85.3605654039413));
#30280=CARTESIAN_POINT('Ctrl Pts',(-3.47252699101504,5.81071017374932,85.3687654129353));
#30281=CARTESIAN_POINT('Ctrl Pts',(-3.62146833855935,5.71907383731397,85.3769654219293));
#30282=CARTESIAN_POINT('Ctrl Pts',(-3.76667280761687,5.62178485539598,85.3851654309232));
#30283=CARTESIAN_POINT('Ctrl Pts',(-3.91186566581762,5.52450365291098,85.3933647842271));
#30284=CARTESIAN_POINT('Ctrl Pts',(-4.05332193831789,5.42157089734255,85.401564137531));
#30285=CARTESIAN_POINT('Ctrl Pts',(-4.19058417650266,5.3133128328422,85.4097634908348));
#30286=CARTESIAN_POINT('Ctrl Pts',(-4.32784551977821,5.20505547415241,85.4179627906813));
#30287=CARTESIAN_POINT('Ctrl Pts',(-4.46091260103117,5.0914730968509,85.4261620905279));
#30288=CARTESIAN_POINT('Ctrl Pts',(-4.58936014499293,4.97293298361746,85.4343613903744));
#30289=CARTESIAN_POINT('Ctrl Pts',(-4.71783015315902,4.85437213889129,85.4425621241973));
#30290=CARTESIAN_POINT('Ctrl Pts',(-4.84167875093471,4.73085207391203,85.4507628580202));
#30291=CARTESIAN_POINT('Ctrl Pts',(-4.96051666765852,4.60277779062623,85.4589635918431));
#30292=CARTESIAN_POINT('Ctrl Pts',(-5.07939692655719,4.47465787423066,85.4671672476031));
#30293=CARTESIAN_POINT('Ctrl Pts',(-5.19326270426276,4.34198076971755,85.4753709033629));
#30294=CARTESIAN_POINT('Ctrl Pts',(-5.30176421555099,4.2051855134706,85.4835745591229));
#30295=CARTESIAN_POINT('Ctrl Pts',(-5.41039002229519,4.06823354946403,85.4917876126978));
#30296=CARTESIAN_POINT('Ctrl Pts',(-5.51363906262672,3.92715428986149,85.5000006662727));
#30297=CARTESIAN_POINT('Ctrl Pts',(-5.6112035853492,3.78241765591326,85.5082137198476));
#30298=CARTESIAN_POINT('Ctrl Pts',(-5.70882583918863,3.63759537805155,85.5164316332706));
#30299=CARTESIAN_POINT('Ctrl Pts',(-5.8007566819811,3.4891117162018,85.5246495466937));
#30300=CARTESIAN_POINT('Ctrl Pts',(-5.88673383057957,3.33746218074603,85.5328674601167));
#30301=CARTESIAN_POINT('Ctrl Pts',(-5.97284507452841,3.1855761231687,85.5410981907126));
#30302=CARTESIAN_POINT('Ctrl Pts',(-6.05298390287635,3.03051464266153,85.5493289213085));
#30303=CARTESIAN_POINT('Ctrl Pts',(-6.12693521146768,2.8727954877571,85.5575596519044));
#30304=CARTESIAN_POINT('Ctrl Pts',(-6.1948506440094,2.7279493068106,85.5651185935811));
#30305=CARTESIAN_POINT('Ctrl Pts',(-6.2575478694029,2.5808620072146,85.5726775352578));
#30306=CARTESIAN_POINT('Ctrl Pts',(-6.31489739915265,2.43194568980787,85.5802364769345));
#30307=CARTESIAN_POINT('Ctrl Pts',(-6.38883459767798,2.23995710033198,85.5899817525074));
#30308=CARTESIAN_POINT('Ctrl Pts',(-6.45408504329421,2.04440410320538,85.5997270280803));
#30309=CARTESIAN_POINT('Ctrl Pts',(-6.51033274202365,1.84603807873373,85.6094723036533));
#30310=CARTESIAN_POINT('Ctrl Pts',(-6.5637575996793,1.65762723063672,85.6187285038545));
#30311=CARTESIAN_POINT('Ctrl Pts',(-6.60906092362952,1.46667898193729,85.6279847040558));
#30312=CARTESIAN_POINT('Ctrl Pts',(-6.64601882907735,1.27386134392614,85.6372409042571));
#30313=CARTESIAN_POINT('Ctrl Pts',(-6.68284040545216,1.08175496510389,85.6464629604997));
#30314=CARTESIAN_POINT('Ctrl Pts',(-6.71137790879288,0.88779312340325,85.6556850167424));
#30315=CARTESIAN_POINT('Ctrl Pts',(-6.73145708710518,0.692657552085745,
85.6649070729851));
#30316=CARTESIAN_POINT('Ctrl Pts',(-6.75142263795899,0.498626247022922,
85.6740769418924));
#30317=CARTESIAN_POINT('Ctrl Pts',(-6.76302523036422,0.303434632015563,
85.6832468107997));
#30318=CARTESIAN_POINT('Ctrl Pts',(-6.76614176185295,0.107771325080025,
85.692416679707));
#30319=CARTESIAN_POINT('Ctrl Pts',(-6.76668136840097,0.0738935343331261,
85.6940043810747));
#30320=CARTESIAN_POINT('Ctrl Pts',(-6.76696669415284,0.0400016440156962,
85.6955920824423));
#30321=CARTESIAN_POINT('Ctrl Pts',(-6.76699725127752,0.00609927884748164,
85.6971797838099));
#30322=CARTESIAN_POINT('',(-6.767,4.35244939048229E-12,85.3028202161897));
#30323=CARTESIAN_POINT('Ctrl Pts',(3.0991757505325,6.01559628526643,84.6515000956437));
#30324=CARTESIAN_POINT('Ctrl Pts',(2.93966228093791,6.09777604823717,84.6599141842356));
#30325=CARTESIAN_POINT('Ctrl Pts',(2.77681272021419,6.17364026143562,84.6683282728275));
#30326=CARTESIAN_POINT('Ctrl Pts',(2.61117916232911,6.24291857885543,84.6767423614193));
#30327=CARTESIAN_POINT('Ctrl Pts',(2.4512708651572,6.30980223402163,84.6848656100904));
#30328=CARTESIAN_POINT('Ctrl Pts',(2.28876818650668,6.37054755109567,84.6929888587616));
#30329=CARTESIAN_POINT('Ctrl Pts',(2.12418928260589,6.42495983580149,84.7011121074327));
#30330=CARTESIAN_POINT('Ctrl Pts',(1.95959542423578,6.47937706468194,84.7092360942231));
#30331=CARTESIAN_POINT('Ctrl Pts',(1.79292531213377,6.52745999986657,84.7173600810136));
#30332=CARTESIAN_POINT('Ctrl Pts',(1.62471304845604,6.56906359462113,84.725484067804));
#30333=CARTESIAN_POINT('Ctrl Pts',(1.45645349744324,6.61067888485545,84.7336103383856));
#30334=CARTESIAN_POINT('Ctrl Pts',(1.2866512865693,6.64581111970828,84.7417366089673));
#30335=CARTESIAN_POINT('Ctrl Pts',(1.11585146793037,6.6743662247076,84.7498628795489));
#30336=CARTESIAN_POINT('Ctrl Pts',(0.944971136688856,6.70293479017685,84.7579929807388));
#30337=CARTESIAN_POINT('Ctrl Pts',(0.773092621512681,6.72491999178411,84.7661230819287));
#30338=CARTESIAN_POINT('Ctrl Pts',(0.600766820405878,6.74027953630259,84.7742531831185));
#30339=CARTESIAN_POINT('Ctrl Pts',(0.428235182212657,6.75565742725481,84.7823929954273));
#30340=CARTESIAN_POINT('Ctrl Pts',(0.255255555454282,6.76439382711683,84.7905328077361));
#30341=CARTESIAN_POINT('Ctrl Pts',(0.0823804065246283,6.76649853828558,
84.7986726200448));
#30342=CARTESIAN_POINT('Ctrl Pts',(-0.0906175152634459,6.76860474418279,
84.8068182131036));
#30343=CARTESIAN_POINT('Ctrl Pts',(-0.263510447505407,6.76406988825879,
84.8149638061625));
#30344=CARTESIAN_POINT('Ctrl Pts',(-0.435750638838326,6.7529556773869,84.8231093992213));
#30345=CARTESIAN_POINT('Ctrl Pts',(-0.608231588421889,6.74182593101227,
84.8312663782331));
#30346=CARTESIAN_POINT('Ctrl Pts',(-0.780057614198549,6.72409850849497,
84.839423357245));
#30347=CARTESIAN_POINT('Ctrl Pts',(-0.950689986302749,6.69988638336082,
84.8475803362569));
#30348=CARTESIAN_POINT('Ctrl Pts',(-0.991536191438923,6.69409045250774,
84.8495329647874));
#30349=CARTESIAN_POINT('Ctrl Pts',(-1.03231406068258,6.68792315174578,84.851485593318));
#30350=CARTESIAN_POINT('Ctrl Pts',(-1.07301633482434,6.68138645381332,84.8534382218486));
#30351=CARTESIAN_POINT('Ctrl Pts',(-1.24463313664217,6.65382516351021,84.8616712719821));
#30352=CARTESIAN_POINT('Ctrl Pts',(-1.41543824272571,6.61960716377652,84.8699043221155));
#30353=CARTESIAN_POINT('Ctrl Pts',(-1.58487627386707,6.57878835322533,84.878137372249));
#30354=CARTESIAN_POINT('Ctrl Pts',(-1.75411253035867,6.538018151603,84.8863606180853));
#30355=CARTESIAN_POINT('Ctrl Pts',(-1.92198460880699,6.4906628745298,84.8945838639217));
#30356=CARTESIAN_POINT('Ctrl Pts',(-2.08794366208133,6.43682998563535,84.902807109758));
#30357=CARTESIAN_POINT('Ctrl Pts',(-2.2537383006969,6.38305042866757,84.911022208873));
#30358=CARTESIAN_POINT('Ctrl Pts',(-2.41762335013413,6.32280614983077,84.919237307988));
#30359=CARTESIAN_POINT('Ctrl Pts',(-2.57906145728834,6.25625534961048,84.927452407103));
#30360=CARTESIAN_POINT('Ctrl Pts',(-2.74037192917028,6.18975716540296,84.9356610112433));
#30361=CARTESIAN_POINT('Ctrl Pts',(-2.89923898242252,6.11696252687464,84.9438696153837));
#30362=CARTESIAN_POINT('Ctrl Pts',(-3.05514161475003,6.03807905826204,84.9520782195241));
#30363=CARTESIAN_POINT('Ctrl Pts',(-3.21095217310614,5.95924217715167,84.9602819757746));
#30364=CARTESIAN_POINT('Ctrl Pts',(-3.36380147952,5.87432379091544,84.9684857320251));
#30365=CARTESIAN_POINT('Ctrl Pts',(-3.5131895866198,5.78357916246214,84.9766894882757));
#30366=CARTESIAN_POINT('Ctrl Pts',(-3.6625334935432,5.69286138305769,84.9848908172414));
#30367=CARTESIAN_POINT('Ctrl Pts',(-3.80841793334186,5.59632097767957,84.9930921462072));
#30368=CARTESIAN_POINT('Ctrl Pts',(-3.95036838552731,5.49425869600498,85.001293475173));
#30369=CARTESIAN_POINT('Ctrl Pts',(-4.09229926138989,5.39221048969365,85.0094936730973));
#30370=CARTESIAN_POINT('Ctrl Pts',(-4.23029693891469,5.28464213219884,85.0176938710215));
#30371=CARTESIAN_POINT('Ctrl Pts',(-4.36391666322163,5.17189717187577,85.0258940689457));
#30372=CARTESIAN_POINT('Ctrl Pts',(-4.49754217470596,5.05914732847808,85.0340946220271));
#30373=CARTESIAN_POINT('Ctrl Pts',(-4.62678908133326,4.94122066660374,85.0422951751084));
#30374=CARTESIAN_POINT('Ctrl Pts',(-4.75124641020018,4.81850044615126,85.0504957281898));
#30375=CARTESIAN_POINT('Ctrl Pts',(-4.87573168351915,4.69575267128035,85.0586981225445));
#30376=CARTESIAN_POINT('Ctrl Pts',(-4.99542498210598,4.56820944565328,85.0669005168992));
#30377=CARTESIAN_POINT('Ctrl Pts',(-5.1099528035355,4.43629026841568,85.0751029112539));
#30378=CARTESIAN_POINT('Ctrl Pts',(-5.22458772861137,4.30424772355674,85.0833129762893));
#30379=CARTESIAN_POINT('Ctrl Pts',(-5.33404729014861,4.16782132194593,85.0915230413246));
#30380=CARTESIAN_POINT('Ctrl Pts',(-5.43799826248202,4.02746370526695,85.09973310636));
#30381=CARTESIAN_POINT('Ctrl Pts',(-5.54199898390667,3.88703891592259,85.1079471005868));
#30382=CARTESIAN_POINT('Ctrl Pts',(-5.64048565794353,3.74267945609009,85.1161610948137));
#30383=CARTESIAN_POINT('Ctrl Pts',(-5.73316896334866,3.59486615017802,85.1243750890405));
#30384=CARTESIAN_POINT('Ctrl Pts',(-5.82597862696782,3.4468513254998,85.1326002816772));
#30385=CARTESIAN_POINT('Ctrl Pts',(-5.91296893139418,3.29537355503984,85.1408254743139));
#30386=CARTESIAN_POINT('Ctrl Pts',(-5.9938964313008,3.14093848568219,85.1490506669506));
#30387=CARTESIAN_POINT('Ctrl Pts',(-6.06667435844338,3.00205535894607,85.1564475650525));
#30388=CARTESIAN_POINT('Ctrl Pts',(-6.13454962914461,2.86078102512443,85.1638444631543));
#30389=CARTESIAN_POINT('Ctrl Pts',(-6.19737899166069,2.71749565477531,85.1712413612562));
#30390=CARTESIAN_POINT('Ctrl Pts',(-6.27351749308934,2.54385815571206,85.1802051437003));
#30391=CARTESIAN_POINT('Ctrl Pts',(-6.34240785676341,2.36689760305845,85.1891689261444));
#30392=CARTESIAN_POINT('Ctrl Pts',(-6.40377895071463,2.18721378707802,85.1981327085885));
#30393=CARTESIAN_POINT('Ctrl Pts',(-6.46499023798479,2.00799785707495,85.2070731498759));
#30394=CARTESIAN_POINT('Ctrl Pts',(-6.51872125062415,1.8260730545473,85.2160135911632));
#30395=CARTESIAN_POINT('Ctrl Pts',(-6.56474965271754,1.64205694089607,85.2249540324506));
#30396=CARTESIAN_POINT('Ctrl Pts',(-6.61070198134038,1.45834495999257,85.2338796974181));
#30397=CARTESIAN_POINT('Ctrl Pts',(-6.64897703290111,1.27254880623831,85.2428053623855));
#30398=CARTESIAN_POINT('Ctrl Pts',(-6.67940181839658,1.08530196185229,85.2517310273529));
#30399=CARTESIAN_POINT('Ctrl Pts',(-6.70974215523581,0.898574849787709,
85.2606319177689));
#30400=CARTESIAN_POINT('Ctrl Pts',(-6.732275662664,0.710405329823299,85.2695328081849));
#30401=CARTESIAN_POINT('Ctrl Pts',(-6.74688020335029,0.521436977630101,
85.2784336986009));
#30402=CARTESIAN_POINT('Ctrl Pts',(-6.76021796589159,0.348859485224565,
85.2865625377972));
#30403=CARTESIAN_POINT('Ctrl Pts',(-6.766943122425,0.175616043403798,85.2946913769935));
#30404=CARTESIAN_POINT('Ctrl Pts',(-6.76699964058907,0.00220550842528099,
85.3028202161898));
#30405=CARTESIAN_POINT('Ctrl Pts',(-6.767,4.35244894485728E-12,85.3028202161897));
#30406=CARTESIAN_POINT('Ctrl Pts',(-6.76700000000012,-0.186007249411442,
85.3115697279957));
#30407=CARTESIAN_POINT('Ctrl Pts',(-6.75932637295461,-0.37201435552342,
85.3203192398016));
#30408=CARTESIAN_POINT('Ctrl Pts',(-6.74400518266961,-0.557389537151059,
85.3290687516076));
#30409=CARTESIAN_POINT('Ctrl Pts',(-6.72868405709688,-0.742763935807543,
85.3378182264581));
#30410=CARTESIAN_POINT('Ctrl Pts',(-6.70571545653043,-0.927506129691318,
85.3465677013087));
#30411=CARTESIAN_POINT('Ctrl Pts',(-6.6751773941571,-1.11098863924618,85.3553171761592));
#30412=CARTESIAN_POINT('Ctrl Pts',(-6.64463945823134,-1.29447038906332,
85.3640666147812));
#30413=CARTESIAN_POINT('Ctrl Pts',(-6.60653217027191,-1.47669218228071,
85.3728160534032));
#30414=CARTESIAN_POINT('Ctrl Pts',(-6.56098496116743,-1.65703510503998,
85.3815654920252));
#30415=CARTESIAN_POINT('Ctrl Pts',(-6.51543793687551,-1.837377296039,85.3903148951455));
#30416=CARTESIAN_POINT('Ctrl Pts',(-6.46245112202676,-2.01584035396935,
85.3990642982657));
#30417=CARTESIAN_POINT('Ctrl Pts',(-6.40220448416282,-2.19181813638027,
85.4078137013859));
#30418=CARTESIAN_POINT('Ctrl Pts',(-6.34195808575224,-2.36779521935847,
85.4165630697312));
#30419=CARTESIAN_POINT('Ctrl Pts',(-6.27445201489266,-2.54128677544751,
85.4253124380765));
#30420=CARTESIAN_POINT('Ctrl Pts',(-6.19991555136209,-2.71170355237783,
85.4340618064218));
#30421=CARTESIAN_POINT('Ctrl Pts',(-6.1253793778906,-2.88211966613026,85.4428111407188));
#30422=CARTESIAN_POINT('Ctrl Pts',(-6.04381298133635,-3.0494607621041,85.4515604750159));
#30423=CARTESIAN_POINT('Ctrl Pts',(-5.95549339426319,-3.2131584820683,85.4603098093129));
#30424=CARTESIAN_POINT('Ctrl Pts',(-5.86717414355174,-3.37685557859613,
85.4690591102885));
#30425=CARTESIAN_POINT('Ctrl Pts',(-5.77210188986252,-3.53690907467289,
85.4778084112641));
#30426=CARTESIAN_POINT('Ctrl Pts',(-5.67059953467082,-3.69277536784884,
85.4865577122396));
#30427=CARTESIAN_POINT('Ctrl Pts',(-5.56909755761774,-3.84864108035781,
85.4953069806204));
#30428=CARTESIAN_POINT('Ctrl Pts',(-5.46116568338073,-4.00031938104276,
85.5040562490012));
#30429=CARTESIAN_POINT('Ctrl Pts',(-5.3471704868611,-4.14729511663224,85.5128055173819));
#30430=CARTESIAN_POINT('Ctrl Pts',(-5.23317570555531,-4.29427031688023,
85.5215547538945));
#30431=CARTESIAN_POINT('Ctrl Pts',(-5.11311782178838,-4.43654275987091,
85.5303039904071));
#30432=CARTESIAN_POINT('Ctrl Pts',(-4.98740459172068,-4.57362924147591,
85.5390532269197));
#30433=CARTESIAN_POINT('Ctrl Pts',(-4.86169180910883,-4.71071523514381,
85.5478024322909));
#30434=CARTESIAN_POINT('Ctrl Pts',(-4.73032391415484,-4.84261509316472,
85.556551637662));
#30435=CARTESIAN_POINT('Ctrl Pts',(-4.59374707237345,-4.96888084331476,
85.5653008430331));
#30436=CARTESIAN_POINT('Ctrl Pts',(-4.45717070537455,-5.09514615452678,
85.5740500179893));
#30437=CARTESIAN_POINT('Ctrl Pts',(-4.31538563819563,-5.21577720253588,
85.5827991929456));
#30438=CARTESIAN_POINT('Ctrl Pts',(-4.16887341290702,-5.33036429028608,
85.5915483679018));
#30439=CARTESIAN_POINT('Ctrl Pts',(-4.02236168477416,-5.44495098921118,
85.6002975131697));
#30440=CARTESIAN_POINT('Ctrl Pts',(-3.87112305634542,-5.55349359238686,
85.6090466584376));
#30441=CARTESIAN_POINT('Ctrl Pts',(-3.71567117316862,-5.65562346102388,
85.6177958037055));
#30442=CARTESIAN_POINT('Ctrl Pts',(-3.56021980457459,-5.7577529915867,85.6265449200117));
#30443=CARTESIAN_POINT('Ctrl Pts',(-3.40055544862578,-5.85346967275242,
85.6352940363178));
#30444=CARTESIAN_POINT('Ctrl Pts',(-3.23722036323625,-5.94244842803441,
85.644043152624));
#30445=CARTESIAN_POINT('Ctrl Pts',(-3.07388580496276,-6.03142689616358,
85.6527922406949));
#30446=CARTESIAN_POINT('Ctrl Pts',(-2.90688079257944,-6.1136673448471,85.6615413287658));
#30447=CARTESIAN_POINT('Ctrl Pts',(-2.73677251094859,-6.18889046787194,
85.6702904168368));
#30448=CARTESIAN_POINT('Ctrl Pts',(-2.5666647641688,-6.26411335438175,85.679039477399));
#30449=CARTESIAN_POINT('Ctrl Pts',(-2.39345402972317,-6.33231884350206,
85.6877885379612));
#30450=CARTESIAN_POINT('Ctrl Pts',(-2.21772856474251,-6.39327529620969,
85.6965375985235));
#30451=CARTESIAN_POINT('Ctrl Pts',(-2.04200363768457,-6.45423156232023,
85.7052866323035));
#30452=CARTESIAN_POINT('Ctrl Pts',(-1.86376426620255,-6.5079387425201,85.7140356660835));
#30453=CARTESIAN_POINT('Ctrl Pts',(-1.68361578194823,-6.55421443796088,
85.7227846998635));
#30454=CARTESIAN_POINT('Ctrl Pts',(-1.50346783420016,-6.60048999558646,
85.7315337075878));
#30455=CARTESIAN_POINT('Ctrl Pts',(-1.32141106257409,-6.63933404145463,
85.740282715312));
#30456=CARTESIAN_POINT('Ctrl Pts',(-1.1380637595922,-6.67061465527,85.7490317230362));
#30457=CARTESIAN_POINT('Ctrl Pts',(-0.954716987420987,-6.70189517852454,
85.7577807054311));
#30458=CARTESIAN_POINT('Ctrl Pts',(-0.770079973811785,-6.72561226535806,
85.766529687826));
#30459=CARTESIAN_POINT('Ctrl Pts',(-0.58477977055444,-6.74168536939765,
85.7752786702208));
#30460=CARTESIAN_POINT('Ctrl Pts',(-0.391490647555891,-6.75845143942382,
85.7844048508969));
#30461=CARTESIAN_POINT('Ctrl Pts',(-0.197480213106309,-6.76689975924021,
85.793531031573));
#30462=CARTESIAN_POINT('Ctrl Pts',(-0.00346532629976212,-6.76699911271707,
85.802657212249));
#30463=CARTESIAN_POINT('Ctrl Pts',(0.184486595294048,-6.76709536139779,
85.8114981997789));
#30464=CARTESIAN_POINT('Ctrl Pts',(0.372442378183182,-6.75935659726781,
85.8203391873088));
#30465=CARTESIAN_POINT('Ctrl Pts',(0.559750217720002,-6.74380965729034,
85.8291801748388));
#30466=CARTESIAN_POINT('Ctrl Pts',(0.745129914455671,-6.72842275717276,
85.8379301534365));
#30467=CARTESIAN_POINT('Ctrl Pts',(0.929874656312104,-6.70538772273502,
85.8466801320343));
#30468=CARTESIAN_POINT('Ctrl Pts',(1.1133568828957,-6.67478280180777,85.8554301106321));
#30469=CARTESIAN_POINT('Ctrl Pts',(1.29683723118637,-6.64417819418066,85.864179999657));
#30470=CARTESIAN_POINT('Ctrl Pts',(1.47905480730003,-6.60600390230127,85.872929888682));
#30471=CARTESIAN_POINT('Ctrl Pts',(1.65939064804565,-6.56038959797196,85.8816797777069));
#30472=CARTESIAN_POINT('Ctrl Pts',(1.83972470264028,-6.51477574543323,85.8904295800678));
#30473=CARTESIAN_POINT('Ctrl Pts',(2.01817678125618,-6.46172209820172,85.8991793824288));
#30474=CARTESIAN_POINT('Ctrl Pts',(2.19414072347456,-6.40140886724091,85.9079291847898));
#30475=CARTESIAN_POINT('Ctrl Pts',(2.3701029813187,-6.34109621361459,85.9166789033952));
#30476=CARTESIAN_POINT('Ctrl Pts',(2.54357687926684,-6.27352420826064,85.9254286220007));
#30477=CARTESIAN_POINT('Ctrl Pts',(2.7139731778974,-6.19892237325598,85.9341783406062));
#30478=CARTESIAN_POINT('Ctrl Pts',(2.88436790206977,-6.12432122757069,85.9429279783645));
#30479=CARTESIAN_POINT('Ctrl Pts',(3.05168482126039,-6.04269049717527,85.9516776161227));
#30480=CARTESIAN_POINT('Ctrl Pts',(3.21535561997179,-5.95430745235043,85.960427253881));
#30481=CARTESIAN_POINT('Ctrl Pts',(3.37902496075073,-5.86592519481636,85.9691768137));
#30482=CARTESIAN_POINT('Ctrl Pts',(3.53904799384669,-5.77079087940358,85.977926373519));
#30483=CARTESIAN_POINT('Ctrl Pts',(3.69488118814781,-5.66922763747157,85.986675933338));
#30484=CARTESIAN_POINT('Ctrl Pts',(3.85071304610635,-5.56766526649189,85.9954254181255));
#30485=CARTESIAN_POINT('Ctrl Pts',(4.00235489705775,-5.45967423580855,86.0041749029129));
#30486=CARTESIAN_POINT('Ctrl Pts',(4.14929168607467,-5.34562133936473,86.0129243877004));
#30487=CARTESIAN_POINT('Ctrl Pts',(4.29622726385584,-5.23156938308673,86.0216738003637));
#30488=CARTESIAN_POINT('Ctrl Pts',(4.43845763091908,-5.11145583677341,86.030423213027));
#30489=CARTESIAN_POINT('Ctrl Pts',(4.57549970660816,-4.98568866204345,86.0391726256903));
#30490=CARTESIAN_POINT('Ctrl Pts',(4.71254069815155,-4.85992248226297,86.0479219691366));
#30491=CARTESIAN_POINT('Ctrl Pts',(4.8443932693118,-4.72850295734139,86.0566713125829));
#30492=CARTESIAN_POINT('Ctrl Pts',(4.9706095943457,-4.5918764422182,86.0654206560293));
#30493=CARTESIAN_POINT('Ctrl Pts',(5.09682496280396,-4.45525096256801,86.0741699331656));
#30494=CARTESIAN_POINT('Ctrl Pts',(5.21740397615728,-4.3134187821846,86.0829192103019));
#30495=CARTESIAN_POINT('Ctrl Pts',(5.33193710451831,-4.16686161438809,86.0916684874382));
#30496=CARTESIAN_POINT('Ctrl Pts',(5.44646940289288,-4.02030550864643,86.1004177011711));
#30497=CARTESIAN_POINT('Ctrl Pts',(5.55495572749577,-3.8690247098026,86.1091669149041));
#30498=CARTESIAN_POINT('Ctrl Pts',(5.65702762491375,-3.71353301465905,86.117916128637));
#30499=CARTESIAN_POINT('Ctrl Pts',(5.75909881655071,-3.55804239467027,86.1266652818732));
#30500=CARTESIAN_POINT('Ctrl Pts',(5.85475551250698,-3.39834117619698,86.1354144351093));
#30501=CARTESIAN_POINT('Ctrl Pts',(5.9436728372801,-3.23497174692125,86.1441635883454));
#30502=CARTESIAN_POINT('Ctrl Pts',(6.03258957676226,-3.07160339301132,86.1529126839909));
#30503=CARTESIAN_POINT('Ctrl Pts',(6.114766896852,-2.90456712829681,86.1616617796364));
#30504=CARTESIAN_POINT('Ctrl Pts',(6.18992570525178,-2.73443024476092,86.170410875282));
#30505=CARTESIAN_POINT('Ctrl Pts',(6.26508404388622,-2.56429442463214,86.179159916243));
#30506=CARTESIAN_POINT('Ctrl Pts',(6.33322384283247,-2.39105828656172,86.187908957204));
#30507=CARTESIAN_POINT('Ctrl Pts',(6.39411368719972,-2.21531017132257,86.1966579981651));
#30508=CARTESIAN_POINT('Ctrl Pts',(6.45500317120833,-2.03956309619696,86.2054069873475));
#30509=CARTESIAN_POINT('Ctrl Pts',(6.5086426927002,-1.86130434438819,86.2141559765299));
#30510=CARTESIAN_POINT('Ctrl Pts',(6.55485008446285,-1.68113930720135,86.2229049657123));
#30511=CARTESIAN_POINT('Ctrl Pts',(6.60199664749362,-1.49731239212027,86.2318317792416));
#30512=CARTESIAN_POINT('Ctrl Pts',(6.64140563640871,-1.31150116499854,86.240758592771));
#30513=CARTESIAN_POINT('Ctrl Pts',(6.67293772282142,-1.12436255155839,86.2496854063004));
#30514=CARTESIAN_POINT('Ctrl Pts',(6.70384494949847,-0.940932395053078,
86.2584353204559));
#30515=CARTESIAN_POINT('Ctrl Pts',(6.72718449348912,-0.756227260508392,
86.2671852346114));
#30516=CARTESIAN_POINT('Ctrl Pts',(6.74287707373918,-0.570874564543308,
86.275935148767));
#30517=CARTESIAN_POINT('Ctrl Pts',(6.75856934538661,-0.38552551363405,86.284684890851));
#30518=CARTESIAN_POINT('Ctrl Pts',(6.76661493004099,-0.199529212419761,
86.2934346329349));
#30519=CARTESIAN_POINT('Ctrl Pts',(6.76698649908906,-0.0135174386019142,
86.3021843750189));
#30520=CARTESIAN_POINT('Ctrl Pts',(6.76735806132393,0.172490924444367,86.3109339566648));
#30521=CARTESIAN_POINT('Ctrl Pts',(6.76005588896296,0.358514472900072,86.3196835383107));
#30522=CARTESIAN_POINT('Ctrl Pts',(6.74510478454595,0.543921359660955,86.3284331199566));
#30523=CARTESIAN_POINT('Ctrl Pts',(6.73015393440701,0.729325093149245,86.3371825527957));
#30524=CARTESIAN_POINT('Ctrl Pts',(6.70755443556913,0.914111900255209,86.3459319856347));
#30525=CARTESIAN_POINT('Ctrl Pts',(6.67738304682337,1.0976541559143,86.3546814184737));
#30526=CARTESIAN_POINT('Ctrl Pts',(6.6472121311188,1.28119353391173,86.3634307141351));
#30527=CARTESIAN_POINT('Ctrl Pts',(6.60946960955515,1.46348811672561,86.3721800097964));
#30528=CARTESIAN_POINT('Ctrl Pts',(6.56428366991204,1.64391876348138,86.3809293054577));
#30529=CARTESIAN_POINT('Ctrl Pts',(6.51909837867742,1.82434682109629,86.3896784755686));
#30530=CARTESIAN_POINT('Ctrl Pts',(6.46646995271948,2.00291071820357,86.3984276456794));
#30531=CARTESIAN_POINT('Ctrl Pts',(6.4065771328158,2.17900400212613,86.4071768157902));
#30532=CARTESIAN_POINT('Ctrl Pts',(6.34668509279089,2.3550949930958,86.415925871976));
#30533=CARTESIAN_POINT('Ctrl Pts',(6.27952894037553,2.52871516398056,86.4246749281618));
#30534=CARTESIAN_POINT('Ctrl Pts',(6.20533675061471,2.69927486771364,86.4334239843476));
#30535=CARTESIAN_POINT('Ctrl Pts',(6.12832117907942,2.8763252163587,86.4425059856298));
#30536=CARTESIAN_POINT('Ctrl Pts',(6.04372366626106,3.05007728919946,86.4515879869121));
#30537=CARTESIAN_POINT('Ctrl Pts',(5.95185378007895,3.21989527478146,86.4606699881944));
#30538=CARTESIAN_POINT('Ctrl Pts',(5.86334450817396,3.38350129286709,86.4694197685015));
#30539=CARTESIAN_POINT('Ctrl Pts',(5.76808562057277,3.54345567124927,86.4781695488086));
#30540=CARTESIAN_POINT('Ctrl Pts',(5.66640068804502,3.69921508465281,86.4869193291158));
#30541=CARTESIAN_POINT('Ctrl Pts',(5.56471941107939,3.85496889852261,86.4956687948692));
#30542=CARTESIAN_POINT('Ctrl Pts',(5.45661270815127,4.00652780919619,86.5044182606227));
#30543=CARTESIAN_POINT('Ctrl Pts',(5.34244776449124,4.15337704569217,86.5131677263762));
#30544=CARTESIAN_POINT('Ctrl Pts',(5.22828631819606,4.30022178356236,86.5219169240958));
#30545=CARTESIAN_POINT('Ctrl Pts',(5.10806717844082,4.44235690972665,86.5306661218154));
#30546=CARTESIAN_POINT('Ctrl Pts',(4.98219864544733,4.5792996907063,86.539415319535));
#30547=CARTESIAN_POINT('Ctrl Pts',(4.8563332994404,4.71623900429985,86.5481642957252));
#30548=CARTESIAN_POINT('Ctrl Pts',(4.72481904033666,4.847986024836,86.5569132719155));
#30549=CARTESIAN_POINT('Ctrl Pts',(4.58810250737218,4.97409332259108,86.5656622481057));
#30550=CARTESIAN_POINT('Ctrl Pts',(4.45137708685657,5.10020881822122,86.5744117930419));
#30551=CARTESIAN_POINT('Ctrl Pts',(4.30944892636061,5.22068366307925,86.5831613379781));
#30552=CARTESIAN_POINT('Ctrl Pts',(4.16280009466665,5.33510865604847,86.5919108829142));
#30553=CARTESIAN_POINT('Ctrl Pts',(4.0161598834881,5.44952692272875,86.6006599135225));
#30554=CARTESIAN_POINT('Ctrl Pts',(3.86479978232271,5.55789587288598,86.6094089441308));
#30555=CARTESIAN_POINT('Ctrl Pts',(3.70923383581127,5.65984746713839,86.618157974739));
#30556=CARTESIAN_POINT('Ctrl Pts',(3.55366577799604,5.76180044505344,86.6269071240871));
#30557=CARTESIAN_POINT('Ctrl Pts',(3.39389200026908,5.8573357357102,86.6356562734351));
#30558=CARTESIAN_POINT('Ctrl Pts',(3.23045513626113,5.94612887621889,86.6444054227831));
#30559=CARTESIAN_POINT('Ctrl Pts',(3.18695122151628,5.96976399206662,86.6467342868961));
#30560=CARTESIAN_POINT('Ctrl Pts',(3.14318791262691,5.99292165435319,86.6490631510091));
#30561=CARTESIAN_POINT('Ctrl Pts',(3.09917575053262,6.01559628526637,86.6513920151221));
#30562=CARTESIAN_POINT('Origin',(0.,0.,-3.69717978381041));
#30563=CARTESIAN_POINT('',(3.09917575053266,6.01559628526635,89.0455129651334));
#30564=CARTESIAN_POINT('',(3.10355585847744,6.02401335114973,88.6512963024177));
#30565=CARTESIAN_POINT('',(3.09917575053259,6.01559628526639,-3.69717978381041));
#30566=CARTESIAN_POINT('',(-6.76699876913485,-0.00288604624860754,87.6971797838098));
#30567=CARTESIAN_POINT('Ctrl Pts',(-6.7669975382697,-0.00577209250227239,
87.6971797838098));
#30568=CARTESIAN_POINT('Ctrl Pts',(-6.7668219844602,-0.211585183032179,
87.7068360010219));
#30569=CARTESIAN_POINT('Ctrl Pts',(-6.75725319663902,-0.416988477787186,
87.7164922182341));
#30570=CARTESIAN_POINT('Ctrl Pts',(-6.73842610194962,-0.621210647497327,
87.7261484354462));
#30571=CARTESIAN_POINT('Ctrl Pts',(-6.7194757805851,-0.826769487542093,
87.7358678543133));
#30572=CARTESIAN_POINT('Ctrl Pts',(-6.69114566347315,-1.03113163631452,
87.7455872731803));
#30573=CARTESIAN_POINT('Ctrl Pts',(-6.65362223626317,-1.23353157118262,
87.7553066920473));
#30574=CARTESIAN_POINT('Ctrl Pts',(-6.61579460887123,-1.43757235022714,
87.7651049056622));
#30575=CARTESIAN_POINT('Ctrl Pts',(-6.56862406942557,-1.6396189176202,87.7749031192772));
#30576=CARTESIAN_POINT('Ctrl Pts',(-6.51234997735823,-1.83890912565093,
87.7847013328921));
#30577=CARTESIAN_POINT('Ctrl Pts',(-6.46802059077958,-1.99589811203143,
87.7924197834821));
#30578=CARTESIAN_POINT('Ctrl Pts',(-6.41804309218314,-2.15117711307301,
87.800138234072));
#30579=CARTESIAN_POINT('Ctrl Pts',(-6.36255499057615,-2.30438342987763,
87.807856684662));
#30580=CARTESIAN_POINT('Ctrl Pts',(-6.30393649042945,-2.46623298399817,
87.8160105768287));
#30581=CARTESIAN_POINT('Ctrl Pts',(-6.23904228599784,-2.62610950829824,
87.8241644689955));
#30582=CARTESIAN_POINT('Ctrl Pts',(-6.16802248275564,-2.78348480366266,
87.8323183611622));
#30583=CARTESIAN_POINT('Ctrl Pts',(-6.09708934351528,-2.9406680571984,87.8404623033024));
#30584=CARTESIAN_POINT('Ctrl Pts',(-6.02004563327546,-3.09535582767633,
87.8486062454426));
#30585=CARTESIAN_POINT('Ctrl Pts',(-5.93709108849273,-3.24703532579186,
87.8567501875828));
#30586=CARTESIAN_POINT('Ctrl Pts',(-5.85422031115392,-3.3985616580515,87.8648859059757));
#30587=CARTESIAN_POINT('Ctrl Pts',(-5.7654507560255,-3.54708544711929,87.8730216243686));
#30588=CARTESIAN_POINT('Ctrl Pts',(-5.67103007503556,-3.69211414883698,
87.8811573427614));
#30589=CARTESIAN_POINT('Ctrl Pts',(-5.57668487857314,-3.837026907491,87.8892865570617));
#30590=CARTESIAN_POINT('Ctrl Pts',(-5.47669775020504,-3.97844983723052,
87.8974157713619));
#30591=CARTESIAN_POINT('Ctrl Pts',(-5.37136206363486,-4.11591527868885,
87.9055449856621));
#30592=CARTESIAN_POINT('Ctrl Pts',(-5.26608843944813,-4.2532997273401,87.9136694103375));
#30593=CARTESIAN_POINT('Ctrl Pts',(-5.15547275458676,-4.38673104168613,
87.9217938350129));
#30594=CARTESIAN_POINT('Ctrl Pts',(-5.03985145501215,-4.51577084354509,
87.9299182596883));
#30595=CARTESIAN_POINT('Ctrl Pts',(-4.92352826013205,-4.6455939996085,87.9380920048226));
#30596=CARTESIAN_POINT('Ctrl Pts',(-4.80213868188773,-4.77097183557626,
87.9462657499568));
#30597=CARTESIAN_POINT('Ctrl Pts',(-4.67606661960873,-4.89149158938058,
87.954439495091));
#30598=CARTESIAN_POINT('Ctrl Pts',(-4.55080188592547,-5.01123956994793,
87.9625608979531));
#30599=CARTESIAN_POINT('Ctrl Pts',(-4.42091474696742,-5.12619126677077,
87.9706823008152));
#30600=CARTESIAN_POINT('Ctrl Pts',(-4.28681860625293,-5.23597891870123,
87.9788037036774));
#30601=CARTESIAN_POINT('Ctrl Pts',(-4.15271209793107,-5.34577505883473,
87.9869257344436));
#30602=CARTESIAN_POINT('Ctrl Pts',(-4.01439622280726,-5.45040612690525,
87.9950477652099));
#30603=CARTESIAN_POINT('Ctrl Pts',(-3.87231710880319,-5.5495449551175,88.0031697959761));
#30604=CARTESIAN_POINT('Ctrl Pts',(-3.73019995484619,-5.64871032654397,
88.0112940013172));
#30605=CARTESIAN_POINT('Ctrl Pts',(-3.58431785579056,-5.74238032078009,
88.0194182066583));
#30606=CARTESIAN_POINT('Ctrl Pts',(-3.43514547672217,-5.83027139623493,
88.0275424119994));
#30607=CARTESIAN_POINT('Ctrl Pts',(-3.28435840986844,-5.91911383176637,
88.0357545562419));
#30608=CARTESIAN_POINT('Ctrl Pts',(-3.13020974698006,-6.00205131654749,
88.0439667004844));
#30609=CARTESIAN_POINT('Ctrl Pts',(-2.9732139894315,-6.07883932778691,88.0521788447269));
#30610=CARTESIAN_POINT('Ctrl Pts',(-2.81765143011832,-6.15492634911473,
88.0603160211433));
#30611=CARTESIAN_POINT('Ctrl Pts',(-2.65929390137479,-6.22497561527429,
88.0684531975598));
#30612=CARTESIAN_POINT('Ctrl Pts',(-2.4986604103372,-6.28879838711765,88.0765903739762));
#30613=CARTESIAN_POINT('Ctrl Pts',(-2.33580704418711,-6.35350315798818,
88.0848400021317));
#30614=CARTESIAN_POINT('Ctrl Pts',(-2.17061471981748,-6.41180794955711,
88.0930896302872));
#30615=CARTESIAN_POINT('Ctrl Pts',(-2.00363795570425,-6.46356897870374,
88.1013392584427));
#30616=CARTESIAN_POINT('Ctrl Pts',(-1.83666119159103,-6.51533000785037,
88.1095888865982));
#30617=CARTESIAN_POINT('Ctrl Pts',(-1.66790037577361,-6.56054723609679,
88.1178385147536));
#30618=CARTESIAN_POINT('Ctrl Pts',(-1.49791805174984,-6.59913104205713,
88.1260881429091));
#30619=CARTESIAN_POINT('Ctrl Pts',(-1.32844591357875,-6.63759904237675,
88.1343130105867));
#30620=CARTESIAN_POINT('Ctrl Pts',(-1.15725305690841,-6.66958853701086,
88.1425378782643));
#30621=CARTESIAN_POINT('Ctrl Pts',(-0.984875954207333,-6.69494647886181,
88.1507627459419));
#30622=CARTESIAN_POINT('Ctrl Pts',(-0.81269305360654,-6.72027585215297,
88.1589783473854));
#30623=CARTESIAN_POINT('Ctrl Pts',(-0.639328915393011,-6.7389884979571,
88.167193948829));
#30624=CARTESIAN_POINT('Ctrl Pts',(-0.465332937994383,-6.75098172540983,
88.1754095502725));
#30625=CARTESIAN_POINT('Ctrl Pts',(-0.291498027256431,-6.76296385082949,
88.1836175466006));
#30626=CARTESIAN_POINT('Ctrl Pts',(-0.117032797816354,-6.76823892085928,
88.1918255429288));
#30627=CARTESIAN_POINT('Ctrl Pts',(0.0575053513952854,-6.76675565796201,
88.2000335392569));
#30628=CARTESIAN_POINT('Ctrl Pts',(0.231916988957002,-6.76527347018808,
88.2082355861284));
#30629=CARTESIAN_POINT('Ctrl Pts',(0.406401083709792,-6.75704270978331,
88.2164376329998));
#30630=CARTESIAN_POINT('Ctrl Pts',(0.580397242535718,-6.74206407866737,
88.2246396798713));
#30631=CARTESIAN_POINT('Ctrl Pts',(0.754302222551982,-6.72709329676928,
88.2328374286428));
#30632=CARTESIAN_POINT('Ctrl Pts',(0.927719419418191,-6.70538171927751,
88.2410351774144));
#30633=CARTESIAN_POINT('Ctrl Pts',(1.10009048385972,-6.67698209727429,88.249232926186));
#30634=CARTESIAN_POINT('Ctrl Pts',(1.27242867198254,-6.64858789192859,88.2574291114016));
#30635=CARTESIAN_POINT('Ctrl Pts',(1.44372077046563,-6.61350823505483,88.2656252966172));
#30636=CARTESIAN_POINT('Ctrl Pts',(1.6134152756098,-6.57184754452117,88.2738214818329));
#30637=CARTESIAN_POINT('Ctrl Pts',(1.78309722713759,-6.53018993595135,88.2820170607132));
#30638=CARTESIAN_POINT('Ctrl Pts',(1.95118147200846,-6.48195234798002,88.2902126395935));
#30639=CARTESIAN_POINT('Ctrl Pts',(2.11712845311619,-6.42728995090512,88.2984082184739));
#30640=CARTESIAN_POINT('Ctrl Pts',(2.28309334992864,-6.37262165245521,88.3066046821523));
#30641=CARTESIAN_POINT('Ctrl Pts',(2.44692018238773,-6.31152727527567,88.3148011458308));
#30642=CARTESIAN_POINT('Ctrl Pts',(2.608086216873,-6.24421134214379,88.3229976095092));
#30643=CARTESIAN_POINT('Ctrl Pts',(2.76929897328441,-6.17687589416768,88.331196449337));
#30644=CARTESIAN_POINT('Ctrl Pts',(2.92784906423909,-6.10331543591301,88.3393952891648));
#30645=CARTESIAN_POINT('Ctrl Pts',(3.08323529220617,-6.02378196259579,88.3475941289926));
#30646=CARTESIAN_POINT('Ctrl Pts',(3.23878382550873,-5.94416541430314,88.3558015327418));
#30647=CARTESIAN_POINT('Ctrl Pts',(3.39116157352667,-5.85856354998363,88.364008936491));
#30648=CARTESIAN_POINT('Ctrl Pts',(3.53989256732983,-5.7672740191327,88.3722163402403));
#30649=CARTESIAN_POINT('Ctrl Pts',(3.68870322932408,-5.67593558877802,88.3804281403093));
#30650=CARTESIAN_POINT('Ctrl Pts',(3.83386294492437,-5.57890361760862,88.3886399403783));
#30651=CARTESIAN_POINT('Ctrl Pts',(3.97492625272948,-5.47651808043779,88.3968517404473));
#30652=CARTESIAN_POINT('Ctrl Pts',(4.11619722543429,-5.37398181745003,88.4050756294335));
#30653=CARTESIAN_POINT('Ctrl Pts',(4.25335945656462,-5.26607645997574,88.4132995184196));
#30654=CARTESIAN_POINT('Ctrl Pts',(4.38600100006403,-5.15318195171074,88.4215234074058));
#30655=CARTESIAN_POINT('Ctrl Pts',(4.50855949317275,-5.04886937777519,88.4291221386558));
#30656=CARTESIAN_POINT('Ctrl Pts',(4.62725871104192,-4.94029791892675,88.4367208699058));
#30657=CARTESIAN_POINT('Ctrl Pts',(4.74180331890803,-4.82779352135039,88.4443196011557));
#30658=CARTESIAN_POINT('Ctrl Pts',(4.86578612535438,-4.70601903358597,88.4525444494778));
#30659=CARTESIAN_POINT('Ctrl Pts',(4.9852489806452,-4.5792945540232,88.4607692977998));
#30660=CARTESIAN_POINT('Ctrl Pts',(5.09977311128348,-4.44798867055999,88.4689941461218));
#30661=CARTESIAN_POINT('Ctrl Pts',(5.21416826235842,-4.31683066663464,88.477209731441));
#30662=CARTESIAN_POINT('Ctrl Pts',(5.32363553066573,-4.18110180095576,88.4854253167602));
#30663=CARTESIAN_POINT('Ctrl Pts',(5.42779151894399,-4.04120875814152,88.4936409020794));
#30664=CARTESIAN_POINT('Ctrl Pts',(5.53185113149757,-3.90144515861328,88.5018488855027));
#30665=CARTESIAN_POINT('Ctrl Pts',(5.63060903851758,-3.75752534147557,88.5100568689259));
#30666=CARTESIAN_POINT('Ctrl Pts',(5.72372077095539,-3.60989051580983,88.5182648523491));
#30667=CARTESIAN_POINT('Ctrl Pts',(5.81676504890371,-3.46236264370985,88.5264668895257));
#30668=CARTESIAN_POINT('Ctrl Pts',(5.90417110886795,-3.31112542592446,88.5346689267022));
#30669=CARTESIAN_POINT('Ctrl Pts',(5.98563659266067,-3.15665069030476,88.5428709638787));
#30670=CARTESIAN_POINT('Ctrl Pts',(6.06705941804239,-3.00225684350394,88.5510687061581));
#30671=CARTESIAN_POINT('Ctrl Pts',(6.14254769732389,-2.844629172746,88.5592664484375));
#30672=CARTESIAN_POINT('Ctrl Pts',(6.21184396533849,-2.68426592391436,88.5674641907169));
#30673=CARTESIAN_POINT('Ctrl Pts',(6.28112705781444,-2.5239331655008,88.5756603743312));
#30674=CARTESIAN_POINT('Ctrl Pts',(6.34422033618203,-2.36086619156955,88.5838565579456));
#30675=CARTESIAN_POINT('Ctrl Pts',(6.40091350225666,-2.19558542002547,88.59205274156));
#30676=CARTESIAN_POINT('Ctrl Pts',(6.45760249492325,-2.03031681545225,88.6002483218208));
#30677=CARTESIAN_POINT('Ctrl Pts',(6.5078921963106,-1.86283507694031,88.6084439020817));
#30678=CARTESIAN_POINT('Ctrl Pts',(6.55162146372919,-1.69367800836019,88.6166394823426));
#30679=CARTESIAN_POINT('Ctrl Pts',(6.59535546808648,-1.52450261597294,88.6248359503833));
#30680=CARTESIAN_POINT('Ctrl Pts',(6.63252753280762,-1.35365187943672,88.633032418424));
#30681=CARTESIAN_POINT('Ctrl Pts',(6.66302712934105,-1.18167612892247,88.6412288864647));
#30682=CARTESIAN_POINT('Ctrl Pts',(6.69353557878362,-1.00965046018414,88.6494277336381));
#30683=CARTESIAN_POINT('Ctrl Pts',(6.71736763959185,-0.836499480249944,
88.6576265808115));
#30684=CARTESIAN_POINT('Ctrl Pts',(6.73446436328804,-0.662781064608349,
88.6658254279849));
#30685=CARTESIAN_POINT('Ctrl Pts',(6.75157895472304,-0.48888109632954,88.6740328437509));
#30686=CARTESIAN_POINT('Ctrl Pts',(6.76194411068771,-0.314412865139171,
88.6822402595168));
#30687=CARTESIAN_POINT('Ctrl Pts',(6.76555292931201,-0.139937702845619,
88.6904476752827));
#30688=CARTESIAN_POINT('Ctrl Pts',(6.76916368213616,0.0346309719982851,
88.6986594899349));
#30689=CARTESIAN_POINT('Ctrl Pts',(6.76601088522337,0.209206226919585,88.706871304587));
#30690=CARTESIAN_POINT('Ctrl Pts',(6.75613973648387,0.3832295149173,88.7150831192392));
#30691=CARTESIAN_POINT('Ctrl Pts',(6.7462540509772,0.557509078662265,88.7233070270368));
#30692=CARTESIAN_POINT('Ctrl Pts',(6.72963027535547,0.731234693812542,88.7315309348344));
#30693=CARTESIAN_POINT('Ctrl Pts',(6.70636535089734,0.903854402148699,88.739754842632));
#30694=CARTESIAN_POINT('Ctrl Pts',(6.6848689903614,1.06335182466049,88.7473535815555));
#30695=CARTESIAN_POINT('Ctrl Pts',(6.65770341198288,1.22190497617399,88.7549523204789));
#30696=CARTESIAN_POINT('Ctrl Pts',(6.62498316933598,1.37908919436523,88.7625510594024));
#30697=CARTESIAN_POINT('Ctrl Pts',(6.58988221675236,1.54771006460649,88.7707026791055));
#30698=CARTESIAN_POINT('Ctrl Pts',(6.54828423870661,1.7152548674017,88.7788542988085));
#30699=CARTESIAN_POINT('Ctrl Pts',(6.50026562115968,1.88117937857333,88.7870059185115));
#30700=CARTESIAN_POINT('Ctrl Pts',(6.45230358230907,2.0469083865629,88.7951479334396));
#30701=CARTESIAN_POINT('Ctrl Pts',(6.3979360646495,2.21102055561252,88.8032899483676));
#30702=CARTESIAN_POINT('Ctrl Pts',(6.33729074034879,2.37298020899658,88.8114319632957));
#30703=CARTESIAN_POINT('Ctrl Pts',(6.27670410897857,2.53478311679824,88.8195660983299));
#30704=CARTESIAN_POINT('Ctrl Pts',(6.20985189507299,2.69443731640079,88.8277002333642));
#30705=CARTESIAN_POINT('Ctrl Pts',(6.13691200674627,2.85142070229096,88.8358343683984));
#30706=CARTESIAN_POINT('Ctrl Pts',(6.0640273681515,3.00828517807325,88.8439623420744));
#30707=CARTESIAN_POINT('Ctrl Pts',(5.98506439115894,3.1624825384342,88.8520903157505));
#30708=CARTESIAN_POINT('Ctrl Pts',(5.90024966940371,3.3135091426917,88.8602182894265));
#30709=CARTESIAN_POINT('Ctrl Pts',(5.8154800593316,3.46445541815515,88.8683419399548));
#30710=CARTESIAN_POINT('Ctrl Pts',(5.72486508178144,3.61223397800653,88.8764655904831));
#30711=CARTESIAN_POINT('Ctrl Pts',(5.62867799410391,3.75636433785255,88.8845892410114));
#30712=CARTESIAN_POINT('Ctrl Pts',(5.53251724504356,3.90045523092123,88.8927106670652));
#30713=CARTESIAN_POINT('Ctrl Pts',(5.4307876259904,4.04089960855886,88.900832093119));
#30714=CARTESIAN_POINT('Ctrl Pts',(5.32380661113034,4.17724456637206,88.9089535191728));
#30715=CARTESIAN_POINT('Ctrl Pts',(5.21683452069907,4.31357815019644,88.9170742677317));
#30716=CARTESIAN_POINT('Ctrl Pts',(5.10461213274398,4.44581270751718,88.9251950162907));
#30717=CARTESIAN_POINT('Ctrl Pts',(4.98749819833177,4.57352716419586,88.9333157648496));
#30718=CARTESIAN_POINT('Ctrl Pts',(4.87037173414231,4.7012552847797,88.9414373822306));
#30719=CARTESIAN_POINT('Ctrl Pts',(4.7483529294541,4.82446207291372,88.9495589996116));
#30720=CARTESIAN_POINT('Ctrl Pts',(4.62183845456009,4.94276221357548,88.9576806169926));
#30721=CARTESIAN_POINT('Ctrl Pts',(4.49523238084849,5.06114800572506,88.9658081145747));
#30722=CARTESIAN_POINT('Ctrl Pts',(4.3641244028324,5.17461980434966,88.9739356121568));
#30723=CARTESIAN_POINT('Ctrl Pts',(4.22894592839778,5.2828311855186,88.9820631097388));
#30724=CARTESIAN_POINT('Ctrl Pts',(4.09371401733998,5.3910853431046,88.9901938201551));
#30725=CARTESIAN_POINT('Ctrl Pts',(3.95440869625667,5.49407472060417,88.9983245305714));
#30726=CARTESIAN_POINT('Ctrl Pts',(3.81149139010395,5.59149554083373,89.0064552409876));
#30727=CARTESIAN_POINT('Ctrl Pts',(3.66841558133587,5.6890244057446,89.0145949687783));
#30728=CARTESIAN_POINT('Ctrl Pts',(3.52172009509385,5.78097218249617,89.022734696569));
#30729=CARTESIAN_POINT('Ctrl Pts',(3.37189273683585,5.86708005495695,89.0308744243598));
#30730=CARTESIAN_POINT('Ctrl Pts',(3.28207589654922,5.91869904576178,89.035753937951));
#30731=CARTESIAN_POINT('Ctrl Pts',(3.19113403238152,5.968220287335,89.0406334515422));
#30732=CARTESIAN_POINT('Ctrl Pts',(3.09917575053266,6.01559628526635,89.0455129651334));
#30733=CARTESIAN_POINT('Ctrl Pts',(3.09917575053243,6.01559628526647,87.0457515827423));
#30734=CARTESIAN_POINT('Ctrl Pts',(2.93382384459255,6.10078395293764,87.0545010306547));
#30735=CARTESIAN_POINT('Ctrl Pts',(2.76495772122979,6.17915010267051,87.0632504785671));
#30736=CARTESIAN_POINT('Ctrl Pts',(2.59315093316712,6.25042856433177,87.0719999264795));
#30737=CARTESIAN_POINT('Ctrl Pts',(2.42134553245623,6.32170645041449,87.0807493037395));
#30738=CARTESIAN_POINT('Ctrl Pts',(2.24659977927601,6.38589665313454,87.0894986809995));
#30739=CARTESIAN_POINT('Ctrl Pts',(2.06950718689934,6.4427811543907,87.0982480582595));
#30740=CARTESIAN_POINT('Ctrl Pts',(1.89241596572869,6.49966521519722,87.1069973677741));
#30741=CARTESIAN_POINT('Ctrl Pts',(1.71297821457197,6.54924360009546,87.1157466772888));
#30742=CARTESIAN_POINT('Ctrl Pts',(1.53180337335836,6.59134792173558,87.1244959868035));
#30743=CARTESIAN_POINT('Ctrl Pts',(1.35062987477773,6.63345193135307,87.1332452314796));
#30744=CARTESIAN_POINT('Ctrl Pts',(1.16771959102941,6.6680819236824,87.1419944761557));
#30745=CARTESIAN_POINT('Ctrl Pts',(0.983693746906729,6.6951202836317,87.1507437208318));
#30746=CARTESIAN_POINT('Ctrl Pts',(0.799669205419738,6.72215845218869,87.159492903576));
#30747=CARTESIAN_POINT('Ctrl Pts',(0.614529402873325,6.74160505424581,87.1682420863202));
#30748=CARTESIAN_POINT('Ctrl Pts',(0.42890312736308,6.75339404354123,87.1769912690644));
#30749=CARTESIAN_POINT('Ctrl Pts',(0.243278104163717,6.76518295330331,87.185740392783));
#30750=CARTESIAN_POINT('Ctrl Pts',(0.0571669005389611,6.76931433552276,
87.1944895165016));
#30751=CARTESIAN_POINT('Ctrl Pts',(-0.128798404777663,6.76577415902473,
87.2032386402202));
#30752=CARTESIAN_POINT('Ctrl Pts',(-0.314762517259356,6.7622340052344,87.2119877078194));
#30753=CARTESIAN_POINT('Ctrl Pts',(-0.500580446819875,6.75102239665086,
87.2207367754186));
#30754=CARTESIAN_POINT('Ctrl Pts',(-0.685621118843082,6.73217741012493,
87.2294858430178));
#30755=CARTESIAN_POINT('Ctrl Pts',(-0.870660665414926,6.71333253821766,
87.2382348574036));
#30756=CARTESIAN_POINT('Ctrl Pts',(-1.05492267885527,6.68685441030606,87.2469838717894));
#30757=CARTESIAN_POINT('Ctrl Pts',(-1.23778137635289,6.6528329502817,87.2557328861752));
#30758=CARTESIAN_POINT('Ctrl Pts',(-1.42999922978883,6.61707018861857,87.2649296965426));
#30759=CARTESIAN_POINT('Ctrl Pts',(-1.6206660123373,6.57297172934404,87.2741265069099));
#30760=CARTESIAN_POINT('Ctrl Pts',(-1.80906628500419,6.52070304311285,87.2833233172773));
#30761=CARTESIAN_POINT('Ctrl Pts',(-1.98831342545562,6.4709737491502,87.2920733150151));
#30762=CARTESIAN_POINT('Ctrl Pts',(-2.16550875896737,6.41384933989517,87.3008233127529));
#30763=CARTESIAN_POINT('Ctrl Pts',(-2.34005036714048,6.34952386240462,87.3095733104906));
#30764=CARTESIAN_POINT('Ctrl Pts',(-2.51458843547125,6.28519968948581,87.3183231307715));
#30765=CARTESIAN_POINT('Ctrl Pts',(-2.68647261718091,6.21367483971083,87.3270729510524));
#30766=CARTESIAN_POINT('Ctrl Pts',(-2.85511905908767,6.13519226743827,87.3358227713332));
#30767=CARTESIAN_POINT('Ctrl Pts',(-3.02376230488914,6.05671118252922,87.3445724257918));
#30768=CARTESIAN_POINT('Ctrl Pts',(-3.18916767379929,5.9712727599262,87.3533220802503));
#30769=CARTESIAN_POINT('Ctrl Pts',(-3.35077334102807,5.87916720437986,87.3620717347088));
#30770=CARTESIAN_POINT('Ctrl Pts',(-3.51237616037396,5.78706327195626,87.3708212349773));
#30771=CARTESIAN_POINT('Ctrl Pts',(-3.67017916302336,5.68829258362275,87.3795707352457));
#30772=CARTESIAN_POINT('Ctrl Pts',(-3.82364636566507,5.58319061741011,87.3883202355142));
#30773=CARTESIAN_POINT('Ctrl Pts',(-3.97711106778838,5.47809036367673,87.3970695932226));
#30774=CARTESIAN_POINT('Ctrl Pts',(-4.12623987481963,5.36665920043197,87.405818950931));
#30775=CARTESIAN_POINT('Ctrl Pts',(-4.27052628213961,5.24927559512309,87.4145683086395));
#30776=CARTESIAN_POINT('Ctrl Pts',(-4.41481053025006,5.13189374643012,87.423317535416));
#30777=CARTESIAN_POINT('Ctrl Pts',(-4.55425230136554,5.00855981477331,87.4320667621925));
#30778=CARTESIAN_POINT('Ctrl Pts',(-4.68837800630569,4.87969268192057,87.440815988969));
#30779=CARTESIAN_POINT('Ctrl Pts',(-4.82250188228921,4.75082730631783,87.4495650964399));
#30780=CARTESIAN_POINT('Ctrl Pts',(-4.95130963052998,4.61642907903491,87.4583142039107));
#30781=CARTESIAN_POINT('Ctrl Pts',(-5.07436379033404,4.47695444731647,87.4670633113816));
#30782=CARTESIAN_POINT('Ctrl Pts',(-5.19741643562824,4.33748153220563,87.4758123111713));
#30783=CARTESIAN_POINT('Ctrl Pts',(-5.31471544462775,4.19293255254586,87.484561310961));
#30784=CARTESIAN_POINT('Ctrl Pts',(-5.42586245275613,4.04379841779622,87.4933103107508));
#30785=CARTESIAN_POINT('Ctrl Pts',(-5.53702160019141,3.8946479948436,87.5020602660929));
#30786=CARTESIAN_POINT('Ctrl Pts',(-5.64202723081242,3.74091164443865,87.5108102214351));
#30787=CARTESIAN_POINT('Ctrl Pts',(-5.74052265232959,3.58311159163245,87.5195601767772));
#30788=CARTESIAN_POINT('Ctrl Pts',(-5.83901427066911,3.42531763191796,87.5283097942597));
#30789=CARTESIAN_POINT('Ctrl Pts',(-5.93099603115732,3.26346052695626,87.5370594117421));
#30790=CARTESIAN_POINT('Ctrl Pts',(-6.01615550622747,3.0980900446709,87.5458090292246));
#30791=CARTESIAN_POINT('Ctrl Pts',(-6.10131214578789,2.93272506863849,87.5545583553757));
#30792=CARTESIAN_POINT('Ctrl Pts',(-6.17964682328735,2.76384720416922,87.5633076815268));
#30793=CARTESIAN_POINT('Ctrl Pts',(-6.25089348288549,2.59203002791629,87.5720570076779));
#30794=CARTESIAN_POINT('Ctrl Pts',(-6.32213814889317,2.42021765937065,87.5808060890094));
#30795=CARTESIAN_POINT('Ctrl Pts',(-6.38629508412572,2.24546640831953,87.589555170341));
#30796=CARTESIAN_POINT('Ctrl Pts',(-6.443146398198,2.06836976660077,87.5983042516726));
#30797=CARTESIAN_POINT('Ctrl Pts',(-6.50000285283693,1.89125711158301,87.607054124107));
#30798=CARTESIAN_POINT('Ctrl Pts',(-6.54955227673245,1.71179891440271,87.6158039965413));
#30799=CARTESIAN_POINT('Ctrl Pts',(-6.59162635926384,1.53060476278437,87.6245538689758));
#30800=CARTESIAN_POINT('Ctrl Pts',(-6.63369752055196,1.349423191647,87.6333031338983));
#30801=CARTESIAN_POINT('Ctrl Pts',(-6.66829431424254,1.16650618642705,87.6420523988208));
#30802=CARTESIAN_POINT('Ctrl Pts',(-6.69529923745417,0.982474997618545,
87.6508016637433));
#30803=CARTESIAN_POINT('Ctrl Pts',(-6.72230554731443,0.798434359177744,
87.659551377923));
#30804=CARTESIAN_POINT('Ctrl Pts',(-6.74171916496703,0.613279706240354,
87.6683010921027));
#30805=CARTESIAN_POINT('Ctrl Pts',(-6.75347414817275,0.42763995365541,87.6770508062824));
#30806=CARTESIAN_POINT('Ctrl Pts',(-6.76248837758737,0.285283364199755,
87.6837604654582));
#30807=CARTESIAN_POINT('Ctrl Pts',(-6.76699999999989,0.142641701107454,
87.6904701246341));
#30808=CARTESIAN_POINT('Ctrl Pts',(-6.767,5.05731187567021E-12,87.6971797838099));
#30809=CARTESIAN_POINT('',(-6.76192617641306,-0.00322362460917852,87.3028202161898));
#30810=CARTESIAN_POINT('Ctrl Pts',(3.09917575053262,6.01559628526637,86.6513920151221));
#30811=CARTESIAN_POINT('Ctrl Pts',(2.93382384459274,6.10078395293755,86.6601414630345));
#30812=CARTESIAN_POINT('Ctrl Pts',(2.76495772122998,6.17915010267042,86.6688909109469));
#30813=CARTESIAN_POINT('Ctrl Pts',(2.59315093316732,6.25042856433169,86.6776403588593));
#30814=CARTESIAN_POINT('Ctrl Pts',(2.4213455324563,6.32170645041446,86.6863897361193));
#30815=CARTESIAN_POINT('Ctrl Pts',(2.24659977927596,6.38589665313456,86.6951391133793));
#30816=CARTESIAN_POINT('Ctrl Pts',(2.06950718689917,6.44278115439076,86.7038884906393));
#30817=CARTESIAN_POINT('Ctrl Pts',(1.89241596572852,6.49966521519727,86.712637800154));
#30818=CARTESIAN_POINT('Ctrl Pts',(1.7129782145718,6.54924360009551,86.7213871096686));
#30819=CARTESIAN_POINT('Ctrl Pts',(1.53180337335819,6.59134792173562,86.7301364191833));
#30820=CARTESIAN_POINT('Ctrl Pts',(1.35062987477756,6.6334519313531,86.7388856638594));
#30821=CARTESIAN_POINT('Ctrl Pts',(1.16771959102924,6.66808192368243,86.7476349085355));
#30822=CARTESIAN_POINT('Ctrl Pts',(0.983693746906558,6.69512028363173,86.7563841532116));
#30823=CARTESIAN_POINT('Ctrl Pts',(0.799669205419693,6.72215845218869,86.7651333359558));
#30824=CARTESIAN_POINT('Ctrl Pts',(0.61452940287341,6.74160505424579,86.7738825187));
#30825=CARTESIAN_POINT('Ctrl Pts',(0.428903127363293,6.75339404354122,86.7826317014442));
#30826=CARTESIAN_POINT('Ctrl Pts',(0.243278104164058,6.76518295330329,86.7913808251628));
#30827=CARTESIAN_POINT('Ctrl Pts',(0.0571669005394312,6.76931433552275,
86.8001299488814));
#30828=CARTESIAN_POINT('Ctrl Pts',(-0.128798404777065,6.76577415902474,
86.8088790726));
#30829=CARTESIAN_POINT('Ctrl Pts',(-0.314762517258374,6.76223400523444,
86.8176281401992));
#30830=CARTESIAN_POINT('Ctrl Pts',(-0.50058044681851,6.75102239665096,86.8263772077984));
#30831=CARTESIAN_POINT('Ctrl Pts',(-0.685621118841339,6.73217741012511,
86.8351262753976));
#30832=CARTESIAN_POINT('Ctrl Pts',(-0.870660665413061,6.7133325382179,86.8438752897833));
#30833=CARTESIAN_POINT('Ctrl Pts',(-1.05492267885329,6.68685441030637,86.8526243041691));
#30834=CARTESIAN_POINT('Ctrl Pts',(-1.23778137635079,6.65283295028209,86.8613733185549));
#30835=CARTESIAN_POINT('Ctrl Pts',(-1.42999922978674,6.61707018861903,86.8705701289223));
#30836=CARTESIAN_POINT('Ctrl Pts',(-1.62066601233522,6.57297172934456,86.8797669392896));
#30837=CARTESIAN_POINT('Ctrl Pts',(-1.80906628500213,6.52070304311342,86.888963749657));
#30838=CARTESIAN_POINT('Ctrl Pts',(-1.98831342545345,6.47097374915086,86.8977137473948));
#30839=CARTESIAN_POINT('Ctrl Pts',(-2.16550875896511,6.41384933989593,86.9064637451326));
#30840=CARTESIAN_POINT('Ctrl Pts',(-2.34005036713811,6.34952386240549,86.9152137428703));
#30841=CARTESIAN_POINT('Ctrl Pts',(-2.51458843546891,6.28519968948675,86.9239635631512));
#30842=CARTESIAN_POINT('Ctrl Pts',(-2.6864726171786,6.21367483971184,86.932713383432));
#30843=CARTESIAN_POINT('Ctrl Pts',(-2.85511905908539,6.13519226743933,86.9414632037129));
#30844=CARTESIAN_POINT('Ctrl Pts',(-3.02376230488701,6.05671118253029,86.9502128581715));
#30845=CARTESIAN_POINT('Ctrl Pts',(-3.1891676737973,5.97127275992727,86.95896251263));
#30846=CARTESIAN_POINT('Ctrl Pts',(-3.35077334102621,5.87916720438091,86.9677121670885));
#30847=CARTESIAN_POINT('Ctrl Pts',(-3.51237616037203,5.78706327195743,86.976461667357));
#30848=CARTESIAN_POINT('Ctrl Pts',(-3.67017916302135,5.68829258362404,86.9852111676254));
#30849=CARTESIAN_POINT('Ctrl Pts',(-3.82364636566299,5.58319061741154,86.9939606678938));
#30850=CARTESIAN_POINT('Ctrl Pts',(-3.97711106778634,5.47809036367821,87.0027100256023));
#30851=CARTESIAN_POINT('Ctrl Pts',(-4.12623987481763,5.36665920043351,87.0114593833107));
#30852=CARTESIAN_POINT('Ctrl Pts',(-4.27052628213765,5.24927559512468,87.0202087410192));
#30853=CARTESIAN_POINT('Ctrl Pts',(-4.41481053024835,5.1318937464316,87.0289579677957));
#30854=CARTESIAN_POINT('Ctrl Pts',(-4.55425230136406,5.00855981477467,87.0377071945722));
#30855=CARTESIAN_POINT('Ctrl Pts',(-4.68837800630443,4.87969268192178,87.0464564213487));
#30856=CARTESIAN_POINT('Ctrl Pts',(-4.82250188228808,4.75082730631899,87.0552055288196));
#30857=CARTESIAN_POINT('Ctrl Pts',(-4.95130963052897,4.61642907903601,87.0639546362904));
#30858=CARTESIAN_POINT('Ctrl Pts',(-5.07436379033314,4.4769544473175,87.0727037437613));
#30859=CARTESIAN_POINT('Ctrl Pts',(-5.19741643562762,4.33748153220639,87.081452743551));
#30860=CARTESIAN_POINT('Ctrl Pts',(-5.31471544462738,4.19293255254634,87.0902017433408));
#30861=CARTESIAN_POINT('Ctrl Pts',(-5.42586245275601,4.04379841779639,87.0989507431305));
#30862=CARTESIAN_POINT('Ctrl Pts',(-5.53702160019121,3.89464799484387,87.1077006984727));
#30863=CARTESIAN_POINT('Ctrl Pts',(-5.64202723081216,3.74091164443904,87.1164506538148));
#30864=CARTESIAN_POINT('Ctrl Pts',(-5.74052265232928,3.58311159163296,87.125200609157));
#30865=CARTESIAN_POINT('Ctrl Pts',(-5.83901427066881,3.42531763191847,87.1339502266394));
#30866=CARTESIAN_POINT('Ctrl Pts',(-5.93099603115704,3.26346052695678,87.1426998441219));
#30867=CARTESIAN_POINT('Ctrl Pts',(-6.0161555062272,3.09809004467143,87.1514494616043));
#30868=CARTESIAN_POINT('Ctrl Pts',(-6.10131214578775,2.93272506863879,87.1601987877554));
#30869=CARTESIAN_POINT('Ctrl Pts',(-6.17964682328732,2.76384720416931,87.1689481139066));
#30870=CARTESIAN_POINT('Ctrl Pts',(-6.25089348288555,2.59203002791614,87.1776974400577));
#30871=CARTESIAN_POINT('Ctrl Pts',(-6.32213814889313,2.42021765937072,87.1864465213892));
#30872=CARTESIAN_POINT('Ctrl Pts',(-6.38629508412561,2.24546640831985,87.1951956027208));
#30873=CARTESIAN_POINT('Ctrl Pts',(-6.44314639819782,2.06836976660133,87.2039446840523));
#30874=CARTESIAN_POINT('Ctrl Pts',(-6.50000285283673,1.89125711158371,87.2126945564867));
#30875=CARTESIAN_POINT('Ctrl Pts',(-6.54955227673223,1.71179891440353,87.2214444289211));
#30876=CARTESIAN_POINT('Ctrl Pts',(-6.59162635926361,1.53060476278533,87.2301943013555));
#30877=CARTESIAN_POINT('Ctrl Pts',(-6.63369752055176,1.34942319164796,87.238943566278));
#30878=CARTESIAN_POINT('Ctrl Pts',(-6.66829431424237,1.16650618642802,87.2476928312005));
#30879=CARTESIAN_POINT('Ctrl Pts',(-6.69529923745403,0.982474997619514,
87.256442096123));
#30880=CARTESIAN_POINT('Ctrl Pts',(-6.72230554731432,0.798434359178717,
87.2651918103027));
#30881=CARTESIAN_POINT('Ctrl Pts',(-6.74171916496694,0.613279706241331,
87.2739415244824));
#30882=CARTESIAN_POINT('Ctrl Pts',(-6.75347414817269,0.427639953656388,
87.2826912386621));
#30883=CARTESIAN_POINT('Ctrl Pts',(-6.76248837758735,0.28528336420035,87.289400897838));
#30884=CARTESIAN_POINT('Ctrl Pts',(-6.7669999999999,0.142641701107664,87.2961105570138));
#30885=CARTESIAN_POINT('Ctrl Pts',(-6.767,4.88301307805299E-12,87.3028202161897));
#30886=CARTESIAN_POINT('Ctrl Pts',(-6.75952464934065,-0.00474942101288033,
87.3028202161898));
#30887=CARTESIAN_POINT('Ctrl Pts',(-6.76474205737662,-0.664932310615616,
87.3338345898298));
#30888=CARTESIAN_POINT('Ctrl Pts',(-6.52475900416391,-2.44944862935725,
87.4178161533712));
#30889=CARTESIAN_POINT('Ctrl Pts',(-4.9434562315809,-5.00423164848898,87.5547649068138));
#30890=CARTESIAN_POINT('Ctrl Pts',(-0.961442134084449,-7.40213597015891,
87.7666336664189));
#30891=CARTESIAN_POINT('Ctrl Pts',(5.26255964958237,-6.02988092025636,88.0314696159252));
#30892=CARTESIAN_POINT('Ctrl Pts',(7.87321604513668,1.04812428378684,88.3440128912255));
#30893=CARTESIAN_POINT('Ctrl Pts',(4.99392233188169,5.04013769176598,88.5506217867228));
#30894=CARTESIAN_POINT('Ctrl Pts',(3.10355585847744,6.02401335114973,88.6512963024177));
#30895=CARTESIAN_POINT('Origin',(0.,0.,-3.69717978381041));
#30896=CARTESIAN_POINT('',(3.09917575053275,6.01559628526631,91.0459618091817));
#30897=CARTESIAN_POINT('',(3.09917575053247,6.01559628526645,90.6515381108923));
#30898=CARTESIAN_POINT('',(3.09917575053259,6.01559628526639,-3.69717978381041));
#30899=CARTESIAN_POINT('',(-6.76699988295537,-0.00125860319137315,89.6971797837778));
#30900=CARTESIAN_POINT('Ctrl Pts',(-6.76699988295525,-0.00125860387117534,
89.6971797838099));
#30901=CARTESIAN_POINT('Ctrl Pts',(-6.76697355887306,-0.142792461478475,
89.703868333921));
#30902=CARTESIAN_POINT('Ctrl Pts',(-6.76250695607499,-0.284257024204317,
89.710556884032));
#30903=CARTESIAN_POINT('Ctrl Pts',(-6.7536127253551,-0.425445831947712,
89.7172454341431));
#30904=CARTESIAN_POINT('Ctrl Pts',(-6.74267579642089,-0.599060842084828,
89.7254701136619));
#30905=CARTESIAN_POINT('Ctrl Pts',(-6.72502547760636,-0.772482642989311,
89.7336947931806));
#30906=CARTESIAN_POINT('Ctrl Pts',(-6.70066978690113,-0.945152583930449,
89.7419194726994));
#30907=CARTESIAN_POINT('Ctrl Pts',(-6.67633969678227,-1.11764102922893,
89.7501355071496));
#30908=CARTESIAN_POINT('Ctrl Pts',(-6.64531831969244,-1.28937883632884,
89.7583515415997));
#30909=CARTESIAN_POINT('Ctrl Pts',(-6.60766562973601,-1.45980955114203,
89.7665675760498));
#30910=CARTESIAN_POINT('Ctrl Pts',(-6.57004497511633,-1.6300952615651,89.7747766202044));
#30911=CARTESIAN_POINT('Ctrl Pts',(-6.52580432121743,-1.7990757465476,89.782985664359));
#30912=CARTESIAN_POINT('Ctrl Pts',(-6.47505518311067,-1.96620176372407,
89.7911947085136));
#30913=CARTESIAN_POINT('Ctrl Pts',(-6.42433906067716,-2.13321905436489,
89.7993984121416));
#30914=CARTESIAN_POINT('Ctrl Pts',(-6.367122991954,-2.29838393861884,89.8076021157697));
#30915=CARTESIAN_POINT('Ctrl Pts',(-6.30356912565913,-2.46115933617413,
89.8158058193977));
#30916=CARTESIAN_POINT('Ctrl Pts',(-6.2400438815928,-2.62386142592137,89.8240058283917));
#30917=CARTESIAN_POINT('Ctrl Pts',(-6.17018665659501,-2.78417583974394,
89.8322058373856));
#30918=CARTESIAN_POINT('Ctrl Pts',(-6.09420884250469,-2.94158249653781,
89.8404058463796));
#30919=CARTESIAN_POINT('Ctrl Pts',(-6.0182371037608,-3.09897656676307,89.8486051996835));
#30920=CARTESIAN_POINT('Ctrl Pts',(-5.93614589857633,-3.25346301675257,
89.8568045529875));
#30921=CARTESIAN_POINT('Ctrl Pts',(-5.84819413800976,-3.40454318876239,
89.8650039062914));
#30922=CARTESIAN_POINT('Ctrl Pts',(-5.76024295086259,-3.55562237577426,
89.873203206138));
#30923=CARTESIAN_POINT('Ctrl Pts',(-5.66643146387409,-3.70329501865751,
89.8814025059846));
#30924=CARTESIAN_POINT('Ctrl Pts',(-5.56706373077756,-3.84708856376624,
89.8896018058312));
#30925=CARTESIAN_POINT('Ctrl Pts',(-5.46767861924757,-3.99090725694346,
89.8978025396542));
#30926=CARTESIAN_POINT('Ctrl Pts',(-5.36273552941765,-4.13084520576755,
89.9060032734772));
#30927=CARTESIAN_POINT('Ctrl Pts',(-5.25258090816052,-4.26646021934198,
89.9142040073002));
#30928=CARTESIAN_POINT('Ctrl Pts',(-5.14238703860357,-4.40212355280216,
89.9224076630601));
#30929=CARTESIAN_POINT('Ctrl Pts',(-5.02697816451822,-4.53346060460891,
89.9306113188201));
#30930=CARTESIAN_POINT('Ctrl Pts',(-4.90673996530744,-4.66006350953018,
89.9388149745801));
#30931=CARTESIAN_POINT('Ctrl Pts',(-4.78636402550986,-4.78681144621781,
89.9470280281551));
#30932=CARTESIAN_POINT('Ctrl Pts',(-4.6611479550591,-4.90881414094584,89.9552410817301));
#30933=CARTESIAN_POINT('Ctrl Pts',(-4.53151390459832,-5.02570101900542,
89.9634541353051));
#30934=CARTESIAN_POINT('Ctrl Pts',(-4.40180314676163,-5.14265706165303,
89.9716720487282));
#30935=CARTESIAN_POINT('Ctrl Pts',(-4.26766947270954,-5.25449102419909,
89.9798899621513));
#30936=CARTESIAN_POINT('Ctrl Pts',(-4.12956674215047,-5.36087376480036,
89.9881078755744));
#30937=CARTESIAN_POINT('Ctrl Pts',(-3.99124861791615,-5.46742242659224,
89.9963386061704));
#30938=CARTESIAN_POINT('Ctrl Pts',(-3.84894935823525,-5.56850266818713,
90.0045693367663));
#30939=CARTESIAN_POINT('Ctrl Pts',(-3.70315145376962,-5.66382894431355,
90.0128000673623));
#30940=CARTESIAN_POINT('Ctrl Pts',(-3.56925351561354,-5.75137472813128,
90.0203590090382));
#30941=CARTESIAN_POINT('Ctrl Pts',(-3.43240522942697,-5.83406791005637,
90.0279179507141));
#30942=CARTESIAN_POINT('Ctrl Pts',(-3.29299648027131,-5.91172252232129,
90.0354768923899));
#30943=CARTESIAN_POINT('Ctrl Pts',(-3.1426151231373,-5.99548918726047,90.0436307845567));
#30944=CARTESIAN_POINT('Ctrl Pts',(-2.9887890810726,-6.073651259737,90.0517846767234));
#30945=CARTESIAN_POINT('Ctrl Pts',(-2.83197802127408,-6.14590835328844,
90.0599385688901));
#30946=CARTESIAN_POINT('Ctrl Pts',(-2.67535831477922,-6.21807727299817,
90.0680825110304));
#30947=CARTESIAN_POINT('Ctrl Pts',(-2.51576116957472,-6.284355405633,90.0762264531705));
#30948=CARTESIAN_POINT('Ctrl Pts',(-2.35367362196189,-6.34448654197334,
90.0843703953107));
#30949=CARTESIAN_POINT('Ctrl Pts',(-2.1917497502459,-6.40455695793254,90.0925061137036));
#30950=CARTESIAN_POINT('Ctrl Pts',(-2.02734082285004,-6.45849260875372,
90.1006418320966));
#30951=CARTESIAN_POINT('Ctrl Pts',(-1.86095677945185,-6.50608398846896,
90.1087775504895));
#30952=CARTESIAN_POINT('Ctrl Pts',(-1.69470575162617,-6.55363732129888,
90.1169067647897));
#30953=CARTESIAN_POINT('Ctrl Pts',(-1.52648310167053,-6.59485638166404,
90.1250359790899));
#30954=CARTESIAN_POINT('Ctrl Pts',(-1.35681697417567,-6.62958043156494,
90.1331651933901));
#30955=CARTESIAN_POINT('Ctrl Pts',(-1.18725081170344,-6.66428402251811,
90.1412896180655));
#30956=CARTESIAN_POINT('Ctrl Pts',(-1.0162432227095,-6.69250015074158,90.1494140427409));
#30957=CARTESIAN_POINT('Ctrl Pts',(-0.844335673570511,-6.71411842838181,
90.1575384674163));
#30958=CARTESIAN_POINT('Ctrl Pts',(-0.671384535558887,-6.7358679428066,
90.1657122125505));
#30959=CARTESIAN_POINT('Ctrl Pts',(-0.497522835850102,-6.75093913494648,
90.1738859576847));
#30960=CARTESIAN_POINT('Ctrl Pts',(-0.323311073628327,-6.75927207246974,
90.1820597028189));
#30961=CARTESIAN_POINT('Ctrl Pts',(-0.15021491255361,-6.7675516482995,90.190181105681));
#30962=CARTESIAN_POINT('Ctrl Pts',(0.0232264698307039,-6.76917902219835,
90.1983025085432));
#30963=CARTESIAN_POINT('Ctrl Pts',(0.19645980411135,-6.76414758453484,90.2064239114053));
#30964=CARTESIAN_POINT('Ctrl Pts',(0.369706531881311,-6.75911575786707,
90.2145459421716));
#30965=CARTESIAN_POINT('Ctrl Pts',(0.542744813668747,-6.74742410473295,
90.2226679729378));
#30966=CARTESIAN_POINT('Ctrl Pts',(0.715023288481733,-6.72911812178452,
90.2307900037041));
#30967=CARTESIAN_POINT('Ctrl Pts',(0.887347888759076,-6.710807237632,90.2389142090452));
#30968=CARTESIAN_POINT('Ctrl Pts',(1.05891191321258,-6.68587853612958,90.2470384143864));
#30969=CARTESIAN_POINT('Ctrl Pts',(1.22917105937705,-6.65442916460833,90.2551626197275));
#30970=CARTESIAN_POINT('Ctrl Pts',(1.40127314298828,-6.62263937540169,90.2633747639699));
#30971=CARTESIAN_POINT('Ctrl Pts',(1.57204155703373,-6.58418699685215,90.2715869082123));
#30972=CARTESIAN_POINT('Ctrl Pts',(1.74092750534122,-6.53922475689178,90.2797990524548));
#30973=CARTESIAN_POINT('Ctrl Pts',(1.90827171107745,-6.49467297262735,90.2879362288712));
#30974=CARTESIAN_POINT('Ctrl Pts',(2.07376734684281,-6.44372985590002,90.2960734052877));
#30975=CARTESIAN_POINT('Ctrl Pts',(2.23689879097849,-6.38659320756528,90.3042105817041));
#30976=CARTESIAN_POINT('Ctrl Pts',(2.40228463069688,-6.32866695911207,90.3124602098595));
#30977=CARTESIAN_POINT('Ctrl Pts',(2.56524009130338,-6.26437488644009,90.3207098380149));
#30978=CARTESIAN_POINT('Ctrl Pts',(2.72525221586998,-6.1939720180104,90.3289594661703));
#30979=CARTESIAN_POINT('Ctrl Pts',(2.88526434043657,-6.12356914958071,90.3372090943257));
#30980=CARTESIAN_POINT('Ctrl Pts',(3.04233281075082,-6.04705571077292,90.3454587224811));
#30981=CARTESIAN_POINT('Ctrl Pts',(3.19597412377447,-5.96473288590227,90.3537083506365));
#30982=CARTESIAN_POINT('Ctrl Pts',(3.34915429694435,-5.88265714519587,90.3619332183141));
#30983=CARTESIAN_POINT('Ctrl Pts',(3.4993858102387,-5.79456166088951,90.3701580859917));
#30984=CARTESIAN_POINT('Ctrl Pts',(3.64616325782922,-5.70068263432163,90.3783829536693));
#30985=CARTESIAN_POINT('Ctrl Pts',(3.7927753441963,-5.60690937298502,90.3865985551129));
#30986=CARTESIAN_POINT('Ctrl Pts',(3.93594081413043,-5.50736573556886,90.3948141565564));
#30987=CARTESIAN_POINT('Ctrl Pts',(4.07517752010596,-5.40233441945453,90.403029758));
#30988=CARTESIAN_POINT('Ctrl Pts',(4.21428533579547,-5.29740032997508,90.4112377543281));
#30989=CARTESIAN_POINT('Ctrl Pts',(4.34947134572244,-5.18698889321526,90.4194457506562));
#30990=CARTESIAN_POINT('Ctrl Pts',(4.48028107267301,-5.07142687119197,90.4276537469844));
#30991=CARTESIAN_POINT('Ctrl Pts',(4.61099598393749,-4.9559486127592,90.4358557938558));
#30992=CARTESIAN_POINT('Ctrl Pts',(4.73734066264471,-4.83532744172815,90.4440578407273));
#30993=CARTESIAN_POINT('Ctrl Pts',(4.85889245303521,-4.70993132963077,90.4522598875987));
#30994=CARTESIAN_POINT('Ctrl Pts',(4.98038054691856,-4.58460092857167,90.4604576363703));
#30995=CARTESIAN_POINT('Ctrl Pts',(5.09708050688783,-4.45450082822877,90.4686553851419));
#30996=CARTESIAN_POINT('Ctrl Pts',(5.20860534822872,-4.32003695891635,90.4768531339134));
#30997=CARTESIAN_POINT('Ctrl Pts',(5.32010891844612,-4.18559873588628,90.4850493191291));
#30998=CARTESIAN_POINT('Ctrl Pts',(5.42643910252046,-4.04679867362448,90.4932455043447));
#30999=CARTESIAN_POINT('Ctrl Pts',(5.52724796153608,-3.90407722409473,90.5014416895603));
#31000=CARTESIAN_POINT('Ctrl Pts',(5.62804936293984,-3.7613663327757,90.5096372684407));
#31001=CARTESIAN_POINT('Ctrl Pts',(5.72333004498768,-3.61473492449087,90.517832847321));
#31002=CARTESIAN_POINT('Ctrl Pts',(5.8127843664756,-3.46465393782076,90.5260284262013));
#31003=CARTESIAN_POINT('Ctrl Pts',(5.90224834548913,-3.31455674834513,90.5342248898798));
#31004=CARTESIAN_POINT('Ctrl Pts',(5.98588452699447,-3.16100954680833,90.5424213535582));
#31005=CARTESIAN_POINT('Ctrl Pts',(6.06343233179332,-3.00450950368997,90.5506178172367));
#31006=CARTESIAN_POINT('Ctrl Pts',(6.14100261764907,-2.8479640913135,90.5588166570645));
#31007=CARTESIAN_POINT('Ctrl Pts',(6.21248085183368,-2.68846445370207,90.5670154968923));
#31008=CARTESIAN_POINT('Ctrl Pts',(6.27765384261681,-2.52652948375403,90.5752143367201));
#31009=CARTESIAN_POINT('Ctrl Pts',(6.34289490844288,-2.36442536812308,90.5834217404693));
#31010=CARTESIAN_POINT('Ctrl Pts',(6.40181743873401,-2.1998811713549,90.5916291442185));
#31011=CARTESIAN_POINT('Ctrl Pts',(6.45425722505974,-2.03343371486855,90.5998365479678));
#31012=CARTESIAN_POINT('Ctrl Pts',(6.50672510091013,-1.86689710031616,90.6080483480368));
#31013=CARTESIAN_POINT('Ctrl Pts',(6.55270321587474,-1.69845553951099,90.6162601481058));
#31014=CARTESIAN_POINT('Ctrl Pts',(6.59207814784328,-1.52865780759695,90.6244719481749));
#31015=CARTESIAN_POINT('Ctrl Pts',(6.6315110452135,-1.35861010969589,90.632695837161));
#31016=CARTESIAN_POINT('Ctrl Pts',(6.66432126536162,-1.18720260322624,90.6409197261471));
#31017=CARTESIAN_POINT('Ctrl Pts',(6.6904468984214,-1.01499226568656,90.6491436151333));
#31018=CARTESIAN_POINT('Ctrl Pts',(6.71458653171343,-0.855872890940896,
90.6567423463834));
#31019=CARTESIAN_POINT('Ctrl Pts',(6.73301979156511,-0.69606838245863,90.6643410776335));
#31020=CARTESIAN_POINT('Ctrl Pts',(6.74573740825346,-0.536018487451575,
90.6719398088836));
#31021=CARTESIAN_POINT('Ctrl Pts',(6.7595029257901,-0.362780868293384,90.6801646572056));
#31022=CARTESIAN_POINT('Ctrl Pts',(6.7666100882802,-0.188769501549492,90.6883895055277));
#31023=CARTESIAN_POINT('Ctrl Pts',(6.76698438507566,-0.0145372673548326,
90.6966143538497));
#31024=CARTESIAN_POINT('Ctrl Pts',(6.76735826032995,0.159498742713185,90.7048299391689));
#31025=CARTESIAN_POINT('Ctrl Pts',(6.76101436821537,0.333754769415102,90.7130455244881));
#31026=CARTESIAN_POINT('Ctrl Pts',(6.74792988781481,0.507672363966806,90.7212611098073));
#31027=CARTESIAN_POINT('Ctrl Pts',(6.73485751450766,0.681429032253275,90.7294690932306));
#31028=CARTESIAN_POINT('Ctrl Pts',(6.71505700093106,0.854847536531307,90.7376770766538));
#31029=CARTESIAN_POINT('Ctrl Pts',(6.68855755548671,1.02736888552345,90.745885060077));
#31030=CARTESIAN_POINT('Ctrl Pts',(6.66207730747878,1.19976525198954,90.7540870972535));
#31031=CARTESIAN_POINT('Ctrl Pts',(6.62890784815014,1.37126540455445,90.7622891344301));
#31032=CARTESIAN_POINT('Ctrl Pts',(6.58913025732375,1.54131484519571,90.7704911716066));
#31033=CARTESIAN_POINT('Ctrl Pts',(6.54937349554961,1.71127524151301,90.778688913886));
#31034=CARTESIAN_POINT('Ctrl Pts',(6.50301557720924,1.87978609073229,90.7868866561654));
#31035=CARTESIAN_POINT('Ctrl Pts',(6.45018879981069,2.04630238400798,90.7950843984448));
#31036=CARTESIAN_POINT('Ctrl Pts',(6.39737206654969,2.212787016966,90.8032805820591));
#31037=CARTESIAN_POINT('Ctrl Pts',(6.33808902656848,2.37727750584865,90.8114767656735));
#31038=CARTESIAN_POINT('Ctrl Pts',(6.27252212793175,2.53924302787396,90.8196729492878));
#31039=CARTESIAN_POINT('Ctrl Pts',(6.20696005593358,2.70119662697704,90.8278685295487));
#31040=CARTESIAN_POINT('Ctrl Pts',(6.13511518033477,2.86062529645276,90.8360641098096));
#31041=CARTESIAN_POINT('Ctrl Pts',(6.05721846300543,3.01701731705771,90.8442596900705));
#31042=CARTESIAN_POINT('Ctrl Pts',(5.97931330757512,3.17342627870596,90.8524561581112));
#31043=CARTESIAN_POINT('Ctrl Pts',(5.89535516435128,3.32679761487085,90.8606526261519));
#31044=CARTESIAN_POINT('Ctrl Pts',(5.80562142392341,3.47664333547195,90.8688490941926));
#31045=CARTESIAN_POINT('Ctrl Pts',(5.71586163709679,3.62653255076492,90.877047941366));
#31046=CARTESIAN_POINT('Ctrl Pts',(5.62032309811326,3.77289380432431,90.8852467885394));
#31047=CARTESIAN_POINT('Ctrl Pts',(5.51932708963897,3.91526722939539,90.8934456357128));
#31048=CARTESIAN_POINT('Ctrl Pts',(5.41822553051475,4.05778944854036,90.9016530514787));
#31049=CARTESIAN_POINT('Ctrl Pts',(5.31165531477073,4.1963152196775,90.9098604672447));
#31050=CARTESIAN_POINT('Ctrl Pts',(5.19997928830277,4.33041619261039,90.9180678830107));
#31051=CARTESIAN_POINT('Ctrl Pts',(5.08824340741248,4.46458903894817,90.9262796976628));
#31052=CARTESIAN_POINT('Ctrl Pts',(4.97139650035427,4.59433209298243,90.9344915123149));
#31053=CARTESIAN_POINT('Ctrl Pts',(4.84983892418515,4.71925326820448,90.9427033269671));
#31054=CARTESIAN_POINT('Ctrl Pts',(4.72810233600539,4.84435840884812,90.9509272347647));
#31055=CARTESIAN_POINT('Ctrl Pts',(4.60164147498368,4.96462723234345,90.9591511425623));
#31056=CARTESIAN_POINT('Ctrl Pts',(4.47089144602487,5.07970655430623,90.9673750503599));
#31057=CARTESIAN_POINT('Ctrl Pts',(4.35008083399665,5.18603772248131,90.9749737892834));
#31058=CARTESIAN_POINT('Ctrl Pts',(4.22560891298427,5.28793871061637,90.9825725282069));
#31059=CARTESIAN_POINT('Ctrl Pts',(4.09784061972497,5.38516399521241,90.9901712671303));
#31060=CARTESIAN_POINT('Ctrl Pts',(3.96075565233607,5.48947880312157,90.9983240948073));
#31061=CARTESIAN_POINT('Ctrl Pts',(3.81946952411304,5.58871963443161,91.0064769224842));
#31062=CARTESIAN_POINT('Ctrl Pts',(3.67439693588874,5.68252550874446,91.0146297501611));
#31063=CARTESIAN_POINT('Ctrl Pts',(3.52951465418826,5.77620832831572,91.0227718829417));
#31064=CARTESIAN_POINT('Ctrl Pts',(3.38085610879501,5.86447019286279,91.0309140157223));
#31065=CARTESIAN_POINT('Ctrl Pts',(3.2288689564537,5.94699035328372,91.0390561485029));
#31066=CARTESIAN_POINT('Ctrl Pts',(3.18590021063501,5.9703198764929,91.0413580353959));
#31067=CARTESIAN_POINT('Ctrl Pts',(3.14266561864551,5.99319073505027,91.0436599222888));
#31068=CARTESIAN_POINT('Ctrl Pts',(3.09917575053275,6.01559628526631,91.0459618091817));
#31069=CARTESIAN_POINT('Ctrl Pts',(3.09917575053266,6.01559628526635,89.0455129651334));
#31070=CARTESIAN_POINT('Ctrl Pts',(2.94549603082524,6.09477055795357,89.0536675572585));
#31071=CARTESIAN_POINT('Ctrl Pts',(2.78897690056007,6.16795072432149,89.0618221493837));
#31072=CARTESIAN_POINT('Ctrl Pts',(2.63013819161377,6.23495485893961,89.0699767415088));
#31073=CARTESIAN_POINT('Ctrl Pts',(2.55997831502702,6.26455093062009,89.073578666889));
#31074=CARTESIAN_POINT('Ctrl Pts',(2.48936606853457,6.29294269471233,89.0771805922693));
#31075=CARTESIAN_POINT('Ctrl Pts',(2.41834701719733,6.32011761792554,89.0807825176495));
#31076=CARTESIAN_POINT('Ctrl Pts',(2.25604142262126,6.38222267264861,89.0890142896803));
#31077=CARTESIAN_POINT('Ctrl Pts',(2.09110366302185,6.43816268252841,89.0972460617112));
#31078=CARTESIAN_POINT('Ctrl Pts',(1.92404214632294,6.48770767060085,89.105477833742));
#31079=CARTESIAN_POINT('Ctrl Pts',(1.75718011777019,6.53719349700626,89.1136997762144));
#31080=CARTESIAN_POINT('Ctrl Pts',(1.58819972197526,6.58029940635646,89.1219217186869));
#31081=CARTESIAN_POINT('Ctrl Pts',(1.41762956869311,6.61684331127517,89.1301436611593));
#31082=CARTESIAN_POINT('Ctrl Pts',(1.24722891798956,6.65335090101215,89.1383574331492));
#31083=CARTESIAN_POINT('Ctrl Pts',(1.07524200392315,6.68330939818465,89.1465712051391));
#31084=CARTESIAN_POINT('Ctrl Pts',(0.902212927985894,6.7065863770308,89.154784977129));
#31085=CARTESIAN_POINT('Ctrl Pts',(0.729321142857274,6.72984488663859,89.1629922318594));
#31086=CARTESIAN_POINT('Ctrl Pts',(0.555389196392874,6.7464323897719,89.1711994865897));
#31087=CARTESIAN_POINT('Ctrl Pts',(0.380971819444985,6.75626742164553,89.1794067413201));
#31088=CARTESIAN_POINT('Ctrl Pts',(0.206657910601496,6.7660966191687,89.1876091273321));
#31089=CARTESIAN_POINT('Ctrl Pts',(0.0318595017268982,6.76918130516252,
89.1958115133441));
#31090=CARTESIAN_POINT('Ctrl Pts',(-0.142863013963399,6.76549178990273,
89.2040138993561));
#31091=CARTESIAN_POINT('Ctrl Pts',(-0.317533379220613,6.76180337587377,
89.2122138371548));
#31092=CARTESIAN_POINT('Ctrl Pts',(-0.492127538551597,6.75134479187953,
89.2204137749534));
#31093=CARTESIAN_POINT('Ctrl Pts',(-0.666084300259802,6.73413845305748,
89.2286137127521));
#31094=CARTESIAN_POINT('Ctrl Pts',(-0.840016738322924,6.7169345201257,89.2368125039879));
#31095=CARTESIAN_POINT('Ctrl Pts',(-1.01331159962821,6.692984745948,89.2450112952237));
#31096=CARTESIAN_POINT('Ctrl Pts',(-1.18541199675908,6.66236349938516,89.2532100864595));
#31097=CARTESIAN_POINT('Ctrl Pts',(-1.357519549718,6.63174097960983,89.2614092185959));
#31098=CARTESIAN_POINT('Ctrl Pts',(-1.52843218663935,6.59444649752415,89.2696083507323));
#31099=CARTESIAN_POINT('Ctrl Pts',(-1.69760234907644,6.55060571736768,89.2778074828688));
#31100=CARTESIAN_POINT('Ctrl Pts',(-1.86681023373675,6.50675516142291,89.2860084432797));
#31101=CARTESIAN_POINT('Ctrl Pts',(-2.03427452314954,6.45635548996661,89.2942094036906));
#31102=CARTESIAN_POINT('Ctrl Pts',(-2.19946192181757,6.39958250626356,89.3024103641015));
#31103=CARTESIAN_POINT('Ctrl Pts',(-2.36480414084381,6.34275631260779,89.3106190107866));
#31104=CARTESIAN_POINT('Ctrl Pts',(-2.52786486612134,6.27954498901384,89.3188276574716));
#31105=CARTESIAN_POINT('Ctrl Pts',(-2.68812904233416,6.21017320626081,89.3270363041567));
#31106=CARTESIAN_POINT('Ctrl Pts',(-2.84846973316572,6.14076830347038,89.3352488698802));
#31107=CARTESIAN_POINT('Ctrl Pts',(-3.00601088986818,6.06519723225535,89.3434614356037));
#31108=CARTESIAN_POINT('Ctrl Pts',(-3.16026132918106,5.98373105439096,89.3516740013272));
#31109=CARTESIAN_POINT('Ctrl Pts',(-3.31472342235522,5.90215309317486,89.359897835876));
#31110=CARTESIAN_POINT('Ctrl Pts',(-3.4658854636801,5.81466403877044,89.3681216704247));
#31111=CARTESIAN_POINT('Ctrl Pts',(-3.61328352052205,5.72157943231795,89.3763455049735));
#31112=CARTESIAN_POINT('Ctrl Pts',(-3.74871460788017,5.6360521890268,89.3839016619477));
#31113=CARTESIAN_POINT('Ctrl Pts',(-3.88096824980724,5.54580171474602,89.391457818922));
#31114=CARTESIAN_POINT('Ctrl Pts',(-4.00970942196484,5.4511025812588,89.3990139758962));
#31115=CARTESIAN_POINT('Ctrl Pts',(-4.15701444487575,5.34274829339431,89.4076596939486));
#31116=CARTESIAN_POINT('Ctrl Pts',(-4.30005656548543,5.22832269101837,89.4163054120009));
#31117=CARTESIAN_POINT('Ctrl Pts',(-4.43833437284333,5.1081774631308,89.4249511300533));
#31118=CARTESIAN_POINT('Ctrl Pts',(-4.57643465967659,4.98818647723112,89.4335857487656));
#31119=CARTESIAN_POINT('Ctrl Pts',(-4.70978260057282,4.86249070688326,89.442220367478));
#31120=CARTESIAN_POINT('Ctrl Pts',(-4.83790797572715,4.73148342683303,89.4508549861903));
#31121=CARTESIAN_POINT('Ctrl Pts',(-4.97055824140488,4.59584947857377,89.4597945460927));
#31122=CARTESIAN_POINT('Ctrl Pts',(-5.09761005166698,4.45452217666433,89.4687341059952));
#31123=CARTESIAN_POINT('Ctrl Pts',(-5.2185790068843,4.30798353628545,89.4776736658976));
#31124=CARTESIAN_POINT('Ctrl Pts',(-5.3350972405823,4.16683638398692,89.4862843191681));
#31125=CARTESIAN_POINT('Ctrl Pts',(-5.44597198202418,4.02085476569849,89.4948949724386));
#31126=CARTESIAN_POINT('Ctrl Pts',(-5.5508074454288,3.87050716363788,89.5035056257091));
#31127=CARTESIAN_POINT('Ctrl Pts',(-5.65554367505331,3.72030187564161,89.5121081284202));
#31128=CARTESIAN_POINT('Ctrl Pts',(-5.75425185009584,3.56573909271019,89.5207106311313));
#31129=CARTESIAN_POINT('Ctrl Pts',(-5.84657691847434,3.40731967041003,89.5293131338424));
#31130=CARTESIAN_POINT('Ctrl Pts',(-5.93879807684676,3.2490785459809,89.5379059546098));
#31131=CARTESIAN_POINT('Ctrl Pts',(-6.02465030729407,3.0869897044384,89.5464987753773));
#31132=CARTESIAN_POINT('Ctrl Pts',(-6.1038221834623,2.9215824055935,89.5550915961447));
#31133=CARTESIAN_POINT('Ctrl Pts',(-6.11315294868852,2.90208840410054,89.5561042991031));
#31134=CARTESIAN_POINT('Ctrl Pts',(-6.12239097611867,2.88254834210267,89.5571170020614));
#31135=CARTESIAN_POINT('Ctrl Pts',(-6.13153579659713,2.86296311101768,89.5581297050197));
#31136=CARTESIAN_POINT('Ctrl Pts',(-6.20694943739315,2.70145162094188,89.5664810572756));
#31137=CARTESIAN_POINT('Ctrl Pts',(-6.2759495415789,2.53701859353149,89.5748324095315));
#31138=CARTESIAN_POINT('Ctrl Pts',(-6.3383282268765,2.37020764668006,89.5831837617874));
#31139=CARTESIAN_POINT('Ctrl Pts',(-6.400741841753,2.20330329234334,89.5915397904679));
#31140=CARTESIAN_POINT('Ctrl Pts',(-6.45652652657995,2.03401868138721,89.5998958191483));
#31141=CARTESIAN_POINT('Ctrl Pts',(-6.50552402217737,1.86291336268577,89.6082518478288));
#31142=CARTESIAN_POINT('Ctrl Pts',(-6.55458494958711,1.69158653224517,89.6166186941651));
#31143=CARTESIAN_POINT('Ctrl Pts',(-6.59684103795359,1.51843461103407,89.6249855405014));
#31144=CARTESIAN_POINT('Ctrl Pts',(-6.63218470330744,1.34402941233246,89.6333523868377));
#31145=CARTESIAN_POINT('Ctrl Pts',(-6.66755368113727,1.16949930787032,89.6417252253537));
#31146=CARTESIAN_POINT('Ctrl Pts',(-6.69600030669519,0.993714469902181,
89.6500980638698));
#31147=CARTESIAN_POINT('Ctrl Pts',(-6.7174687628772,0.817252971710188,89.6584709023859));
#31148=CARTESIAN_POINT('Ctrl Pts',(-6.73896903306949,0.64052997600431,89.6668561485743));
#31149=CARTESIAN_POINT('Ctrl Pts',(-6.75347044137896,0.463128654103991,
89.6752413947628));
#31150=CARTESIAN_POINT('Ctrl Pts',(-6.76096921623424,0.285629580283465,
89.6836266409512));
#31151=CARTESIAN_POINT('Ctrl Pts',(-6.76500932685846,0.189998506171939,
89.6881443552268));
#31152=CARTESIAN_POINT('Ctrl Pts',(-6.76701766328379,0.0943390253482907,
89.6926620695022));
#31153=CARTESIAN_POINT('Ctrl Pts',(-6.76699988295537,-0.00125860319118299,
89.6971797837778));
#31154=CARTESIAN_POINT('',(-6.77442561751979,-0.00144966683613033,89.3028202190345));
#31155=CARTESIAN_POINT('Ctrl Pts',(3.10355585847744,6.02401335114973,88.6512963024177));
#31156=CARTESIAN_POINT('Ctrl Pts',(3.00479133306508,6.07541714714956,88.6565561665253));
#31157=CARTESIAN_POINT('Ctrl Pts',(0.888771830976022,7.10662707875989,88.7677504104355));
#31158=CARTESIAN_POINT('Ctrl Pts',(-4.32981959233283,6.73089174556964,88.9849250483597));
#31159=CARTESIAN_POINT('Ctrl Pts',(-6.77955107493284,2.23990816749953,89.1968398221759));
#31160=CARTESIAN_POINT('Ctrl Pts',(-6.7788200090861,-0.00145054709842048,
89.3028202161897));
#31161=CARTESIAN_POINT('Ctrl Pts',(-6.76699984504039,-0.00144817934294948,
89.3028202238418));
#31162=CARTESIAN_POINT('Ctrl Pts',(-6.76696265070365,-0.175248525353057,
89.311052552929));
#31163=CARTESIAN_POINT('Ctrl Pts',(-6.76022539825672,-0.349301770394149,
89.3192848820163));
#31164=CARTESIAN_POINT('Ctrl Pts',(-6.74675528548857,-0.523050779305459,
89.3275172111035));
#31165=CARTESIAN_POINT('Ctrl Pts',(-6.73330121635344,-0.696592843747613,
89.3357397350415));
#31166=CARTESIAN_POINT('Ctrl Pts',(-6.71313028247931,-0.869831039932917,
89.3439622589794));
#31167=CARTESIAN_POINT('Ctrl Pts',(-6.68626163023778,-1.0422065112107,89.3521847829174));
#31168=CARTESIAN_POINT('Ctrl Pts',(-6.65941959930036,-1.21441119387581,
89.3603991600265));
#31169=CARTESIAN_POINT('Ctrl Pts',(-6.62589312054883,-1.38575450239281,
89.3686135371357));
#31170=CARTESIAN_POINT('Ctrl Pts',(-6.58575325746878,-1.55568089007332,
89.3768279142448));
#31171=CARTESIAN_POINT('Ctrl Pts',(-6.54564512923008,-1.72547293282737,
89.385035797013));
#31172=CARTESIAN_POINT('Ctrl Pts',(-6.49893411291866,-1.89384993891608,
89.3932436797813));
#31173=CARTESIAN_POINT('Ctrl Pts',(-6.44574266198897,-2.06026467605874,
89.4014515625496));
#31174=CARTESIAN_POINT('Ctrl Pts',(-6.39258261907043,-2.22658115011907,
89.4096545988008));
#31175=CARTESIAN_POINT('Ctrl Pts',(-6.33294987322123,-2.39093732310856,
89.417857635052));
#31176=CARTESIAN_POINT('Ctrl Pts',(-6.26701725032542,-2.55279920560228,
89.4260606713032));
#31177=CARTESIAN_POINT('Ctrl Pts',(-6.20110411656765,-2.71461324306219,
89.4342612828047));
#31178=CARTESIAN_POINT('Ctrl Pts',(-6.12889494656976,-2.87393412585758,
89.4424618943062));
#31179=CARTESIAN_POINT('Ctrl Pts',(-6.05061150614224,-3.03024576589741,
89.4506625058077));
#31180=CARTESIAN_POINT('Ctrl Pts',(-5.97233883730244,-3.18653589788224,
89.4588619889275));
#31181=CARTESIAN_POINT('Ctrl Pts',(-5.88799372235747,-3.33981729111234,
89.4670614720472));
#31182=CARTESIAN_POINT('Ctrl Pts',(-5.79784489959881,-3.48959646953571,
89.475260955167));
#31183=CARTESIAN_POINT('Ctrl Pts',(-5.70769213553479,-3.6393821963028,89.4834607967681));
#31184=CARTESIAN_POINT('Ctrl Pts',(-5.61173534291087,-3.78566509613694,
89.4916606383692));
#31185=CARTESIAN_POINT('Ctrl Pts',(-5.51028781984356,-3.92797876044203,
89.4998604799702));
#31186=CARTESIAN_POINT('Ctrl Pts',(-5.40881746737885,-4.07032445051868,
89.5080621668351));
#31187=CARTESIAN_POINT('Ctrl Pts',(-5.30185413145434,-4.20869883427915,
89.5162638537));
#31188=CARTESIAN_POINT('Ctrl Pts',(-5.18975282496585,-4.34266676314899,
89.5244655405648));
#31189=CARTESIAN_POINT('Ctrl Pts',(-5.07754666409169,-4.47675999943338,
89.5326748989089));
#31190=CARTESIAN_POINT('Ctrl Pts',(-4.96019316133644,-4.60643827107466,
89.5408842572529));
#31191=CARTESIAN_POINT('Ctrl Pts',(-4.83808642973629,-4.73130095200058,
89.549093615597));
#31192=CARTESIAN_POINT('Ctrl Pts',(-4.71592118302453,-4.85622346872436,
89.5573069079708));
#31193=CARTESIAN_POINT('Ctrl Pts',(-4.58899842606424,-4.97632554743034,
89.5655202003446));
#31194=CARTESIAN_POINT('Ctrl Pts',(-4.45774704878049,-5.09124545166395,
89.5737334927185));
#31195=CARTESIAN_POINT('Ctrl Pts',(-4.32631686568479,-5.20632191308736,
89.5819579741895));
#31196=CARTESIAN_POINT('Ctrl Pts',(-4.19054655584925,-5.31620186561755,
89.5901824556604));
#31197=CARTESIAN_POINT('Ctrl Pts',(-4.05089677684706,-5.42056494318905,
89.5984069371314));
#31198=CARTESIAN_POINT('Ctrl Pts',(-3.92593488445409,-5.51395146884251,
89.6057663957422));
#31199=CARTESIAN_POINT('Ctrl Pts',(-3.79786722402444,-5.60292107817416,
89.6131258543529));
#31200=CARTESIAN_POINT('Ctrl Pts',(-3.66704116395306,-5.68727510341058,
89.6204853129636));
#31201=CARTESIAN_POINT('Ctrl Pts',(-3.51334538395874,-5.78637506634838,
89.6291312794545));
#31202=CARTESIAN_POINT('Ctrl Pts',(-3.35549317856629,-5.87932933795801,
89.6377772459454));
#31203=CARTESIAN_POINT('Ctrl Pts',(-3.19399180898765,-5.96579460961571,
89.6464232124363));
#31204=CARTESIAN_POINT('Ctrl Pts',(-3.03269702161607,-6.0521492804364,89.6550581195607));
#31205=CARTESIAN_POINT('Ctrl Pts',(-2.86776264543916,-6.13203135937298,
89.6636930266851));
#31206=CARTESIAN_POINT('Ctrl Pts',(-2.69972368964322,-6.20514149714406,
89.6723279338095));
#31207=CARTESIAN_POINT('Ctrl Pts',(-2.5261059761421,-6.28067883248063,89.681249512881));
#31208=CARTESIAN_POINT('Ctrl Pts',(-2.34917425510513,-6.34898665526861,
89.6901710919525));
#31209=CARTESIAN_POINT('Ctrl Pts',(-2.16954766146866,-6.40978563952149,
89.699092671024));
#31210=CARTESIAN_POINT('Ctrl Pts',(-1.99617306275606,-6.46846848421379,
89.7077037299997));
#31211=CARTESIAN_POINT('Ctrl Pts',(-1.82028833657608,-6.52015622982342,
89.7163147889754));
#31212=CARTESIAN_POINT('Ctrl Pts',(-1.64247222101487,-6.56464576372515,
89.7249258479511));
#31213=CARTESIAN_POINT('Ctrl Pts',(-1.46482379425947,-6.60909334194255,
89.7335287863006));
#31214=CARTESIAN_POINT('Ctrl Pts',(-1.28524790436,-6.64635616866093,89.7421317246502));
#31215=CARTESIAN_POINT('Ctrl Pts',(-1.10433903936368,-6.67628072253836,
89.7507346629997));
#31216=CARTESIAN_POINT('Ctrl Pts',(-0.923632750445762,-6.70617176783801,
89.7593279680485));
#31217=CARTESIAN_POINT('Ctrl Pts',(-0.741596764402537,-6.72874088365617,
89.7679212730972));
#31218=CARTESIAN_POINT('Ctrl Pts',(-0.558836585141634,-6.74388542837935,
89.776514578146));
#31219=CARTESIAN_POINT('Ctrl Pts',(-0.538474109691523,-6.74557277855254,
89.7774720129865));
#31220=CARTESIAN_POINT('Ctrl Pts',(-0.518102655000697,-6.74716801521932,
89.7784294478271));
#31221=CARTESIAN_POINT('Ctrl Pts',(-0.497723066033231,-6.74867103580686,
89.7793868826677));
#31222=CARTESIAN_POINT('Ctrl Pts',(-0.314757084158314,-6.76216500950856,
89.7879826402152));
#31223=CARTESIAN_POINT('Ctrl Pts',(-0.131349403861584,-6.76820605441165,
89.7965783977628));
#31224=CARTESIAN_POINT('Ctrl Pts',(0.0518851096250705,-6.76680108584545,
89.8051741553104));
#31225=CARTESIAN_POINT('Ctrl Pts',(0.23529058714254,-6.76539480639581,89.813777932992));
#31226=CARTESIAN_POINT('Ctrl Pts',(0.418522270053867,-6.75652864858688,
89.8223817106736));
#31227=CARTESIAN_POINT('Ctrl Pts',(0.600968566963205,-6.74026155141788,
89.8309854883552));
#31228=CARTESIAN_POINT('Ctrl Pts',(0.790585162880118,-6.72335514310549,
89.8399274020232));
#31229=CARTESIAN_POINT('Ctrl Pts',(0.979353017731205,-6.69845435117792,
89.8488693156912));
#31230=CARTESIAN_POINT('Ctrl Pts',(1.16659650727857,-6.66568388008353,89.8578112293592));
#31231=CARTESIAN_POINT('Ctrl Pts',(1.34724994785157,-6.63406676823249,89.8664384316899));
#31232=CARTESIAN_POINT('Ctrl Pts',(1.52648421520364,-6.5951245947866,89.8750656340206));
#31233=CARTESIAN_POINT('Ctrl Pts',(1.70370697552198,-6.5490206551482,89.8836928363513));
#31234=CARTESIAN_POINT('Ctrl Pts',(1.88109851339277,-6.50287280856423,89.8923282547717));
#31235=CARTESIAN_POINT('Ctrl Pts',(2.05647442793163,-6.44954966720732,89.9009636731921));
#31236=CARTESIAN_POINT('Ctrl Pts',(2.22925926219645,-6.38926381846229,89.9095990916125));
#31237=CARTESIAN_POINT('Ctrl Pts',(2.40229936144318,-6.32888890596259,89.9182472676337));
#31238=CARTESIAN_POINT('Ctrl Pts',(2.57274044573925,-6.2615308383996,89.9268954436548));
#31239=CARTESIAN_POINT('Ctrl Pts',(2.74002730451484,-6.18745015095177,89.9355436196759));
#31240=CARTESIAN_POINT('Ctrl Pts',(2.75772561987258,-6.17961269511115,89.9364585639077));
#31241=CARTESIAN_POINT('Ctrl Pts',(2.77538865371704,-6.17170003616697,89.9373735081395));
#31242=CARTESIAN_POINT('Ctrl Pts',(2.79301576541894,-6.16371251228683,89.9382884523713));
#31243=CARTESIAN_POINT('Ctrl Pts',(2.95149590480565,-6.09189905133607,89.9465144449126));
#31244=CARTESIAN_POINT('Ctrl Pts',(3.1074125902076,-6.01387519699057,89.954740437454));
#31245=CARTESIAN_POINT('Ctrl Pts',(3.26024624044715,-5.92984683205648,89.9629664299953));
#31246=CARTESIAN_POINT('Ctrl Pts',(3.41291966435877,-5.84590656000202,89.9711837986467));
#31247=CARTESIAN_POINT('Ctrl Pts',(3.56251617815635,-5.75597448414214,89.9794011672981));
#31248=CARTESIAN_POINT('Ctrl Pts',(3.70853670240629,-5.66030427865018,89.9876185359495));
#31249=CARTESIAN_POINT('Ctrl Pts',(3.85443336108473,-5.56471522780917,89.9958289340119));
#31250=CARTESIAN_POINT('Ctrl Pts',(3.99675977367483,-5.4633979368922,90.0040393320743));
#31251=CARTESIAN_POINT('Ctrl Pts',(4.13504190170056,-5.35665170336664,90.0122497301367));
#31252=CARTESIAN_POINT('Ctrl Pts',(4.27323439030631,-5.24997466656659,90.0204548059255));
#31253=CARTESIAN_POINT('Ctrl Pts',(4.40738753388358,-5.13787591537142,90.0286598817142));
#31254=CARTESIAN_POINT('Ctrl Pts',(4.53705663900844,-5.02069776569248,90.036864957503));
#31255=CARTESIAN_POINT('Ctrl Pts',(4.66666762163094,-4.90357213960638,90.0450663554725));
#31256=CARTESIAN_POINT('Ctrl Pts',(4.7917983048632,-4.78137189075798,90.0532677534419));
#31257=CARTESIAN_POINT('Ctrl Pts',(4.91203736727252,-4.65447933742524,90.0614691514114));
#31258=CARTESIAN_POINT('Ctrl Pts',(5.03226701155738,-4.52759672337376,90.0696699069791));
#31259=CARTESIAN_POINT('Ctrl Pts',(5.14760554564225,-4.39602279080391,90.0778706625469));
#31260=CARTESIAN_POINT('Ctrl Pts',(5.25767854304365,-4.26017667920222,90.0860714181146));
#31261=CARTESIAN_POINT('Ctrl Pts',(5.36775098132661,-4.12433125763411,90.0942721320263));
#31262=CARTESIAN_POINT('Ctrl Pts',(5.47255770975845,-3.98421397802927,90.1024728459381));
#31263=CARTESIAN_POINT('Ctrl Pts',(5.57176472796013,-3.84027691921551,90.1106735598499));
#31264=CARTESIAN_POINT('Ctrl Pts',(5.67098922101932,-3.69631450655443,90.1188757182795));
#31265=CARTESIAN_POINT('Ctrl Pts',(5.76461183530915,-3.54853126925179,90.1270778767091));
#31266=CARTESIAN_POINT('Ctrl Pts',(5.85234200095878,-3.39740814501494,90.1352800351387));
#31267=CARTESIAN_POINT('Ctrl Pts',(5.94010351892995,-3.24623101357602,90.1434851247916));
#31268=CARTESIAN_POINT('Ctrl Pts',(6.02196821358159,-3.09171192725364,90.1516902144446));
#31269=CARTESIAN_POINT('Ctrl Pts',(6.0976915279016,-2.93435632303868,90.1598953040975));
#31270=CARTESIAN_POINT('Ctrl Pts',(6.17350134715538,-2.7768209586502,90.1681097670953));
#31271=CARTESIAN_POINT('Ctrl Pts',(6.24315561418344,-2.6164429259011,90.1763242300931));
#31272=CARTESIAN_POINT('Ctrl Pts',(6.30645757824187,-2.45374852294113,90.1845386930908));
#31273=CARTESIAN_POINT('Ctrl Pts',(6.36979704671332,-2.29095772868938,90.1927580228983));
#31274=CARTESIAN_POINT('Ctrl Pts',(6.42677659332348,-2.12584816675173,90.2009773527058));
#31275=CARTESIAN_POINT('Ctrl Pts',(6.47724945315914,-1.95896108219372,90.2091966825133));
#31276=CARTESIAN_POINT('Ctrl Pts',(6.527800517631,-1.79181541621639,90.217428747674));
#31277=CARTESIAN_POINT('Ctrl Pts',(6.57182465781303,-1.62288707027252,90.2256608128347));
#31278=CARTESIAN_POINT('Ctrl Pts',(6.60922602780241,-1.45272857527453,90.2338928779953));
#31279=CARTESIAN_POINT('Ctrl Pts',(6.64284506471496,-1.29977790191831,90.2412924492566));
#31280=CARTESIAN_POINT('Ctrl Pts',(6.6711137667923,-1.14583359882521,90.2486920205178));
#31281=CARTESIAN_POINT('Ctrl Pts',(6.69399839447839,-0.991299397115065,
90.256091591779));
#31282=CARTESIAN_POINT('Ctrl Pts',(6.7192207516475,-0.820979089359053,90.2642470501858));
#31283=CARTESIAN_POINT('Ctrl Pts',(6.73797962917,-0.649417720235256,90.2724025085926));
#31284=CARTESIAN_POINT('Ctrl Pts',(6.75015668295053,-0.477151711322865,
90.2805579669994));
#31285=CARTESIAN_POINT('Ctrl Pts',(6.76231891565596,-0.305095372787335,
90.2887034991413));
#31286=CARTESIAN_POINT('Ctrl Pts',(6.76791524528198,-0.132336462220329,
90.2968490312831));
#31287=CARTESIAN_POINT('Ctrl Pts',(6.7668783330469,0.0405786365024204,90.304994563425));
#31288=CARTESIAN_POINT('Ctrl Pts',(6.76584246482847,0.213319635397034,90.3131318942256));
#31289=CARTESIAN_POINT('Ctrl Pts',(6.75818665301157,0.386216146611542,90.3212692250261));
#31290=CARTESIAN_POINT('Ctrl Pts',(6.74389534570866,0.558716892646988,90.3294065558267));
#31291=CARTESIAN_POINT('Ctrl Pts',(6.7296154242676,0.731080207611699,90.3375374036287));
#31292=CARTESIAN_POINT('Ctrl Pts',(6.70871056343421,0.903048022650518,90.3456682514307));
#31293=CARTESIAN_POINT('Ctrl Pts',(6.68121726641431,1.07406928964906,90.3537990992328));
#31294=CARTESIAN_POINT('Ctrl Pts',(6.65374009781757,1.24499023025313,90.3619251772266));
#31295=CARTESIAN_POINT('Ctrl Pts',(6.61968224793648,1.41496536867099,90.3700512552204));
#31296=CARTESIAN_POINT('Ctrl Pts',(6.57913202703983,1.58344901110798,90.3781773332142));
#31297=CARTESIAN_POINT('Ctrl Pts',(6.53843802246611,1.75253006576861,90.3863322247964));
#31298=CARTESIAN_POINT('Ctrl Pts',(6.4912055576777,1.9201086578375,90.3944871163785));
#31299=CARTESIAN_POINT('Ctrl Pts',(6.43757573536627,2.08564322246723,90.4026420079607));
#31300=CARTESIAN_POINT('Ctrl Pts',(6.38415505061073,2.25053226017239,90.410765098317));
#31301=CARTESIAN_POINT('Ctrl Pts',(6.3243869434986,2.41339283868552,90.4188881886733));
#31302=CARTESIAN_POINT('Ctrl Pts',(6.25846084365304,2.57370489148652,90.4270112790296));
#31303=CARTESIAN_POINT('Ctrl Pts',(6.19252956698909,2.73402953272194,90.435135007248));
#31304=CARTESIAN_POINT('Ctrl Pts',(6.12043947350541,2.89180491126887,90.4432587354665));
#31305=CARTESIAN_POINT('Ctrl Pts',(6.04242806073999,3.04653116359935,90.4513824636849));
#31306=CARTESIAN_POINT('Ctrl Pts',(5.96439568058366,3.20129900222728,90.4595083753453));
#31307=CARTESIAN_POINT('Ctrl Pts',(5.88043897681269,3.35301575629469,90.4676342870056));
#31308=CARTESIAN_POINT('Ctrl Pts',(5.79084126922772,3.50120641988003,90.4757601986659));
#31309=CARTESIAN_POINT('Ctrl Pts',(5.70067057498911,3.65034477816333,90.4839380763759));
#31310=CARTESIAN_POINT('Ctrl Pts',(5.60478667122776,3.79591146857661,90.492115954086));
#31311=CARTESIAN_POINT('Ctrl Pts',(5.50352196063604,3.93745286051742,90.5002938317961));
#31312=CARTESIAN_POINT('Ctrl Pts',(5.40274056454492,4.07831870609307,90.5084326782695));
#31313=CARTESIAN_POINT('Ctrl Pts',(5.29662988469172,4.21519734130055,90.516571524743));
#31314=CARTESIAN_POINT('Ctrl Pts',(5.18555709224255,4.34767600484362,90.5247103712164));
#31315=CARTESIAN_POINT('Ctrl Pts',(5.07368529680328,4.48110765467579,90.5329077645448));
#31316=CARTESIAN_POINT('Ctrl Pts',(4.95677998332856,4.61007551183414,90.5411051578731));
#31317=CARTESIAN_POINT('Ctrl Pts',(4.83525264498751,4.73419696032403,90.5493025512015));
#31318=CARTESIAN_POINT('Ctrl Pts',(4.71372530664655,4.85831840881383,90.5574999445299));
#31319=CARTESIAN_POINT('Ctrl Pts',(4.58757625589913,4.97759323730456,90.5656973378583));
#31320=CARTESIAN_POINT('Ctrl Pts',(4.45724896156953,5.09168151935953,90.5738947311867));
#31321=CARTESIAN_POINT('Ctrl Pts',(4.32646157626755,5.20617256423481,90.5821210635542));
#31322=CARTESIAN_POINT('Ctrl Pts',(4.19107721989538,5.31578121746848,90.5903473959217));
#31323=CARTESIAN_POINT('Ctrl Pts',(4.05149525096489,5.42011763999721,90.5985737282891));
#31324=CARTESIAN_POINT('Ctrl Pts',(3.91205160760407,5.52435066525198,90.6067919083708));
#31325=CARTESIAN_POINT('Ctrl Pts',(3.76841891532853,5.62332164540642,90.6150100884524));
#31326=CARTESIAN_POINT('Ctrl Pts',(3.62103201932383,5.71667876612212,90.623228268534));
#31327=CARTESIAN_POINT('Ctrl Pts',(3.47379502011576,5.80994093990756,90.6314380904854));
#31328=CARTESIAN_POINT('Ctrl Pts',(3.32281172514781,5.89760043816214,90.6396479124369));
#31329=CARTESIAN_POINT('Ctrl Pts',(3.16854834407815,5.97934698702456,90.6478577343883));
#31330=CARTESIAN_POINT('Ctrl Pts',(3.14549679572227,5.99156235862449,90.6490845265563));
#31331=CARTESIAN_POINT('Ctrl Pts',(3.12237206044821,6.00364577566048,90.6503113187243));
#31332=CARTESIAN_POINT('Ctrl Pts',(3.09917575053247,6.01559628526645,90.6515381108923));
#31333=CARTESIAN_POINT('Origin',(0.,0.,-3.69717978381041));
#31334=CARTESIAN_POINT('',(3.09917575053244,6.01559628526647,93.0458095097322));
#31335=CARTESIAN_POINT('',(3.09917575053273,6.01559628526632,92.651392015122));
#31336=CARTESIAN_POINT('',(3.09917575053259,6.01559628526639,-3.69717978381041));
#31337=CARTESIAN_POINT('',(-6.76699860320916,0.00434789205820069,91.6971797838561));
#31338=CARTESIAN_POINT('Ctrl Pts',(-6.76699860320916,0.00434789205818717,
91.6971797838561));
#31339=CARTESIAN_POINT('Ctrl Pts',(-6.76710755774317,-0.165227426188215,
91.705162465091));
#31340=CARTESIAN_POINT('Ctrl Pts',(-6.76083819870497,-0.335012369902362,
91.713145146326));
#31341=CARTESIAN_POINT('Ctrl Pts',(-6.74816981568796,-0.504473129748143,
91.7211278275609));
#31342=CARTESIAN_POINT('Ctrl Pts',(-6.73550943926403,-0.673826788052786,
91.729105463631));
#31343=CARTESIAN_POINT('Ctrl Pts',(-6.71645811032625,-0.842856292913908,
91.7370830997012));
#31344=CARTESIAN_POINT('Ctrl Pts',(-6.69104717862425,-1.01102752357418,
91.7450607357713));
#31345=CARTESIAN_POINT('Ctrl Pts',(-6.66564677156446,-1.17912910145453,
91.7530350676821));
#31346=CARTESIAN_POINT('Ctrl Pts',(-6.63389205724408,-1.34637273726657,
91.7610093995929));
#31347=CARTESIAN_POINT('Ctrl Pts',(-6.5958662380544,-1.51222933766481,91.7689837315038));
#31348=CARTESIAN_POINT('Ctrl Pts',(-6.56921624055413,-1.62846820063229,
91.774572458585));
#31349=CARTESIAN_POINT('Ctrl Pts',(-6.53948711408368,-1.74402586995437,
91.7801611856661));
#31350=CARTESIAN_POINT('Ctrl Pts',(-6.50672250975899,-1.85872299738174,
91.7857499127473));
#31351=CARTESIAN_POINT('Ctrl Pts',(-6.45633174716039,-2.03512298261142,
91.7943451705074));
#31352=CARTESIAN_POINT('Ctrl Pts',(-6.39879310470646,-2.2093686632292,91.8029404282674));
#31353=CARTESIAN_POINT('Ctrl Pts',(-6.33432507402493,-2.3808853094131,91.8115356860274));
#31354=CARTESIAN_POINT('Ctrl Pts',(-6.26979667176679,-2.55256257366203,
91.8201389928819));
#31355=CARTESIAN_POINT('Ctrl Pts',(-6.19832603626417,-2.72150541652671,
91.8287422997363));
#31356=CARTESIAN_POINT('Ctrl Pts',(-6.12017936261071,-2.88716012189728,
91.8373456065907));
#31357=CARTESIAN_POINT('Ctrl Pts',(-6.0387927007682,-3.05968292879758,91.8463056095307));
#31358=CARTESIAN_POINT('Ctrl Pts',(-5.95016479774376,-3.22863879470019,
91.8552656124707));
#31359=CARTESIAN_POINT('Ctrl Pts',(-5.85464789181539,-3.3934329318349,91.8642256154107));
#31360=CARTESIAN_POINT('Ctrl Pts',(-5.76268259042405,-3.55209952956248,
91.8728524586155));
#31361=CARTESIAN_POINT('Ctrl Pts',(-5.66433155353296,-3.70690808393633,
91.8814793018202));
#31362=CARTESIAN_POINT('Ctrl Pts',(-5.55995238299365,-3.85735900569849,
91.8901061450249));
#31363=CARTESIAN_POINT('Ctrl Pts',(-5.45547345235264,-4.00795372051034,
91.898741233311));
#31364=CARTESIAN_POINT('Ctrl Pts',(-5.34495506920274,-4.15418224439382,
91.9073763215971));
#31365=CARTESIAN_POINT('Ctrl Pts',(-5.22879527599012,-4.29557783793792,
91.9160114098832));
#31366=CARTESIAN_POINT('Ctrl Pts',(-5.11246296217296,-4.43718343231452,
91.9246593230084));
#31367=CARTESIAN_POINT('Ctrl Pts',(-4.99047269463205,-4.57394152202166,
91.9333072361335));
#31368=CARTESIAN_POINT('Ctrl Pts',(-4.86326053704181,-4.70542091091242,
91.9419551492587));
#31369=CARTESIAN_POINT('Ctrl Pts',(-4.8489892695319,-4.72017089681348,91.9429253134627));
#31370=CARTESIAN_POINT('Ctrl Pts',(-4.83465231767785,-4.73485448880977,
91.9438954776668));
#31371=CARTESIAN_POINT('Ctrl Pts',(-4.82025032355627,-4.74947110931898,
91.9448656418708));
#31372=CARTESIAN_POINT('Ctrl Pts',(-4.69815574864879,-4.87338520431105,
91.9530903213896));
#31373=CARTESIAN_POINT('Ctrl Pts',(-4.57111901890713,-4.99275154831081,
91.9613150009084));
#31374=CARTESIAN_POINT('Ctrl Pts',(-4.43951248728886,-5.10715359816075,
91.9695396804272));
#31375=CARTESIAN_POINT('Ctrl Pts',(-4.30804428902431,-5.2214353985137,91.9777557148773));
#31376=CARTESIAN_POINT('Ctrl Pts',(-4.17201612238669,-5.33076306246661,
91.9859717493275));
#31377=CARTESIAN_POINT('Ctrl Pts',(-4.0318381286734,-5.43475577226571,91.9941877837776));
#31378=CARTESIAN_POINT('Ctrl Pts',(-3.89177939999142,-5.53866000388458,
92.0023968279322));
#31379=CARTESIAN_POINT('Ctrl Pts',(-3.74757816231607,-5.63723810903598,
92.0106058720868));
#31380=CARTESIAN_POINT('Ctrl Pts',(-3.59967874351923,-5.73014850972083,
92.0188149162414));
#31381=CARTESIAN_POINT('Ctrl Pts',(-3.45187554308325,-5.82299846604062,
92.0270186198694));
#31382=CARTESIAN_POINT('Ctrl Pts',(-3.3003792563041,-5.91018787252385,92.0352223234975));
#31383=CARTESIAN_POINT('Ctrl Pts',(-3.14566446671059,-5.99141753367885,
92.0434260271255));
#31384=CARTESIAN_POINT('Ctrl Pts',(-2.99101935473563,-6.07261061210405,
92.0516260361195));
#31385=CARTESIAN_POINT('Ctrl Pts',(-2.83315894441096,-6.14784912628321,
92.0598260451135));
#31386=CARTESIAN_POINT('Ctrl Pts',(-2.67258385337681,-6.21687900370191,
92.0680260541075));
#31387=CARTESIAN_POINT('Ctrl Pts',(-2.51202160226596,-6.28590336134585,
92.0762254074114));
#31388=CARTESIAN_POINT('Ctrl Pts',(-2.34874542839318,-6.34871992161912,
92.0844247607154));
#31389=CARTESIAN_POINT('Ctrl Pts',(-2.18327778105369,-6.40512194503409,
92.0926241140193));
#31390=CARTESIAN_POINT('Ctrl Pts',(-2.01781121251409,-6.46152360072463,
92.1008234138659));
#31391=CARTESIAN_POINT('Ctrl Pts',(-1.85015353795974,-6.51151068615962,
92.1090227137125));
#31392=CARTESIAN_POINT('Ctrl Pts',(-1.68084417487681,-6.55492577073018,
92.1172220135591));
#31393=CARTESIAN_POINT('Ctrl Pts',(-1.51150520126126,-6.59834844816954,
92.1254227473822));
#31394=CARTESIAN_POINT('Ctrl Pts',(-1.34051431089039,-6.63519674574834,
92.1336234812052));
#31395=CARTESIAN_POINT('Ctrl Pts',(-1.1684230211126,-6.66536395433394,92.1418242150282));
#31396=CARTESIAN_POINT('Ctrl Pts',(-0.996270414882502,-6.69554191155306,
92.1500278707882));
#31397=CARTESIAN_POINT('Ctrl Pts',(-0.823016981123086,-6.71903397586791,
92.1582315265482));
#31398=CARTESIAN_POINT('Ctrl Pts',(-0.649221352251423,-6.73578507939356,
92.1664351823083));
#31399=CARTESIAN_POINT('Ctrl Pts',(-0.475226629315058,-6.75255537238508,
92.1746482358833));
#31400=CARTESIAN_POINT('Ctrl Pts',(-0.300688827600502,-6.76256924240023,
92.1828612894583));
#31401=CARTESIAN_POINT('Ctrl Pts',(-0.126169665710542,-6.76582369083429,
92.1910743430333));
#31402=CARTESIAN_POINT('Ctrl Pts',(0.0484527630829802,-6.7690800649985,
92.1992922564564));
#31403=CARTESIAN_POINT('Ctrl Pts',(0.223056172214694,-6.76556905187751,
92.2075101698795));
#31404=CARTESIAN_POINT('Ctrl Pts',(0.397082068574533,-6.75533972726884,
92.2157280833026));
#31405=CARTESIAN_POINT('Ctrl Pts',(0.571379386630653,-6.74509444836431,
92.2239588138986));
#31406=CARTESIAN_POINT('Ctrl Pts',(0.745097035285941,-6.72810995271888,
92.2321895444946));
#31407=CARTESIAN_POINT('Ctrl Pts',(0.917683489713388,-6.70448700593173,
92.2404202750906));
#31408=CARTESIAN_POINT('Ctrl Pts',(1.07618350715472,-6.68279215455884,92.2479792167663));
#31409=CARTESIAN_POINT('Ctrl Pts',(1.23372935843241,-6.65549892256677,92.2555381584418));
#31410=CARTESIAN_POINT('Ctrl Pts',(1.38990473063026,-6.62272253984505,92.2630971001175));
#31411=CARTESIAN_POINT('Ctrl Pts',(1.55837238108287,-6.58736638791305,92.2712509922842));
#31412=CARTESIAN_POINT('Ctrl Pts',(1.72576603746152,-6.54551994726072,92.2794048844509));
#31413=CARTESIAN_POINT('Ctrl Pts',(1.8915416762854,-6.49725781286809,92.2875587766177));
#31414=CARTESIAN_POINT('Ctrl Pts',(2.05711502251477,-6.44905457176311,92.2957027187579));
#31415=CARTESIAN_POINT('Ctrl Pts',(2.22107393415481,-6.39445132170594,92.3038466608981));
#31416=CARTESIAN_POINT('Ctrl Pts',(2.38288268948448,-6.33357395852888,92.3119906030383));
#31417=CARTESIAN_POINT('Ctrl Pts',(2.54452805044158,-6.27275806927232,92.3201263214312));
#31418=CARTESIAN_POINT('Ctrl Pts',(2.70402723791533,-6.20568080760949,92.3282620398241));
#31419=CARTESIAN_POINT('Ctrl Pts',(2.86085785998917,-6.13251834933563,92.336397758217));
#31420=CARTESIAN_POINT('Ctrl Pts',(3.0175631039645,-6.05941438072265,92.3445269725172));
#31421=CARTESIAN_POINT('Ctrl Pts',(3.17160370050919,-5.98023505569614,92.3526561868174));
#31422=CARTESIAN_POINT('Ctrl Pts',(3.32247548881616,-5.89520530823277,92.3607854011176));
#31423=CARTESIAN_POINT('Ctrl Pts',(3.47325838547474,-5.81022565916419,92.368909825793));
#31424=CARTESIAN_POINT('Ctrl Pts',(3.62087587424615,-5.71940263127901,92.3770342504684));
#31425=CARTESIAN_POINT('Ctrl Pts',(3.76484674977185,-5.62300790953848,92.3851586751439));
#31426=CARTESIAN_POINT('Ctrl Pts',(3.90969162067757,-5.52602801012816,92.393332420278));
#31427=CARTESIAN_POINT('Ctrl Pts',(4.0508451187565,-5.42340870668908,92.4015061654122));
#31428=CARTESIAN_POINT('Ctrl Pts',(4.18784475117516,-5.31547225936272,92.4096799105464));
#31429=CARTESIAN_POINT('Ctrl Pts',(4.32396707803633,-5.20822700546093,92.4178013134085));
#31430=CARTESIAN_POINT('Ctrl Pts',(4.45598830744837,-5.09573275470312,92.4259227162707));
#31431=CARTESIAN_POINT('Ctrl Pts',(4.58348636821586,-4.97834728724095,92.4340441191328));
#31432=CARTESIAN_POINT('Ctrl Pts',(4.71099428646251,-4.86095274415214,92.4421661498991));
#31433=CARTESIAN_POINT('Ctrl Pts',(4.83397807019475,-4.73866647895501,92.4502881806654));
#31434=CARTESIAN_POINT('Ctrl Pts',(4.9520512544675,-4.61188436250595,92.4584102114316));
#31435=CARTESIAN_POINT('Ctrl Pts',(5.07015605139785,-4.48506830168872,92.4665344167727));
#31436=CARTESIAN_POINT('Ctrl Pts',(5.18334738163508,-4.35375426053406,92.4746586221139));
#31437=CARTESIAN_POINT('Ctrl Pts',(5.29127797625718,-4.21837247975754,92.482782827455));
#31438=CARTESIAN_POINT('Ctrl Pts',(5.40037684488427,-4.08152528488055,92.4909949716974));
#31439=CARTESIAN_POINT('Ctrl Pts',(5.5041001850742,-3.94052207444959,92.4992071159399));
#31440=CARTESIAN_POINT('Ctrl Pts',(5.60213377838816,-3.79583800089551,92.5074192601824));
#31441=CARTESIAN_POINT('Ctrl Pts',(5.69927243304204,-3.65247473347069,92.5155564365988));
#31442=CARTESIAN_POINT('Ctrl Pts',(5.79082465098,-3.50549787138021,92.5236936130153));
#31443=CARTESIAN_POINT('Ctrl Pts',(5.87653081531274,-3.35539484661341,92.5318307894317));
#31444=CARTESIAN_POINT('Ctrl Pts',(5.96342139629414,-3.20321747255176,92.5400804175872));
#31445=CARTESIAN_POINT('Ctrl Pts',(6.04430298011276,-3.04782724715359,92.5483300457426));
#31446=CARTESIAN_POINT('Ctrl Pts',(6.11895548514497,-2.88975306398562,92.5565796738981));
#31447=CARTESIAN_POINT('Ctrl Pts',(6.19360799017718,-2.73167888081765,92.5648293020535));
#31448=CARTESIAN_POINT('Ctrl Pts',(6.2620313239398,-2.57092111869645,92.573078930209));
#31449=CARTESIAN_POINT('Ctrl Pts',(6.32405790722228,-2.40802420795542,92.5813285583644));
#31450=CARTESIAN_POINT('Ctrl Pts',(6.38589832358761,-2.24561621686919,92.589553426042));
#31451=CARTESIAN_POINT('Ctrl Pts',(6.44156534305441,-2.08059650627191,92.5977782937196));
#31452=CARTESIAN_POINT('Ctrl Pts',(6.49083224066949,-1.9134748034624,92.6060031613972));
#31453=CARTESIAN_POINT('Ctrl Pts',(6.54004363360991,-1.74654138195722,92.6142187628407));
#31454=CARTESIAN_POINT('Ctrl Pts',(6.58286916202593,-1.57751102478036,92.6224343642843));
#31455=CARTESIAN_POINT('Ctrl Pts',(6.61913014855371,-1.4069133152072,92.6306499657278));
#31456=CARTESIAN_POINT('Ctrl Pts',(6.65535756858123,-1.23647352654609,92.6388579620559));
#31457=CARTESIAN_POINT('Ctrl Pts',(6.68503247455617,-1.06446962367575,92.6470659583841));
#31458=CARTESIAN_POINT('Ctrl Pts',(6.70802597368386,-0.891446317162547,
92.6552739547122));
#31459=CARTESIAN_POINT('Ctrl Pts',(6.73100280628052,-0.718548424284471,
92.6634760015837));
#31460=CARTESIAN_POINT('Ctrl Pts',(6.74730783115768,-0.54463295371733,92.6716780484551));
#31461=CARTESIAN_POINT('Ctrl Pts',(6.75686320228404,-0.370254865761249,
92.6798800953266));
#31462=CARTESIAN_POINT('Ctrl Pts',(6.76641356613106,-0.195968156757047,
92.6880778440982));
#31463=CARTESIAN_POINT('Ctrl Pts',(6.76922130292415,-0.0212196706970898,
92.6962755928698));
#31464=CARTESIAN_POINT('Ctrl Pts',(6.76526038851042,0.153430360919473,92.7044733416414));
#31465=CARTESIAN_POINT('Ctrl Pts',(6.76130022956156,0.328047081550108,92.712669526857));
#31466=CARTESIAN_POINT('Ctrl Pts',(6.75057399279243,0.502565026684469,92.7208657120726));
#31467=CARTESIAN_POINT('Ctrl Pts',(6.7331077703053,0.676423501553901,92.7290618972882));
#31468=CARTESIAN_POINT('Ctrl Pts',(6.71564283992992,0.850269114765363,92.7372574761686));
#31469=CARTESIAN_POINT('Ctrl Pts',(6.69143895180731,1.02345499775442,92.7454530550489));
#31470=CARTESIAN_POINT('Ctrl Pts',(6.66057412388875,1.19542517130248,92.7536486339292));
#31471=CARTESIAN_POINT('Ctrl Pts',(6.62970596379054,1.36741391082199,92.7618450976076));
#31472=CARTESIAN_POINT('Ctrl Pts',(6.59217549459628,1.53818632615473,92.7700415612861));
#31473=CARTESIAN_POINT('Ctrl Pts',(6.54811195748699,1.70719617859692,92.7782380249646));
#31474=CARTESIAN_POINT('Ctrl Pts',(6.50403564638775,1.87625502688235,92.7864368647923));
#31475=CARTESIAN_POINT('Ctrl Pts',(6.45342258540803,2.04354994736245,92.7946357046201));
#31476=CARTESIAN_POINT('Ctrl Pts',(6.39645203796197,2.20854937143187,92.8028345444479));
#31477=CARTESIAN_POINT('Ctrl Pts',(6.33942198315822,2.37372114209419,92.8110419481971));
#31478=CARTESIAN_POINT('Ctrl Pts',(6.27602129215305,2.53659228639573,92.8192493519463));
#31479=CARTESIAN_POINT('Ctrl Pts',(6.20647796789813,2.69664981671614,92.8274567556956));
#31480=CARTESIAN_POINT('Ctrl Pts',(6.13689739255857,2.85679308231987,92.8356685557646));
#31481=CARTESIAN_POINT('Ctrl Pts',(6.06116778011801,3.01411940644195,92.8438803558336));
#31482=CARTESIAN_POINT('Ctrl Pts',(5.97956331682157,3.16814007583657,92.8520921559027));
#31483=CARTESIAN_POINT('Ctrl Pts',(5.89783872035261,3.32238748517779,92.8603160448888));
#31484=CARTESIAN_POINT('Ctrl Pts',(5.81022216919037,3.47331920411975,92.868539933875));
#31485=CARTESIAN_POINT('Ctrl Pts',(5.71703212125234,3.62047410218178,92.8767638228611));
#31486=CARTESIAN_POINT('Ctrl Pts',(5.63092612801164,3.75644268400171,92.8843625541111));
#31487=CARTESIAN_POINT('Ctrl Pts',(5.54006239522148,3.88918697978357,92.8919612853611));
#31488=CARTESIAN_POINT('Ctrl Pts',(5.44472225972871,4.01836888729926,92.8995600166111));
#31489=CARTESIAN_POINT('Ctrl Pts',(5.34152069359962,4.15820270547307,92.9077853139797));
#31490=CARTESIAN_POINT('Ctrl Pts',(5.23278390163382,4.29425453053385,92.9160106113483));
#31491=CARTESIAN_POINT('Ctrl Pts',(5.11881819253714,4.42605798784323,92.9242359087169));
#31492=CARTESIAN_POINT('Ctrl Pts',(5.00497706538544,4.5577173638215,92.9324522145779));
#31493=CARTESIAN_POINT('Ctrl Pts',(4.88591863435858,4.68513734956562,92.9406685204389));
#31494=CARTESIAN_POINT('Ctrl Pts',(4.76199193154249,4.80788122190266,92.9488848262999));
#31495=CARTESIAN_POINT('Ctrl Pts',(4.63820337581851,4.93048826570596,92.9570919730471));
#31496=CARTESIAN_POINT('Ctrl Pts',(4.50955761656096,5.04842933320243,92.9652991197944));
#31497=CARTESIAN_POINT('Ctrl Pts',(4.3764431142717,5.16130164469621,92.9735062665417));
#31498=CARTESIAN_POINT('Ctrl Pts',(4.24341509065272,5.27410062798577,92.9817080814646));
#31499=CARTESIAN_POINT('Ctrl Pts',(4.10592437625008,5.38183718013761,92.9899098963876));
#31500=CARTESIAN_POINT('Ctrl Pts',(3.96439573176304,5.48414582975134,92.9981117113106));
#31501=CARTESIAN_POINT('Ctrl Pts',(3.82293398255666,5.58640612190461,93.0063096495433));
#31502=CARTESIAN_POINT('Ctrl Pts',(3.6774383938496,5.68324341060657,93.0145075877761));
#31503=CARTESIAN_POINT('Ctrl Pts',(3.52836624268282,5.77433291883108,93.0227055260089));
#31504=CARTESIAN_POINT('Ctrl Pts',(3.38832450469249,5.85990445546354,93.0304068539166));
#31505=CARTESIAN_POINT('Ctrl Pts',(3.24512688595244,5.94040370281804,93.0381081818244));
#31506=CARTESIAN_POINT('Ctrl Pts',(3.09917575053244,6.01559628526647,93.0458095097322));
#31507=CARTESIAN_POINT('Ctrl Pts',(3.09917575053275,6.01559628526631,91.0459618091817));
#31508=CARTESIAN_POINT('Ctrl Pts',(2.94553883644237,6.0947485049227,91.0540936986117));
#31509=CARTESIAN_POINT('Ctrl Pts',(2.78871399936926,6.16809025739574,91.0622255880417));
#31510=CARTESIAN_POINT('Ctrl Pts',(2.62918527808529,6.23535674789338,91.0703574774717));
#31511=CARTESIAN_POINT('Ctrl Pts',(2.46976524118543,6.30257741079941,91.0784838267746));
#31512=CARTESIAN_POINT('Ctrl Pts',(2.30764532394961,6.3637309118955,91.0866101760775));
#31513=CARTESIAN_POINT('Ctrl Pts',(2.14333295264033,6.4185989790706,91.0947365253803));
#31514=CARTESIAN_POINT('Ctrl Pts',(1.9790979820844,6.47344120017153,91.1028590466966));
#31515=CARTESIAN_POINT('Ctrl Pts',(1.81267296063862,6.52200376861243,91.1109815680128));
#31516=CARTESIAN_POINT('Ctrl Pts',(1.64458401674675,6.56411703215757,91.1191040893291));
#31517=CARTESIAN_POINT('Ctrl Pts',(1.47651046575417,6.60622643914196,91.127225866818));
#31518=CARTESIAN_POINT('Ctrl Pts',(1.30677364815761,6.64188761962794,91.135347644307));
#31519=CARTESIAN_POINT('Ctrl Pts',(1.1359137972616,6.6709811006471,91.1434694217959));
#31520=CARTESIAN_POINT('Ctrl Pts',(0.965054922794803,6.70007441540294,91.1515911528705));
#31521=CARTESIAN_POINT('Ctrl Pts',(0.793073388439417,6.72260004293741,91.1597128839451));
#31522=CARTESIAN_POINT('Ctrl Pts',(0.620518326237572,6.7384898906805,91.1678346150197));
#31523=CARTESIAN_POINT('Ctrl Pts',(0.447931392235734,6.75438267335951,91.1759578462195));
#31524=CARTESIAN_POINT('Ctrl Pts',(0.274771083864169,6.76363720173535,91.1840810774192));
#31525=CARTESIAN_POINT('Ctrl Pts',(0.10159029898932,6.76623738950617,91.192204308619));
#31526=CARTESIAN_POINT('Ctrl Pts',(-0.0716554527820409,6.76883855270928,
91.200330587161));
#31527=CARTESIAN_POINT('Ctrl Pts',(-0.244921330711114,6.76478039895497,
91.208456865703));
#31528=CARTESIAN_POINT('Ctrl Pts',(-0.417655840659719,6.7540989479547,91.216583144245));
#31529=CARTESIAN_POINT('Ctrl Pts',(-0.590591764695115,6.7434050420333,91.2247188982935));
#31530=CARTESIAN_POINT('Ctrl Pts',(-0.76299471772106,6.72607243599861,91.232854652342));
#31531=CARTESIAN_POINT('Ctrl Pts',(-0.934318782378692,6.70218900157959,
91.2409904063905));
#31532=CARTESIAN_POINT('Ctrl Pts',(-1.10574976822514,6.67829066181026,91.2491312378605));
#31533=CARTESIAN_POINT('Ctrl Pts',(-1.27610016491944,6.64783341229592,91.2572720693306));
#31534=CARTESIAN_POINT('Ctrl Pts',(-1.44483593130785,6.61095591662823,91.2654129008006));
#31535=CARTESIAN_POINT('Ctrl Pts',(-1.61383281245392,6.57402135387541,91.273566330022));
#31536=CARTESIAN_POINT('Ctrl Pts',(-1.78120971858682,6.5306467894196,91.2817197592434));
#31537=CARTESIAN_POINT('Ctrl Pts',(-1.94644830628421,6.48102059794315,91.2898731884649));
#31538=CARTESIAN_POINT('Ctrl Pts',(-2.07162240693606,6.44342699481808,91.2960497007689));
#31539=CARTESIAN_POINT('Ctrl Pts',(-2.19556975145639,6.40224685692166,91.302226213073));
#31540=CARTESIAN_POINT('Ctrl Pts',(-2.31807371444179,6.35757998411456,91.3084027253771));
#31541=CARTESIAN_POINT('Ctrl Pts',(-2.48134137206542,6.29805002672488,91.3166344974079));
#31542=CARTESIAN_POINT('Ctrl Pts',(-2.64255407483943,6.2321393772728,91.3248662694387));
#31543=CARTESIAN_POINT('Ctrl Pts',(-2.80117716484146,6.16000775090184,91.3330980414696));
#31544=CARTESIAN_POINT('Ctrl Pts',(-2.95961084302233,6.0879622569011,91.341319983942));
#31545=CARTESIAN_POINT('Ctrl Pts',(-3.11546074286904,6.00971072463719,91.3495419264144));
#31546=CARTESIAN_POINT('Ctrl Pts',(-3.26820835388604,5.92546227357744,91.3577638688868));
#31547=CARTESIAN_POINT('Ctrl Pts',(-3.42080417331779,5.84129754366957,91.3659776408767));
#31548=CARTESIAN_POINT('Ctrl Pts',(-3.57030353185832,5.75114793491385,91.3741914128666));
#31549=CARTESIAN_POINT('Ctrl Pts',(-3.71620878461308,5.65527022070251,91.3824051848565));
#31550=CARTESIAN_POINT('Ctrl Pts',(-3.86199826809607,5.55946858115568,91.3906124395868));
#31551=CARTESIAN_POINT('Ctrl Pts',(-4.00419902778808,5.45794808468295,91.3988196943172));
#31552=CARTESIAN_POINT('Ctrl Pts',(-4.14233880762939,5.3510109514752,91.4070269490475));
#31553=CARTESIAN_POINT('Ctrl Pts',(-4.28039664000968,5.24413725565359,91.4152293350595));
#31554=CARTESIAN_POINT('Ctrl Pts',(-4.41439800909446,5.13185354304999,91.4234317210715));
#31555=CARTESIAN_POINT('Ctrl Pts',(-4.54390033169494,5.01450483852819,91.4316341070834));
#31556=CARTESIAN_POINT('Ctrl Pts',(-4.67336400099337,4.89719115974824,91.4398340448821));
#31557=CARTESIAN_POINT('Ctrl Pts',(-4.79833103093333,4.77481573787114,91.4480339826808));
#31558=CARTESIAN_POINT('Ctrl Pts',(-4.91839239984003,4.64776346226826,91.4562339204795));
#31559=CARTESIAN_POINT('Ctrl Pts',(-5.03843698106842,4.52072895185289,91.4644327117152));
#31560=CARTESIAN_POINT('Ctrl Pts',(-5.15357702071807,4.38901914998786,91.472631502951));
#31561=CARTESIAN_POINT('Ctrl Pts',(-5.26344081228832,4.25305535063179,91.4808302941867));
#31562=CARTESIAN_POINT('Ctrl Pts',(-5.37330917192722,4.11708589798484,91.4890294263232));
#31563=CARTESIAN_POINT('Ctrl Pts',(-5.47790062107777,3.97686237421657,91.4972285584596));
#31564=CARTESIAN_POINT('Ctrl Pts',(-5.57688413055956,3.83283868618456,91.505427690596));
#31565=CARTESIAN_POINT('Ctrl Pts',(-5.67588971177063,3.68878288318846,91.5136286510069));
#31566=CARTESIAN_POINT('Ctrl Pts',(-5.76928465974368,3.54092552353243,91.5218296114178));
#31567=CARTESIAN_POINT('Ctrl Pts',(-5.85678158973804,3.38974901874837,91.5300305718287));
#31568=CARTESIAN_POINT('Ctrl Pts',(-5.94436052541906,3.23843082518641,91.5382392185137));
#31569=CARTESIAN_POINT('Ctrl Pts',(-6.02603021900859,3.08378758185689,91.5464478651988));
#31570=CARTESIAN_POINT('Ctrl Pts',(-6.10154909944083,2.9263266371191,91.5546565118838));
#31571=CARTESIAN_POINT('Ctrl Pts',(-6.17710403470759,2.76879051610389,91.5628690776073));
#31572=CARTESIAN_POINT('Ctrl Pts',(-6.24650215950944,2.60843434025241,91.5710816433308));
#31573=CARTESIAN_POINT('Ctrl Pts',(-6.30955034489675,2.44578483215784,91.5792942090543));
#31574=CARTESIAN_POINT('Ctrl Pts',(-6.37268504149231,2.28291214546774,91.5875180436031));
#31575=CARTESIAN_POINT('Ctrl Pts',(-6.42945226869713,2.11774017661858,91.5957418781519));
#31576=CARTESIAN_POINT('Ctrl Pts',(-6.4797086371863,1.95081136381079,91.6039657127007));
#31577=CARTESIAN_POINT('Ctrl Pts',(-6.5258847861613,1.79743518562366,91.6115218696751));
#31578=CARTESIAN_POINT('Ctrl Pts',(-6.56656490163375,1.64257621069006,91.6190780266495));
#31579=CARTESIAN_POINT('Ctrl Pts',(-6.60167606144956,1.48666142066172,91.626634183624));
#31580=CARTESIAN_POINT('Ctrl Pts',(-6.65093877381793,1.26790517633836,91.6372358495785));
#31581=CARTESIAN_POINT('Ctrl Pts',(-6.68933642560366,1.046644544309,91.647837515533));
#31582=CARTESIAN_POINT('Ctrl Pts',(-6.71666652858663,0.82382021325287,91.6584391814875));
#31583=CARTESIAN_POINT('Ctrl Pts',(-6.74363790641983,0.603920594613034,
91.6689016937692));
#31584=CARTESIAN_POINT('Ctrl Pts',(-6.75983039058453,0.382497848912048,
91.6793642060509));
#31585=CARTESIAN_POINT('Ctrl Pts',(-6.76509698605697,0.160473578021119,
91.6898267183326));
#31586=CARTESIAN_POINT('Ctrl Pts',(-6.76633077581058,0.108460608368888,
91.6922777401583));
#31587=CARTESIAN_POINT('Ctrl Pts',(-6.76696514953633,0.0564147104294671,
91.6947287619841));
#31588=CARTESIAN_POINT('Ctrl Pts',(-6.76699860320852,0.00434789304140347,
91.6971797838098));
#31589=CARTESIAN_POINT('',(-6.76699927988566,0.00165422498013631,91.3028202161897));
#31590=CARTESIAN_POINT('Ctrl Pts',(3.09917575053247,6.01559628526645,90.6515381108923));
#31591=CARTESIAN_POINT('Ctrl Pts',(2.94407804857715,6.09550108839304,90.6597408227342));
#31592=CARTESIAN_POINT('Ctrl Pts',(2.785778374465,6.1694603469633,90.6679435345761));
#31593=CARTESIAN_POINT('Ctrl Pts',(2.62477392534936,6.23721499074756,90.6761462464181));
#31594=CARTESIAN_POINT('Ctrl Pts',(2.46384860630333,6.30493633464659,90.6843449268114));
#31595=CARTESIAN_POINT('Ctrl Pts',(2.30022149045008,6.36645900014936,90.6925436072047));
#31596=CARTESIAN_POINT('Ctrl Pts',(2.13441204498966,6.42157100888895,90.700742287598));
#31597=CARTESIAN_POINT('Ctrl Pts',(1.9686274665221,6.47667475229767,90.708939738408));
#31598=CARTESIAN_POINT('Ctrl Pts',(1.8006615482882,6.52536963460475,90.7171371892181));
#31599=CARTESIAN_POINT('Ctrl Pts',(1.63105160857606,6.56749264561152,90.7253346400281));
#31600=CARTESIAN_POINT('Ctrl Pts',(1.46144929665274,6.60961376223974,90.733531722178));
#31601=CARTESIAN_POINT('Ctrl Pts',(1.29020345843443,6.64516350893887,90.7417288043278));
#31602=CARTESIAN_POINT('Ctrl Pts',(1.11786430112426,6.67402939791787,90.7499258864777));
#31603=CARTESIAN_POINT('Ctrl Pts',(0.945501571982807,6.7028992350528,90.7581240897903));
#31604=CARTESIAN_POINT('Ctrl Pts',(0.77204557966371,6.72508333402019,90.7663222931029));
#31605=CARTESIAN_POINT('Ctrl Pts',(0.598054450501333,6.74052074206701,90.7745204964155));
#31606=CARTESIAN_POINT('Ctrl Pts',(0.424007900805846,6.75596306731499,90.7827213110612));
#31607=CARTESIAN_POINT('Ctrl Pts',(0.249426231884836,6.76465438943605,90.7909221257069));
#31608=CARTESIAN_POINT('Ctrl Pts',(0.074870443341808,6.76658580206546,90.7991229403526));
#31609=CARTESIAN_POINT('Ctrl Pts',(-0.0998690993695105,6.76851924788508,
90.8073323879625));
#31610=CARTESIAN_POINT('Ctrl Pts',(-0.274582348242346,6.76367856474909,
90.8155418355725));
#31611=CARTESIAN_POINT('Ctrl Pts',(-0.448709576780406,6.75210698343158,
90.8237512831824));
#31612=CARTESIAN_POINT('Ctrl Pts',(-0.622934508067399,6.7405289093024,90.8319653371116));
#31613=CARTESIAN_POINT('Ctrl Pts',(-0.796572407360125,6.72221244597446,
90.8401793910407));
#31614=CARTESIAN_POINT('Ctrl Pts',(-0.969071009046813,6.69725245002942,
90.8483934449698));
#31615=CARTESIAN_POINT('Ctrl Pts',(-1.14181493237204,6.67225695682791,90.8566191806468));
#31616=CARTESIAN_POINT('Ctrl Pts',(-1.31341596828111,6.64059911777658,90.8648449163238));
#31617=CARTESIAN_POINT('Ctrl Pts',(-1.48333318655589,6.60242468019606,90.8730706520008));
#31618=CARTESIAN_POINT('Ctrl Pts',(-1.61159264329477,6.57360928011416,90.8792797248653));
#31619=CARTESIAN_POINT('Ctrl Pts',(-1.73889295021271,6.5410819312111,90.8854887977298));
#31620=CARTESIAN_POINT('Ctrl Pts',(-1.86500840206443,6.50492372439747,90.8916978705944));
#31621=CARTESIAN_POINT('Ctrl Pts',(-2.03209470965791,6.457018878663,90.8999240716132));
#31622=CARTESIAN_POINT('Ctrl Pts',(-2.19756763433466,6.40260523918426,90.9081502726321));
#31623=CARTESIAN_POINT('Ctrl Pts',(-2.3608831728243,6.34180728533082,90.9163764736509));
#31624=CARTESIAN_POINT('Ctrl Pts',(-2.52401526072713,6.28107762516465,90.9245934342667));
#31625=CARTESIAN_POINT('Ctrl Pts',(-2.68499445497847,6.21397805487934,90.9328103948824));
#31626=CARTESIAN_POINT('Ctrl Pts',(-2.84328969871749,6.14068340571039,90.9410273554982));
#31627=CARTESIAN_POINT('Ctrl Pts',(-3.00143890222536,6.06745637681388,90.9492367352998));
#31628=CARTESIAN_POINT('Ctrl Pts',(-3.1569087631929,5.98804580133518,90.9574461151014));
#31629=CARTESIAN_POINT('Ctrl Pts',(-3.3091859943984,5.90267541496883,90.965655494903));
#31630=CARTESIAN_POINT('Ctrl Pts',(-3.46135329092207,5.81736666070723,90.9738589480434));
#31631=CARTESIAN_POINT('Ctrl Pts',(-3.61033223704725,5.72610684029319,90.9820624011838));
#31632=CARTESIAN_POINT('Ctrl Pts',(-3.75563197273801,5.62916667770177,90.9902658543242));
#31633=CARTESIAN_POINT('Ctrl Pts',(-3.90085595782944,5.53227705391815,90.9984650306743));
#31634=CARTESIAN_POINT('Ctrl Pts',(-4.04240425610001,5.42971318614278,91.0066642070245));
#31635=CARTESIAN_POINT('Ctrl Pts',(-4.17981288093117,5.32179042056354,91.0148633833746));
#31636=CARTESIAN_POINT('Ctrl Pts',(-4.31719565025572,5.21388796228148,91.023061016926));
#31637=CARTESIAN_POINT('Ctrl Pts',(-4.45044001211519,5.1006288311366,91.0312586504774));
#31638=CARTESIAN_POINT('Ctrl Pts',(-4.57911287462895,4.98237034767664,91.0394562840288));
#31639=CARTESIAN_POINT('Ctrl Pts',(-4.70777646953871,4.86412038172979,91.0476533271493));
#31640=CARTESIAN_POINT('Ctrl Pts',(-4.8318689561582,4.74087202263994,91.0558503702699));
#31641=CARTESIAN_POINT('Ctrl Pts',(-4.95099216549088,4.61302130682787,91.0640474133905));
#31642=CARTESIAN_POINT('Ctrl Pts',(-5.07012844547349,4.4851565627508,91.0722453559217));
#31643=CARTESIAN_POINT('Ctrl Pts',(-5.18429411731668,4.35268871834763,91.0804432984529));
#31644=CARTESIAN_POINT('Ctrl Pts',(-5.29312953230817,4.21604895064171,91.0886412409841));
#31645=CARTESIAN_POINT('Ctrl Pts',(-5.40199666986208,4.07936935616103,91.0968415729925));
#31646=CARTESIAN_POINT('Ctrl Pts',(-5.50553023251861,3.93851569673618,91.1050419050009));
#31647=CARTESIAN_POINT('Ctrl Pts',(-5.60341231425739,3.79395037347995,91.1132422370094));
#31648=CARTESIAN_POINT('Ctrl Pts',(-5.70139641558099,3.64923437408366,91.1214511159801));
#31649=CARTESIAN_POINT('Ctrl Pts',(-5.79371706655625,3.50079927946118,91.1296599949509));
#31650=CARTESIAN_POINT('Ctrl Pts',(-5.8801004651907,3.3491353390486,91.1378688739216));
#31651=CARTESIAN_POINT('Ctrl Pts',(-5.96653023643713,3.19738998191507,91.146082159609));
#31652=CARTESIAN_POINT('Ctrl Pts',(-6.04701623628843,3.04241264156358,91.1542954452964));
#31653=CARTESIAN_POINT('Ctrl Pts',(-6.12133178471444,2.88471596200471,91.1625087309838));
#31654=CARTESIAN_POINT('Ctrl Pts',(-6.1957560476286,2.72678859163935,91.1707340316959));
#31655=CARTESIAN_POINT('Ctrl Pts',(-6.26399167981509,2.566134262291,91.178959332408));
#31656=CARTESIAN_POINT('Ctrl Pts',(-6.32586062813689,2.40328448448943,91.1871846331201));
#31657=CARTESIAN_POINT('Ctrl Pts',(-6.38181362877759,2.25600650468158,91.1946234254141));
#31658=CARTESIAN_POINT('Ctrl Pts',(-6.43255989262885,2.10693325614759,91.2020622177081));
#31659=CARTESIAN_POINT('Ctrl Pts',(-6.47800353283848,1.95646600495182,91.2095010100021));
#31660=CARTESIAN_POINT('Ctrl Pts',(-6.5388554738026,1.75498073122464,91.2194620286932));
#31661=CARTESIAN_POINT('Ctrl Pts',(-6.59034529481158,1.5505156935588,91.2294230473842));
#31662=CARTESIAN_POINT('Ctrl Pts',(-6.63221952038937,1.34385759415431,91.2393840660753));
#31663=CARTESIAN_POINT('Ctrl Pts',(-6.67382360801738,1.13853268227768,91.2492808244934));
#31664=CARTESIAN_POINT('Ctrl Pts',(-6.70593570481504,0.931042901249972,
91.2591775829115));
#31665=CARTESIAN_POINT('Ctrl Pts',(-6.7283536306715,0.722181708872217,91.2690743413295));
#31666=CARTESIAN_POINT('Ctrl Pts',(-6.75051776729323,0.515684995818658,
91.2788590603573));
#31667=CARTESIAN_POINT('Ctrl Pts',(-6.76320592088888,0.30784775881192,91.288643779385));
#31668=CARTESIAN_POINT('Ctrl Pts',(-6.766269064769,0.0994582482758889,91.2984284984127));
#31669=CARTESIAN_POINT('Ctrl Pts',(-6.76672734614269,0.0682807930567607,
91.2998924043384));
#31670=CARTESIAN_POINT('Ctrl Pts',(-6.76697027192187,0.0370910152686651,
91.3013563102641));
#31671=CARTESIAN_POINT('Ctrl Pts',(-6.7669974352806,0.00589159620233154,
91.3028202161897));
#31672=CARTESIAN_POINT('Ctrl Pts',(-6.767,4.78819593890031E-12,91.3028202161897));
#31673=CARTESIAN_POINT('Ctrl Pts',(-6.76700000000013,-0.18600724941091,
91.3115697279957));
#31674=CARTESIAN_POINT('Ctrl Pts',(-6.75932637295464,-0.372014355522786,
91.3203192398016));
#31675=CARTESIAN_POINT('Ctrl Pts',(-6.74400518266967,-0.557389537150331,
91.3290687516076));
#31676=CARTESIAN_POINT('Ctrl Pts',(-6.72868405709696,-0.742763935806849,
91.3378182264581));
#31677=CARTESIAN_POINT('Ctrl Pts',(-6.70571545653052,-0.927506129690664,
91.3465677013087));
#31678=CARTESIAN_POINT('Ctrl Pts',(-6.6751773941572,-1.11098863924556,91.3553171761592));
#31679=CARTESIAN_POINT('Ctrl Pts',(-6.64463945823145,-1.29447038906274,
91.3640666147812));
#31680=CARTESIAN_POINT('Ctrl Pts',(-6.60653217027203,-1.47669218228016,
91.3728160534032));
#31681=CARTESIAN_POINT('Ctrl Pts',(-6.56098496116756,-1.65703510503947,
91.3815654920252));
#31682=CARTESIAN_POINT('Ctrl Pts',(-6.51543793687555,-1.83737729603889,
91.3903148951454));
#31683=CARTESIAN_POINT('Ctrl Pts',(-6.46245112202668,-2.01584035396964,
91.3990642982657));
#31684=CARTESIAN_POINT('Ctrl Pts',(-6.40220448416259,-2.19181813638095,
91.407813701386));
#31685=CARTESIAN_POINT('Ctrl Pts',(-6.34195808575197,-2.36779521935917,
91.4165630697312));
#31686=CARTESIAN_POINT('Ctrl Pts',(-6.27445201489237,-2.54128677544823,
91.4253124380765));
#31687=CARTESIAN_POINT('Ctrl Pts',(-6.19991555136176,-2.71170355237857,
91.4340618064218));
#31688=CARTESIAN_POINT('Ctrl Pts',(-6.12537937789035,-2.88211966613079,
91.4428111407189));
#31689=CARTESIAN_POINT('Ctrl Pts',(-6.04381298133618,-3.04946076210442,
91.4515604750159));
#31690=CARTESIAN_POINT('Ctrl Pts',(-5.95549339426313,-3.21315848206843,
91.4603098093129));
#31691=CARTESIAN_POINT('Ctrl Pts',(-5.86717414355159,-3.37685557859639,
91.4690591102885));
#31692=CARTESIAN_POINT('Ctrl Pts',(-5.77210188986228,-3.53690907467328,
91.4778084112641));
#31693=CARTESIAN_POINT('Ctrl Pts',(-5.67059953467048,-3.69277536784935,
91.4865577122397));
#31694=CARTESIAN_POINT('Ctrl Pts',(-5.56909755761758,-3.84864108035802,
91.4953069806204));
#31695=CARTESIAN_POINT('Ctrl Pts',(-5.46116568338077,-4.00031938104269,
91.5040562490012));
#31696=CARTESIAN_POINT('Ctrl Pts',(-5.34717048686137,-4.14729511663189,
91.5128055173819));
#31697=CARTESIAN_POINT('Ctrl Pts',(-5.23317570555541,-4.29427031688012,
91.5215547538945));
#31698=CARTESIAN_POINT('Ctrl Pts',(-5.11311782178829,-4.43654275987102,
91.5303039904072));
#31699=CARTESIAN_POINT('Ctrl Pts',(-4.98740459172039,-4.57362924147623,
91.5390532269198));
#31700=CARTESIAN_POINT('Ctrl Pts',(-4.86169180910834,-4.71071523514433,
91.5478024322909));
#31701=CARTESIAN_POINT('Ctrl Pts',(-4.73032391415413,-4.84261509316543,
91.556551637662));
#31702=CARTESIAN_POINT('Ctrl Pts',(-4.5937470723725,-4.96888084331563,91.5653008430332));
#31703=CARTESIAN_POINT('Ctrl Pts',(-4.45717070537355,-5.09514615452766,
91.5740500179894));
#31704=CARTESIAN_POINT('Ctrl Pts',(-4.31538563819458,-5.21577720253675,
91.5827991929456));
#31705=CARTESIAN_POINT('Ctrl Pts',(-4.16887341290592,-5.33036429028693,
91.5915483679019));
#31706=CARTESIAN_POINT('Ctrl Pts',(-4.02236168477282,-5.44495098921219,
91.6002975131698));
#31707=CARTESIAN_POINT('Ctrl Pts',(-3.87112305634381,-5.55349359238799,
91.6090466584377));
#31708=CARTESIAN_POINT('Ctrl Pts',(-3.71567117316673,-5.65562346102512,
91.6177958037056));
#31709=CARTESIAN_POINT('Ctrl Pts',(-3.56021980457233,-5.75775299158811,
91.6265449200118));
#31710=CARTESIAN_POINT('Ctrl Pts',(-3.40055544862311,-5.85346967275398,
91.635294036318));
#31711=CARTESIAN_POINT('Ctrl Pts',(-3.23722036323317,-5.94244842803608,
91.6440431526241));
#31712=CARTESIAN_POINT('Ctrl Pts',(-3.0738858049595,-6.03142689616525,91.6527922406951));
#31713=CARTESIAN_POINT('Ctrl Pts',(-2.90688079257599,-6.11366734484874,
91.661541328766));
#31714=CARTESIAN_POINT('Ctrl Pts',(-2.73677251094495,-6.18889046787355,
91.670290416837));
#31715=CARTESIAN_POINT('Ctrl Pts',(-2.56666476416543,-6.26411335438311,
91.6790394773992));
#31716=CARTESIAN_POINT('Ctrl Pts',(-2.3934540297201,-6.33231884350321,91.6877885379614));
#31717=CARTESIAN_POINT('Ctrl Pts',(-2.21772856473975,-6.39327529621065,
91.6965375985236));
#31718=CARTESIAN_POINT('Ctrl Pts',(-2.04200363768211,-6.454231562321,91.7052866323036));
#31719=CARTESIAN_POINT('Ctrl Pts',(-1.86376426620041,-6.50793874252071,
91.7140356660836));
#31720=CARTESIAN_POINT('Ctrl Pts',(-1.68361578194642,-6.55421443796135,
91.7227846998636));
#31721=CARTESIAN_POINT('Ctrl Pts',(-1.50346783419843,-6.60048999558685,
91.7315337075879));
#31722=CARTESIAN_POINT('Ctrl Pts',(-1.32141106257244,-6.63933404145495,
91.7402827153121));
#31723=CARTESIAN_POINT('Ctrl Pts',(-1.13806375959064,-6.67061465527026,
91.7490317230363));
#31724=CARTESIAN_POINT('Ctrl Pts',(-0.954716987419518,-6.70189517852475,
91.7577807054312));
#31725=CARTESIAN_POINT('Ctrl Pts',(-0.770079973810406,-6.72561226535821,
91.766529687826));
#31726=CARTESIAN_POINT('Ctrl Pts',(-0.584779770553154,-6.74168536939776,
91.7752786702209));
#31727=CARTESIAN_POINT('Ctrl Pts',(-0.391490647554569,-6.7584514394239,
91.784404850897));
#31728=CARTESIAN_POINT('Ctrl Pts',(-0.197480213104954,-6.76689975924025,
91.793531031573));
#31729=CARTESIAN_POINT('Ctrl Pts',(-0.00346532629837374,-6.76699911271707,
91.8026572122491));
#31730=CARTESIAN_POINT('Ctrl Pts',(0.184486595295469,-6.76709536139775,
91.811498199779));
#31731=CARTESIAN_POINT('Ctrl Pts',(0.372442378184638,-6.75935659726773,
91.8203391873089));
#31732=CARTESIAN_POINT('Ctrl Pts',(0.559750217721486,-6.74380965729021,
91.8291801748389));
#31733=CARTESIAN_POINT('Ctrl Pts',(0.745129914457184,-6.7284227571726,91.8379301534366));
#31734=CARTESIAN_POINT('Ctrl Pts',(0.92987465631364,-6.7053877227348,91.8466801320344));
#31735=CARTESIAN_POINT('Ctrl Pts',(1.11335688289726,-6.67478280180751,91.8554301106322));
#31736=CARTESIAN_POINT('Ctrl Pts',(1.29683723118795,-6.64417819418035,91.8641799996571));
#31737=CARTESIAN_POINT('Ctrl Pts',(1.47905480730164,-6.60600390230091,91.872929888682));
#31738=CARTESIAN_POINT('Ctrl Pts',(1.65939064804728,-6.56038959797155,91.881679777707));
#31739=CARTESIAN_POINT('Ctrl Pts',(1.83972470264193,-6.51477574543277,91.8904295800679));
#31740=CARTESIAN_POINT('Ctrl Pts',(2.01817678125785,-6.4617220982012,91.8991793824289));
#31741=CARTESIAN_POINT('Ctrl Pts',(2.19414072347625,-6.40140886724033,91.9079291847898));
#31742=CARTESIAN_POINT('Ctrl Pts',(2.37010298132052,-6.34109621361391,91.9166789033953));
#31743=CARTESIAN_POINT('Ctrl Pts',(2.54357687926878,-6.27352420825985,91.9254286220008));
#31744=CARTESIAN_POINT('Ctrl Pts',(2.71397317789946,-6.19892237325507,91.9341783406063));
#31745=CARTESIAN_POINT('Ctrl Pts',(2.88436790207172,-6.12432122756977,91.9429279783646));
#31746=CARTESIAN_POINT('Ctrl Pts',(3.05168482126224,-6.04269049717433,91.9516776161228));
#31747=CARTESIAN_POINT('Ctrl Pts',(3.21535561997352,-5.95430745234949,91.9604272538811));
#31748=CARTESIAN_POINT('Ctrl Pts',(3.37902496075246,-5.86592519481537,91.9691768137001));
#31749=CARTESIAN_POINT('Ctrl Pts',(3.53904799384842,-5.77079087940252,91.9779263735191));
#31750=CARTESIAN_POINT('Ctrl Pts',(3.69488118814954,-5.66922763747044,91.9866759333381));
#31751=CARTESIAN_POINT('Ctrl Pts',(3.85071304610807,-5.5676652664907,91.9954254181256));
#31752=CARTESIAN_POINT('Ctrl Pts',(4.00235489705947,-5.45967423580729,92.004174902913));
#31753=CARTESIAN_POINT('Ctrl Pts',(4.14929168607638,-5.34562133936341,92.0129243877005));
#31754=CARTESIAN_POINT('Ctrl Pts',(4.29622726385744,-5.23156938308542,92.0216738003638));
#31755=CARTESIAN_POINT('Ctrl Pts',(4.43845763092056,-5.11145583677211,92.030423213027));
#31756=CARTESIAN_POINT('Ctrl Pts',(4.57549970660954,-4.98568866204219,92.0391726256904));
#31757=CARTESIAN_POINT('Ctrl Pts',(4.71254069815292,-4.85992248226164,92.0479219691367));
#31758=CARTESIAN_POINT('Ctrl Pts',(4.84439326931316,-4.72850295734001,92.056671312583));
#31759=CARTESIAN_POINT('Ctrl Pts',(4.97060959434704,-4.59187644221675,92.0654206560293));
#31760=CARTESIAN_POINT('Ctrl Pts',(5.09682496280528,-4.4552509625665,92.0741699331656));
#31761=CARTESIAN_POINT('Ctrl Pts',(5.21740397615858,-4.31341878218304,92.0829192103019));
#31762=CARTESIAN_POINT('Ctrl Pts',(5.33193710451958,-4.16686161438647,92.0916684874382));
#31763=CARTESIAN_POINT('Ctrl Pts',(5.44646940289404,-4.02030550864485,92.1004177011712));
#31764=CARTESIAN_POINT('Ctrl Pts',(5.55495572749684,-3.86902470980106,92.1091669149042));
#31765=CARTESIAN_POINT('Ctrl Pts',(5.65702762491472,-3.71353301465756,92.1179161286371));
#31766=CARTESIAN_POINT('Ctrl Pts',(5.75909881655173,-3.55804239466862,92.1266652818733));
#31767=CARTESIAN_POINT('Ctrl Pts',(5.85475551250803,-3.39834117619517,92.1354144351094));
#31768=CARTESIAN_POINT('Ctrl Pts',(5.94367283728118,-3.23497174691927,92.1441635883455));
#31769=CARTESIAN_POINT('Ctrl Pts',(6.03258957676336,-3.07160339300917,92.152912683991));
#31770=CARTESIAN_POINT('Ctrl Pts',(6.11476689685311,-2.90456712829448,92.1616617796366));
#31771=CARTESIAN_POINT('Ctrl Pts',(6.18992570525289,-2.73443024475842,92.1704108752821));
#31772=CARTESIAN_POINT('Ctrl Pts',(6.26508404388732,-2.56429442462946,92.1791599162431));
#31773=CARTESIAN_POINT('Ctrl Pts',(6.33322384283356,-2.39105828655887,92.1879089572042));
#31774=CARTESIAN_POINT('Ctrl Pts',(6.39411368720077,-2.21531017131953,92.1966579981652));
#31775=CARTESIAN_POINT('Ctrl Pts',(6.45500317120931,-2.03956309619386,92.2054069873476));
#31776=CARTESIAN_POINT('Ctrl Pts',(6.5086426927011,-1.86130434438504,92.21415597653));
#31777=CARTESIAN_POINT('Ctrl Pts',(6.55485008446367,-1.68113930719815,92.2229049657124));
#31778=CARTESIAN_POINT('Ctrl Pts',(6.60199664749432,-1.49731239211713,92.2318317792418));
#31779=CARTESIAN_POINT('Ctrl Pts',(6.64140563640931,-1.31150116499548,92.2407585927711));
#31780=CARTESIAN_POINT('Ctrl Pts',(6.67293772282192,-1.12436255155541,92.2496854063005));
#31781=CARTESIAN_POINT('Ctrl Pts',(6.70384494949887,-0.940932395050179,
92.258435320456));
#31782=CARTESIAN_POINT('Ctrl Pts',(6.72718449348943,-0.756227260505578,
92.2671852346115));
#31783=CARTESIAN_POINT('Ctrl Pts',(6.74287707373942,-0.570874564540583,
92.2759351487671));
#31784=CARTESIAN_POINT('Ctrl Pts',(6.75856934538676,-0.385525513631416,
92.2846848908511));
#31785=CARTESIAN_POINT('Ctrl Pts',(6.76661493004106,-0.199529212417218,
92.293434632935));
#31786=CARTESIAN_POINT('Ctrl Pts',(6.76698649908907,-0.013517438599468,
92.302184375019));
#31787=CARTESIAN_POINT('Ctrl Pts',(6.76735806132387,0.172490924446717,92.3109339566649));
#31788=CARTESIAN_POINT('Ctrl Pts',(6.76005588896284,0.358514472902324,92.3196835383108));
#31789=CARTESIAN_POINT('Ctrl Pts',(6.74510478454577,0.543921359663106,92.3284331199567));
#31790=CARTESIAN_POINT('Ctrl Pts',(6.73015393440677,0.729325093151422,92.3371825527958));
#31791=CARTESIAN_POINT('Ctrl Pts',(6.70755443556883,0.914111900257411,92.3459319856348));
#31792=CARTESIAN_POINT('Ctrl Pts',(6.677383046823,1.09765415591652,92.3546814184739));
#31793=CARTESIAN_POINT('Ctrl Pts',(6.64721213111837,1.28119353391397,92.3634307141352));
#31794=CARTESIAN_POINT('Ctrl Pts',(6.60946960955465,1.46348811672787,92.3721800097965));
#31795=CARTESIAN_POINT('Ctrl Pts',(6.56428366991147,1.64391876348366,92.3809293054578));
#31796=CARTESIAN_POINT('Ctrl Pts',(6.51909837867677,1.82434682109859,92.3896784755687));
#31797=CARTESIAN_POINT('Ctrl Pts',(6.46646995271877,2.00291071820587,92.3984276456795));
#31798=CARTESIAN_POINT('Ctrl Pts',(6.40657713281501,2.17900400212845,92.4071768157903));
#31799=CARTESIAN_POINT('Ctrl Pts',(6.34668509279007,2.355094993098,92.4159258719761));
#31800=CARTESIAN_POINT('Ctrl Pts',(6.27952894037469,2.52871516398265,92.4246749281619));
#31801=CARTESIAN_POINT('Ctrl Pts',(6.20533675061385,2.69927486771562,92.4334239843476));
#31802=CARTESIAN_POINT('Ctrl Pts',(6.12832117907854,2.87632521636056,92.4425059856299));
#31803=CARTESIAN_POINT('Ctrl Pts',(6.04372366626017,3.05007728920121,92.4515879869122));
#31804=CARTESIAN_POINT('Ctrl Pts',(5.95185378007806,3.2198952747831,92.4606699881945));
#31805=CARTESIAN_POINT('Ctrl Pts',(5.86334450817307,3.38350129286863,92.4694197685016));
#31806=CARTESIAN_POINT('Ctrl Pts',(5.76808562057189,3.5434556712507,92.4781695488087));
#31807=CARTESIAN_POINT('Ctrl Pts',(5.66640068804416,3.69921508465414,92.4869193291158));
#31808=CARTESIAN_POINT('Ctrl Pts',(5.56471941107854,3.85496889852383,92.4956687948693));
#31809=CARTESIAN_POINT('Ctrl Pts',(5.45661270815044,4.00652780919732,92.5044182606228));
#31810=CARTESIAN_POINT('Ctrl Pts',(5.34244776449044,4.15337704569319,92.5131677263763));
#31811=CARTESIAN_POINT('Ctrl Pts',(5.22828631819522,4.30022178356339,92.5219169240959));
#31812=CARTESIAN_POINT('Ctrl Pts',(5.10806717843992,4.44235690972767,92.5306661218154));
#31813=CARTESIAN_POINT('Ctrl Pts',(4.98219864544639,4.57929969070732,92.539415319535));
#31814=CARTESIAN_POINT('Ctrl Pts',(4.85633329943941,4.71623900430087,92.5481642957253));
#31815=CARTESIAN_POINT('Ctrl Pts',(4.72481904033562,4.84798602483701,92.5569132719155));
#31816=CARTESIAN_POINT('Ctrl Pts',(4.58810250737109,4.97409332259208,92.5656622481058));
#31817=CARTESIAN_POINT('Ctrl Pts',(4.45137708685552,5.10020881822214,92.574411793042));
#31818=CARTESIAN_POINT('Ctrl Pts',(4.30944892635961,5.22068366308007,92.5831613379781));
#31819=CARTESIAN_POINT('Ctrl Pts',(4.16280009466571,5.33510865604921,92.5919108829143));
#31820=CARTESIAN_POINT('Ctrl Pts',(4.01615988348681,5.44952692272972,92.6006599135226));
#31821=CARTESIAN_POINT('Ctrl Pts',(3.86479978232104,5.55789587288715,92.6094089441309));
#31822=CARTESIAN_POINT('Ctrl Pts',(3.70923383580922,5.65984746713973,92.6181579747392));
#31823=CARTESIAN_POINT('Ctrl Pts',(3.55366577799393,5.76180044505474,92.6269071240872));
#31824=CARTESIAN_POINT('Ctrl Pts',(3.3938920002669,5.85733573571146,92.6356562734352));
#31825=CARTESIAN_POINT('Ctrl Pts',(3.23045513625889,5.9461288762201,92.6444054227832));
#31826=CARTESIAN_POINT('Ctrl Pts',(3.18695122151482,5.96976399206739,92.6467342868961));
#31827=CARTESIAN_POINT('Ctrl Pts',(3.14318791262623,5.99292165435354,92.6490631510091));
#31828=CARTESIAN_POINT('Ctrl Pts',(3.09917575053273,6.01559628526632,92.651392015122));
#31829=CARTESIAN_POINT('Origin',(0.,0.,-3.69717978381041));
#31830=CARTESIAN_POINT('',(3.09917575053266,6.01559628526635,95.0455637664379));
#31831=CARTESIAN_POINT('',(3.09917575053252,6.01559628526643,94.6512396476018));
#31832=CARTESIAN_POINT('',(3.09917575053259,6.01559628526639,-3.69717978381041));
#31833=CARTESIAN_POINT('',(-6.76699989852763,0.00117189038962358,93.6971797872887));
#31834=CARTESIAN_POINT('Ctrl Pts',(-6.7669998985405,0.00117181604119456,
93.6971797907676));
#31835=CARTESIAN_POINT('Ctrl Pts',(-6.76703136317471,-0.180530062912324,
93.7056818217919));
#31836=CARTESIAN_POINT('Ctrl Pts',(-6.75974012411332,-0.362125139993033,
93.7141838528163));
#31837=CARTESIAN_POINT('Ctrl Pts',(-6.74517804147444,-0.543012144257411,
93.7226858838406));
#31838=CARTESIAN_POINT('Ctrl Pts',(-6.73060282379904,-0.724062309071471,
93.7311955837191));
#31839=CARTESIAN_POINT('Ctrl Pts',(-6.70874370102569,-0.90440281033541,
93.7397052835976));
#31840=CARTESIAN_POINT('Ctrl Pts',(-6.67970414778261,-1.08343966056991,
93.7482149834761));
#31841=CARTESIAN_POINT('Ctrl Pts',(-6.64954898098444,-1.26935457588032,
93.7570516007991));
#31842=CARTESIAN_POINT('Ctrl Pts',(-6.611650843814,-1.45386331083921,93.765888218122));
#31843=CARTESIAN_POINT('Ctrl Pts',(-6.56618291935681,-1.63631624985726,
93.774724835445));
#31844=CARTESIAN_POINT('Ctrl Pts',(-6.52227459259335,-1.81251086091544,
93.7832583474874));
#31845=CARTESIAN_POINT('Ctrl Pts',(-6.47130730698831,-1.98678808993954,
93.7917918595299));
#31846=CARTESIAN_POINT('Ctrl Pts',(-6.41348694788727,-2.15858151786763,
93.8003253715723));
#31847=CARTESIAN_POINT('Ctrl Pts',(-6.35258597155414,-2.33952794661864,
93.8093135415355));
#31848=CARTESIAN_POINT('Ctrl Pts',(-6.28408193108863,-2.51771829154907,
93.8183017114988));
#31849=CARTESIAN_POINT('Ctrl Pts',(-6.20827160375272,-2.69251790969674,
93.827289881462));
#31850=CARTESIAN_POINT('Ctrl Pts',(-6.1324612764168,-2.86731752784441,93.8362780514252));
#31851=CARTESIAN_POINT('Ctrl Pts',(-6.04934489877415,-3.03872608388942,
93.8452662213884));
#31852=CARTESIAN_POINT('Ctrl Pts',(-5.95927365459807,-3.20614199773082,
93.8542543913516));
#31853=CARTESIAN_POINT('Ctrl Pts',(-5.87263415123288,-3.36717931617058,
93.8629001094041));
#31854=CARTESIAN_POINT('Ctrl Pts',(-5.77938579804812,-3.52484672363379,
93.8715458274565));
#31855=CARTESIAN_POINT('Ctrl Pts',(-5.67980653833225,-3.67859846777522,
93.8801915455089));
#31856=CARTESIAN_POINT('Ctrl Pts',(-5.58035511809212,-3.83215282601099,
93.8888261642213));
#31857=CARTESIAN_POINT('Ctrl Pts',(-5.47458916316032,-3.98180129009379,
93.8974607829336));
#31858=CARTESIAN_POINT('Ctrl Pts',(-5.36283216365784,-4.12702316257577,
93.906095401646));
#31859=CARTESIAN_POINT('Ctrl Pts',(-5.24712834107501,-4.27737370745086,
93.9150349615484));
#31860=CARTESIAN_POINT('Ctrl Pts',(-5.12500271662077,-4.42297899790175,
93.9239745214508));
#31861=CARTESIAN_POINT('Ctrl Pts',(-4.99686465761375,-4.56329185933692,
93.9329140813532));
#31862=CARTESIAN_POINT('Ctrl Pts',(-4.87344108767164,-4.69844229318401,
93.9415247346238));
#31863=CARTESIAN_POINT('Ctrl Pts',(-4.74443981405401,-4.8286825042295,93.9501353878943));
#31864=CARTESIAN_POINT('Ctrl Pts',(-4.61026922422516,-4.95355495378444,
93.9587460411649));
#31865=CARTESIAN_POINT('Ctrl Pts',(-4.47622563583541,-5.07830920321209,
93.967348543876));
#31866=CARTESIAN_POINT('Ctrl Pts',(-4.33702270929072,-5.19770561408688,
93.9759510465872));
#31867=CARTESIAN_POINT('Ctrl Pts',(-4.19310659484056,-5.3113224421329,93.9845535492984));
#31868=CARTESIAN_POINT('Ctrl Pts',(-4.04935245508128,-5.4248113967252,93.9931463700658));
#31869=CARTESIAN_POINT('Ctrl Pts',(-3.9008959488065,-5.53253355679588,94.0017391908333));
#31870=CARTESIAN_POINT('Ctrl Pts',(-3.7482174644504,-5.63410639224971,94.0103320116008));
#31871=CARTESIAN_POINT('Ctrl Pts',(-3.73022361156676,-5.64607721227611,
94.0113447145589));
#31872=CARTESIAN_POINT('Ctrl Pts',(-3.71217115528374,-5.65796266538561,
94.012357417517));
#31873=CARTESIAN_POINT('Ctrl Pts',(-3.69406091246685,-5.66976216211797,
94.0133701204751));
#31874=CARTESIAN_POINT('Ctrl Pts',(-3.54035127444973,-5.76990970789374,
94.0219653782351));
#31875=CARTESIAN_POINT('Ctrl Pts',(-3.382657288299,-5.86374391978502,94.0305606359951));
#31876=CARTESIAN_POINT('Ctrl Pts',(-3.2215207646025,-5.95097411885104,94.0391558937552));
#31877=CARTESIAN_POINT('Ctrl Pts',(-3.06023334338487,-6.03828600529932,
94.0477592006096));
#31878=CARTESIAN_POINT('Ctrl Pts',(-2.89549721833821,-6.11898138930087,
94.0563625074641));
#31879=CARTESIAN_POINT('Ctrl Pts',(-2.72787643941772,-6.19281673645117,
94.0649658143185));
#31880=CARTESIAN_POINT('Ctrl Pts',(-2.55330604487707,-6.26971332269832,
94.0739258172585));
#31881=CARTESIAN_POINT('Ctrl Pts',(-2.37560705618886,-6.33916877055169,
94.0828858201985));
#31882=CARTESIAN_POINT('Ctrl Pts',(-2.19543541894558,-6.40096495235205,
94.0918458231385));
#31883=CARTESIAN_POINT('Ctrl Pts',(-2.02196310260359,-6.46046336709713,
94.1004726663433));
#31884=CARTESIAN_POINT('Ctrl Pts',(-1.84619899975639,-6.5128617937432,94.109099509548));
#31885=CARTESIAN_POINT('Ctrl Pts',(-1.66874068540826,-6.55801749958501,
94.1177263527527));
#31886=CARTESIAN_POINT('Ctrl Pts',(-1.4911127657688,-6.60321636286733,94.1263614410388));
#31887=CARTESIAN_POINT('Ctrl Pts',(-1.31178770006376,-6.64115862191189,
94.134996529325));
#31888=CARTESIAN_POINT('Ctrl Pts',(-1.13137205816807,-6.67175286307853,
94.1436316176112));
#31889=CARTESIAN_POINT('Ctrl Pts',(-0.950688462838568,-6.70239254283292,
94.1522795307363));
#31890=CARTESIAN_POINT('Ctrl Pts',(-0.768911356462438,-6.72566235315488,
94.1609274438615));
#31891=CARTESIAN_POINT('Ctrl Pts',(-0.586652711046564,-6.74152264674841,
94.1695753569866));
#31892=CARTESIAN_POINT('Ctrl Pts',(-0.566206065584869,-6.7433019302457,
94.1705455211906));
#31893=CARTESIAN_POINT('Ctrl Pts',(-0.54575335970442,-6.74498801580856,
94.1715156853946));
#31894=CARTESIAN_POINT('Ctrl Pts',(-0.525295456907292,-6.74658088834282,
94.1724858495986));
#31895=CARTESIAN_POINT('Ctrl Pts',(-0.351861214087626,-6.76008464992711,
94.1807105291174));
#31896=CARTESIAN_POINT('Ctrl Pts',(-0.17767736880436,-6.76691420521858,
94.1889352086362));
#31897=CARTESIAN_POINT('Ctrl Pts',(-0.00329818154050613,-6.76699919624633,
94.197159888155));
#31898=CARTESIAN_POINT('Ctrl Pts',(0.170897713470069,-6.7670840979389,94.2053759226051));
#31899=CARTESIAN_POINT('Ctrl Pts',(0.34528818611701,-6.76043855250093,94.2135919570553));
#31900=CARTESIAN_POINT('Ctrl Pts',(0.519313869050381,-6.74704395312584,
94.2218079915054));
#31901=CARTESIAN_POINT('Ctrl Pts',(0.693191488953623,-6.73366075002822,
94.23001703566));
#31902=CARTESIAN_POINT('Ctrl Pts',(0.866704581925109,-6.71353995655838,
94.2382260798146));
#31903=CARTESIAN_POINT('Ctrl Pts',(1.03929369751265,-6.68671500890463,94.2464351239692));
#31904=CARTESIAN_POINT('Ctrl Pts',(1.21177053245603,-6.659907512655,94.2546388275972));
#31905=CARTESIAN_POINT('Ctrl Pts',(1.38332423446943,-6.62640460478376,94.2628425312252));
#31906=CARTESIAN_POINT('Ctrl Pts',(1.55340029863261,-6.58629155991504,94.2710462348532));
#31907=CARTESIAN_POINT('Ctrl Pts',(1.72339976704798,-6.54619658042597,94.2792462438471));
#31908=CARTESIAN_POINT('Ctrl Pts',(1.89192257529227,-6.49949747695438,94.2874462528411));
#31909=CARTESIAN_POINT('Ctrl Pts',(2.05842414827465,-6.44633066370317,94.295646261835));
#31910=CARTESIAN_POINT('Ctrl Pts',(2.22491240744009,-6.39316810178249,94.303845615139));
#31911=CARTESIAN_POINT('Ctrl Pts',(2.38937940944284,-6.33353896082529,94.3120449684429));
#31912=CARTESIAN_POINT('Ctrl Pts',(2.55129513111715,-6.2676297077873,94.3202443217468));
#31913=CARTESIAN_POINT('Ctrl Pts',(2.7132097971487,-6.2017208844582,94.3284436215934));
#31914=CARTESIAN_POINT('Ctrl Pts',(2.87257288351492,-6.12953216476514,94.33664292144));
#31915=CARTESIAN_POINT('Ctrl Pts',(3.02887388659421,-6.05129837135038,94.3448422212866));
#31916=CARTESIAN_POINT('Ctrl Pts',(3.18520222517252,-5.97305089561918,94.3530429551096));
#31917=CARTESIAN_POINT('Ctrl Pts',(3.33846709290998,-5.88875640029779,94.3612436889325));
#31918=CARTESIAN_POINT('Ctrl Pts',(3.48818210770356,-5.79869593818272,94.3694444227555));
#31919=CARTESIAN_POINT('Ctrl Pts',(3.63795046623988,-5.70860338735478,94.3776480785155));
#31920=CARTESIAN_POINT('Ctrl Pts',(3.78416614522528,-5.61274096190219,94.3858517342754));
#31921=CARTESIAN_POINT('Ctrl Pts',(3.92637125084586,-5.51143337077853,94.3940553900354));
#31922=CARTESIAN_POINT('Ctrl Pts',(4.0687392615568,-5.41000972529652,94.4022684436104));
#31923=CARTESIAN_POINT('Ctrl Pts',(4.2070872277713,-5.30312866025565,94.4104814971854));
#31924=CARTESIAN_POINT('Ctrl Pts',(4.34098906656382,-5.19115622226623,94.4186945507604));
#31925=CARTESIAN_POINT('Ctrl Pts',(4.47497013807854,-5.07911752767306,94.4269124641835));
#31926=CARTESIAN_POINT('Ctrl Pts',(4.60449957238568,-4.9619816948056,94.4351303776066));
#31927=CARTESIAN_POINT('Ctrl Pts',(4.72918786633991,-4.84015197332309,94.4433482910297));
#31928=CARTESIAN_POINT('Ctrl Pts',(4.85407063197312,-4.7181322385704,94.4515790216256));
#31929=CARTESIAN_POINT('Ctrl Pts',(4.9740969216564,-4.59140424509049,94.4598097522216));
#31930=CARTESIAN_POINT('Ctrl Pts',(5.08891638578258,-4.46040570111213,94.4680404828176));
#31931=CARTESIAN_POINT('Ctrl Pts',(5.19436433143749,-4.34009920559389,94.4755994244935));
#31932=CARTESIAN_POINT('Ctrl Pts',(5.29542107279306,-4.21619137373607,94.4831583661693));
#31933=CARTESIAN_POINT('Ctrl Pts',(5.39184783388915,-4.08904217833283,94.4907173078452));
#31934=CARTESIAN_POINT('Ctrl Pts',(5.49586416920154,-3.95188530203182,94.4988712000119));
#31935=CARTESIAN_POINT('Ctrl Pts',(5.5948140149615,-3.81053223763217,94.5070250921787));
#31936=CARTESIAN_POINT('Ctrl Pts',(5.68833552564354,-3.66539601512602,94.5151789843454));
#31937=CARTESIAN_POINT('Ctrl Pts',(5.78174291395415,-3.52043689936003,94.5233229264856));
#31938=CARTESIAN_POINT('Ctrl Pts',(5.86973495673427,-3.37170411874182,94.5314668686258));
#31939=CARTESIAN_POINT('Ctrl Pts',(5.95198971378876,-3.21964399382181,94.539610810766));
#31940=CARTESIAN_POINT('Ctrl Pts',(6.03416141004451,-3.06773741911438,94.5477465291589));
#31941=CARTESIAN_POINT('Ctrl Pts',(6.11060718164476,-2.912510508299,94.5558822475518));
#31942=CARTESIAN_POINT('Ctrl Pts',(6.18104812068848,-2.7544388048627,94.5640179659447));
#31943=CARTESIAN_POINT('Ctrl Pts',(6.2514327457875,-2.59649347170604,94.5721471802449));
#31944=CARTESIAN_POINT('Ctrl Pts',(6.31582194860431,-2.43570820665953,94.5802763945451));
#31945=CARTESIAN_POINT('Ctrl Pts',(6.37398255637531,-2.27258341343576,94.5884056088453));
#31946=CARTESIAN_POINT('Ctrl Pts',(6.43210889669107,-2.10955473116684,94.5965300335208));
#31947=CARTESIAN_POINT('Ctrl Pts',(6.48401382774071,-1.94418960933513,94.6046544581963));
#31948=CARTESIAN_POINT('Ctrl Pts',(6.52951216284625,-1.77700869869648,94.6127788828717));
#31949=CARTESIAN_POINT('Ctrl Pts',(6.57528670197219,-1.60881289290735,94.6209526280059));
#31950=CARTESIAN_POINT('Ctrl Pts',(6.61457645356851,-1.4387795230129,94.6291263731401));
#31951=CARTESIAN_POINT('Ctrl Pts',(6.64724352095938,-1.26745515623374,94.6373001182743));
#31952=CARTESIAN_POINT('Ctrl Pts',(6.67970139800974,-1.09722790056639,94.6454215211364));
#31953=CARTESIAN_POINT('Ctrl Pts',(6.70562111567153,-0.925726502013933,
94.6535429239986));
#31954=CARTESIAN_POINT('Ctrl Pts',(6.72491858694054,-0.753497842745212,
94.6616643268607));
#31955=CARTESIAN_POINT('Ctrl Pts',(6.74421755018839,-0.581255867663614,
94.669786357627));
#31956=CARTESIAN_POINT('Ctrl Pts',(6.75689320639271,-0.40828688357517,94.6779083883932));
#31957=CARTESIAN_POINT('Ctrl Pts',(6.76291332800492,-0.235143185938755,
94.6860304191595));
#31958=CARTESIAN_POINT('Ctrl Pts',(6.76893506143143,-0.061953131184593,
94.6941546245006));
#31959=CARTESIAN_POINT('Ctrl Pts',(6.76829769939601,0.111411364646957,94.7022788298417));
#31960=CARTESIAN_POINT('Ctrl Pts',(6.76102114450321,0.28439775593438,94.7104030351829));
#31961=CARTESIAN_POINT('Ctrl Pts',(6.75366582593869,0.459256605210039,94.7186151794253));
#31962=CARTESIAN_POINT('Ctrl Pts',(6.7395267607689,0.633728733321958,94.7268273236677));
#31963=CARTESIAN_POINT('Ctrl Pts',(6.71867825379905,0.807249355483022,94.7350394679102));
#31964=CARTESIAN_POINT('Ctrl Pts',(6.69802007071979,0.979185925608369,94.7431766443266));
#31965=CARTESIAN_POINT('Ctrl Pts',(6.67077455549188,1.15018793875211,94.7513138207431));
#31966=CARTESIAN_POINT('Ctrl Pts',(6.63706529048717,1.31971714007605,94.7594509971595));
#31967=CARTESIAN_POINT('Ctrl Pts',(6.60289018017261,1.49158915081183,94.7677006253149));
#31968=CARTESIAN_POINT('Ctrl Pts',(6.56207145162975,1.66194696293157,94.7759502534704));
#31969=CARTESIAN_POINT('Ctrl Pts',(6.51478972345904,1.83024693938072,94.7841998816258));
#31970=CARTESIAN_POINT('Ctrl Pts',(6.46750799528837,1.99854691582974,94.7924495097812));
#31971=CARTESIAN_POINT('Ctrl Pts',(6.41376344604637,2.16478870994882,94.8006991379366));
#31972=CARTESIAN_POINT('Ctrl Pts',(6.35378652268395,2.32845137895552,94.808948766092));
#31973=CARTESIAN_POINT('Ctrl Pts',(6.29397854994596,2.49165302214472,94.8171751556458));
#31974=CARTESIAN_POINT('Ctrl Pts',(6.22779462444683,2.65277802842965,94.8254015451996));
#31975=CARTESIAN_POINT('Ctrl Pts',(6.1553978770005,2.81129258097013,94.8336279347534));
#31976=CARTESIAN_POINT('Ctrl Pts',(6.08308532859357,2.96962277753435,94.8418447568319));
#31977=CARTESIAN_POINT('Ctrl Pts',(6.00457449590004,3.12534824290175,94.8500615789103));
#31978=CARTESIAN_POINT('Ctrl Pts',(5.92007781878808,3.2779517414833,94.8582784009887));
#31979=CARTESIAN_POINT('Ctrl Pts',(5.83567988021109,3.43037691534964,94.8664856213052));
#31980=CARTESIAN_POINT('Ctrl Pts',(5.74531021133635,3.57968708163405,94.8746928416218));
#31981=CARTESIAN_POINT('Ctrl Pts',(5.64922859225456,3.72538659905969,94.8829000619383));
#31982=CARTESIAN_POINT('Ctrl Pts',(5.553211520259,3.87098823637669,94.8911017686909));
#31983=CARTESIAN_POINT('Ctrl Pts',(5.45149033534239,4.01298375647365,94.8993034754434));
#31984=CARTESIAN_POINT('Ctrl Pts',(5.34437011223514,4.1509031671972,94.9075051821959));
#31985=CARTESIAN_POINT('Ctrl Pts',(5.23730236092207,4.28875501944559,94.9157028714225));
#31986=CARTESIAN_POINT('Ctrl Pts',(5.12484105804399,4.42253445618407,94.9239005606492));
#31987=CARTESIAN_POINT('Ctrl Pts',(5.007333890578,4.5518014355054,94.9320982498758));
#31988=CARTESIAN_POINT('Ctrl Pts',(4.88986290332839,4.68102861378834,94.9402934150508));
#31989=CARTESIAN_POINT('Ctrl Pts',(4.76734938775491,4.80574583753666,94.9484885802256));
#31990=CARTESIAN_POINT('Ctrl Pts',(4.64018054396985,4.92554702742382,94.9566837454005));
#31991=CARTESIAN_POINT('Ctrl Pts',(4.51300243034254,5.04535695009568,94.9648795079536));
#31992=CARTESIAN_POINT('Ctrl Pts',(4.38116856654943,5.16024987153774,94.9730752705067));
#31993=CARTESIAN_POINT('Ctrl Pts',(4.24510243737961,5.26985714191131,94.9812710330598));
#31994=CARTESIAN_POINT('Ctrl Pts',(4.10903283705908,5.37946720844994,94.989467004693));
#31995=CARTESIAN_POINT('Ctrl Pts',(3.96873103887808,5.48379113414139,94.9976629763261));
#31996=CARTESIAN_POINT('Ctrl Pts',(3.82465270478567,5.58250129312799,95.0058589479594));
#31997=CARTESIAN_POINT('Ctrl Pts',(3.68049870632419,5.68126329087263,95.0140592237999));
#31998=CARTESIAN_POINT('Ctrl Pts',(3.53256450856589,5.77440543321535,95.0222594996404));
#31999=CARTESIAN_POINT('Ctrl Pts',(3.38133426050597,5.86164376422933,95.030459775481));
#32000=CARTESIAN_POINT('Ctrl Pts',(3.28848452619887,5.9152048471473,95.0354944391333));
#32001=CARTESIAN_POINT('Ctrl Pts',(3.19439287092439,5.96654136592671,95.0405291027856));
#32002=CARTESIAN_POINT('Ctrl Pts',(3.09917575053267,6.01559628526635,95.0455637664379));
#32003=CARTESIAN_POINT('Ctrl Pts',(3.09917575053244,6.01559628526647,93.0458095097322));
#32004=CARTESIAN_POINT('Ctrl Pts',(2.94385794011429,6.09561448609764,93.0540050841243));
#32005=CARTESIAN_POINT('Ctrl Pts',(2.78542189912283,6.1696224327375,93.0622006585164));
#32006=CARTESIAN_POINT('Ctrl Pts',(2.62437621248653,6.23738234320575,93.0703962329085));
#32007=CARTESIAN_POINT('Ctrl Pts',(2.46331484877174,6.30514884979872,93.0785926051032));
#32008=CARTESIAN_POINT('Ctrl Pts',(2.29964366408314,6.36666596921278,93.0867889772979));
#32009=CARTESIAN_POINT('Ctrl Pts',(2.13389102361547,6.42174416333548,93.0949853494926));
#32010=CARTESIAN_POINT('Ctrl Pts',(1.96809209102169,6.47683773993837,93.1031840108061));
#32011=CARTESIAN_POINT('Ctrl Pts',(1.80021088518807,6.52548869614646,93.1113826721197));
#32012=CARTESIAN_POINT('Ctrl Pts',(1.63079076518772,6.56755742115579,93.1195813334332));
#32013=CARTESIAN_POINT('Ctrl Pts',(1.46119433501691,6.60966992575917,93.1277885268347));
#32014=CARTESIAN_POINT('Ctrl Pts',(1.29005613971564,6.64518642674827,93.1359957202363));
#32015=CARTESIAN_POINT('Ctrl Pts',(1.1179305662884,6.67401829851838,93.1442029136379));
#32016=CARTESIAN_POINT('Ctrl Pts',(0.945714434956046,6.70286533917859,93.1524144249698));
#32017=CARTESIAN_POINT('Ctrl Pts',(0.772510245545406,6.72502069396306,93.1606259363017));
#32018=CARTESIAN_POINT('Ctrl Pts',(0.598877237411706,6.74044768947213,93.1688374476336));
#32019=CARTESIAN_POINT('Ctrl Pts',(0.424985635592444,6.75589766058744,93.1770611884662));
#32020=CARTESIAN_POINT('Ctrl Pts',(0.250664297164476,6.76459922719533,93.1852849292987));
#32021=CARTESIAN_POINT('Ctrl Pts',(0.0764735428941643,6.76656787427993,
93.1935086701312));
#32022=CARTESIAN_POINT('Ctrl Pts',(-0.094974794195755,6.76850552746012,
93.2016029383735));
#32023=CARTESIAN_POINT('Ctrl Pts',(-0.2662963084587,6.7639207858022,93.2096972066159));
#32024=CARTESIAN_POINT('Ctrl Pts',(-0.436963125906042,6.7528773294499,93.2177914748582));
#32025=CARTESIAN_POINT('Ctrl Pts',(-0.608825750804297,6.74175649515391,
93.2259424570325));
#32026=CARTESIAN_POINT('Ctrl Pts',(-0.780533533911339,6.7240529782543,93.2340934392067));
#32027=CARTESIAN_POINT('Ctrl Pts',(-0.951537045940788,6.69976613399321,
93.242244421381));
#32028=CARTESIAN_POINT('Ctrl Pts',(-1.12234192154217,6.67550750115267,93.2503859354341));
#32029=CARTESIAN_POINT('Ctrl Pts',(-1.29244379615307,6.64468081407114,93.2585274494871));
#32030=CARTESIAN_POINT('Ctrl Pts',(-1.46129448753021,6.60733739268049,93.2666689635402));
#32031=CARTESIAN_POINT('Ctrl Pts',(-1.62998457555874,6.57002949070924,93.2748027337433));
#32032=CARTESIAN_POINT('Ctrl Pts',(-1.79742549499512,6.52621727301864,93.2829365039463));
#32033=CARTESIAN_POINT('Ctrl Pts',(-1.96307543085417,6.47600369462346,93.2910702741494));
#32034=CARTESIAN_POINT('Ctrl Pts',(-2.1286026473735,6.42582731622569,93.2991980185675));
#32035=CARTESIAN_POINT('Ctrl Pts',(-2.29234117372637,6.36925912553189,93.3073257629855));
#32036=CARTESIAN_POINT('Ctrl Pts',(-2.45376062469325,6.30645286961736,93.3154535074035));
#32037=CARTESIAN_POINT('Ctrl Pts',(-2.61509442763574,6.24367993826009,93.3235769392976));
#32038=CARTESIAN_POINT('Ctrl Pts',(-2.7741112656693,6.17467566567759,93.3317003711916));
#32039=CARTESIAN_POINT('Ctrl Pts',(-2.93029713630135,6.09964324309087,93.3398238030857));
#32040=CARTESIAN_POINT('Ctrl Pts',(-3.08747378866408,6.02413484432777,93.3479987668365));
#32041=CARTESIAN_POINT('Ctrl Pts',(-3.24178307511636,5.94252166554713,93.3561737305873));
#32042=CARTESIAN_POINT('Ctrl Pts',(-3.39272232760371,5.85505971000973,93.3643486943381));
#32043=CARTESIAN_POINT('Ctrl Pts',(-3.5426760932907,5.76816879614173,93.3724702835111));
#32044=CARTESIAN_POINT('Ctrl Pts',(-3.68930339320392,5.67550546036032,93.3805918726841));
#32045=CARTESIAN_POINT('Ctrl Pts',(-3.8321370633259,5.57736627162714,93.3887134618572));
#32046=CARTESIAN_POINT('Ctrl Pts',(-3.97498959042175,5.47921412650828,93.3968361232465));
#32047=CARTESIAN_POINT('Ctrl Pts',(-4.11404718847162,5.37558489577674,93.4049587846359));
#32048=CARTESIAN_POINT('Ctrl Pts',(-4.24887279397961,5.26681772805742,93.4130814460253));
#32049=CARTESIAN_POINT('Ctrl Pts',(-4.38374187401632,5.15801548835501,93.4212067265675));
#32050=CARTESIAN_POINT('Ctrl Pts',(-4.5143759594578,5.04407224228703,93.4293320071098));
#32051=CARTESIAN_POINT('Ctrl Pts',(-4.64037214806056,4.925366517073,93.4374572876521));
#32052=CARTESIAN_POINT('Ctrl Pts',(-4.767741038993,4.80536751761509,93.4456710914398));
#32053=CARTESIAN_POINT('Ctrl Pts',(-4.89037010359729,4.68050192199052,93.4538848952275));
#32054=CARTESIAN_POINT('Ctrl Pts',(-5.00788304941987,4.55119724504807,93.4620986990153));
#32055=CARTESIAN_POINT('Ctrl Pts',(-5.12433067169839,4.42306479058494,93.4702380398704));
#32056=CARTESIAN_POINT('Ctrl Pts',(-5.23575436939067,4.29057373024794,93.4783773807256));
#32057=CARTESIAN_POINT('Ctrl Pts',(-5.34183027815121,4.15417119043342,93.4865167215808));
#32058=CARTESIAN_POINT('Ctrl Pts',(-5.44936184346608,4.01589682832268,93.4947677568348));
#32059=CARTESIAN_POINT('Ctrl Pts',(-5.55139755368367,3.87360317450173,93.5030187920888));
#32060=CARTESIAN_POINT('Ctrl Pts',(-5.64764718687912,3.72778355762997,93.5112698273428));
#32061=CARTESIAN_POINT('Ctrl Pts',(-5.7438968200745,3.58196394075833,93.5195208625968));
#32062=CARTESIAN_POINT('Ctrl Pts',(-5.83436023472334,3.43261872392146,93.5277718978508));
#32063=CARTESIAN_POINT('Ctrl Pts',(-5.91879711720737,3.28026366094826,93.5360229331049));
#32064=CARTESIAN_POINT('Ctrl Pts',(-6.00834497308961,3.11868652995183,93.5447734043927));
#32065=CARTESIAN_POINT('Ctrl Pts',(-6.09136577186997,2.95327257986616,93.5535238756804));
#32066=CARTESIAN_POINT('Ctrl Pts',(-6.16753814020142,2.78455782650691,93.5622743469682));
#32067=CARTESIAN_POINT('Ctrl Pts',(-6.24357747062115,2.61613773982212,93.5710095352282));
#32068=CARTESIAN_POINT('Ctrl Pts',(-6.31279210425957,2.44442860806013,93.5797447234881));
#32069=CARTESIAN_POINT('Ctrl Pts',(-6.37490601256228,2.26999170284767,93.588479911748));
#32070=CARTESIAN_POINT('Ctrl Pts',(-6.43931765511321,2.08910198115318,93.5975382344198));
#32071=CARTESIAN_POINT('Ctrl Pts',(-6.49609301686329,1.90527905537716,93.6065965570917));
#32072=CARTESIAN_POINT('Ctrl Pts',(-6.54497677419722,1.71917655440589,93.6156548797635));
#32073=CARTESIAN_POINT('Ctrl Pts',(-6.59192178979746,1.54045492399483,93.6243539471497));
#32074=CARTESIAN_POINT('Ctrl Pts',(-6.63158894292493,1.35963136459074,93.633053014536));
#32075=CARTESIAN_POINT('Ctrl Pts',(-6.66380078958852,1.1773054135098,93.6417520819222));
#32076=CARTESIAN_POINT('Ctrl Pts',(-6.695965293044,0.995247435126455,93.6504383638956));
#32077=CARTESIAN_POINT('Ctrl Pts',(-6.72069628556325,0.811691750617424,
93.6591246458691));
#32078=CARTESIAN_POINT('Ctrl Pts',(-6.73786647902023,0.627251393697585,
93.6678109278425));
#32079=CARTESIAN_POINT('Ctrl Pts',(-6.75500384035646,0.443163715859861,
93.6764806002734));
#32080=CARTESIAN_POINT('Ctrl Pts',(-6.76460921398091,0.258195026906238,
93.6851502727042));
#32081=CARTESIAN_POINT('Ctrl Pts',(-6.76660659767924,0.0729667886354999,
93.6938199451351));
#32082=CARTESIAN_POINT('Ctrl Pts',(-6.76686461923086,0.0490390488214526,
93.6949398913601));
#32083=CARTESIAN_POINT('Ctrl Pts',(-6.76699575324996,0.0251069907190605,
93.696059837585));
#32084=CARTESIAN_POINT('Ctrl Pts',(-6.76699989851475,0.00117196473805261,
93.6971797838099));
#32085=CARTESIAN_POINT('',(-6.76718481463439,-0.000576657417987951,93.3031400867603));
#32086=CARTESIAN_POINT('Ctrl Pts',(3.09917575053273,6.01559628526632,92.651392015122));
#32087=CARTESIAN_POINT('Ctrl Pts',(2.93382384459271,6.10078395293757,92.6601414630344));
#32088=CARTESIAN_POINT('Ctrl Pts',(2.76495772122981,6.17915010267051,92.6688909109469));
#32089=CARTESIAN_POINT('Ctrl Pts',(2.59315093316699,6.25042856433183,92.6776403588593));
#32090=CARTESIAN_POINT('Ctrl Pts',(2.42134553245594,6.3217064504146,92.6863897361193));
#32091=CARTESIAN_POINT('Ctrl Pts',(2.24659977927557,6.38589665313469,92.6951391133793));
#32092=CARTESIAN_POINT('Ctrl Pts',(2.06950718689874,6.44278115439089,92.7038884906393));
#32093=CARTESIAN_POINT('Ctrl Pts',(1.89241596572818,6.49966521519737,92.712637800154));
#32094=CARTESIAN_POINT('Ctrl Pts',(1.71297821457155,6.54924360009557,92.7213871096686));
#32095=CARTESIAN_POINT('Ctrl Pts',(1.53180337335803,6.59134792173566,92.7301364191833));
#32096=CARTESIAN_POINT('Ctrl Pts',(1.35062987477737,6.63345193135314,92.7388856638594));
#32097=CARTESIAN_POINT('Ctrl Pts',(1.16771959102902,6.66808192368247,92.7476349085355));
#32098=CARTESIAN_POINT('Ctrl Pts',(0.9836937469063,6.69512028363176,92.7563841532116));
#32099=CARTESIAN_POINT('Ctrl Pts',(0.799669205419276,6.72215845218874,92.7651333359558));
#32100=CARTESIAN_POINT('Ctrl Pts',(0.614529402872833,6.74160505424585,92.7738825187));
#32101=CARTESIAN_POINT('Ctrl Pts',(0.428903127362555,6.75339404354126,92.7826317014442));
#32102=CARTESIAN_POINT('Ctrl Pts',(0.243278104163159,6.76518295330333,92.7913808251628));
#32103=CARTESIAN_POINT('Ctrl Pts',(0.0571669005383708,6.76931433552276,
92.8001299488814));
#32104=CARTESIAN_POINT('Ctrl Pts',(-0.128798404778285,6.76577415902471,
92.8088790726));
#32105=CARTESIAN_POINT('Ctrl Pts',(-0.314762517259753,6.76223400523438,
92.8176281401992));
#32106=CARTESIAN_POINT('Ctrl Pts',(-0.500580446820047,6.75102239665085,
92.8263772077984));
#32107=CARTESIAN_POINT('Ctrl Pts',(-0.685621118843031,6.73217741012493,
92.8351262753976));
#32108=CARTESIAN_POINT('Ctrl Pts',(-0.870660665414907,6.71333253821766,
92.8438752897834));
#32109=CARTESIAN_POINT('Ctrl Pts',(-1.05492267885528,6.68685441030605,92.8526243041692));
#32110=CARTESIAN_POINT('Ctrl Pts',(-1.23778137635294,6.6528329502817,92.861373318555));
#32111=CARTESIAN_POINT('Ctrl Pts',(-1.42999922978878,6.61707018861858,92.8705701289223));
#32112=CARTESIAN_POINT('Ctrl Pts',(-1.62066601233716,6.57297172934408,92.8797669392897));
#32113=CARTESIAN_POINT('Ctrl Pts',(-1.80906628500395,6.52070304311291,92.8889637496571));
#32114=CARTESIAN_POINT('Ctrl Pts',(-1.98831342545542,6.47097374915026,92.8977137473949));
#32115=CARTESIAN_POINT('Ctrl Pts',(-2.16550875896721,6.41384933989522,92.9064637451326));
#32116=CARTESIAN_POINT('Ctrl Pts',(-2.34005036714034,6.34952386240467,92.9152137428704));
#32117=CARTESIAN_POINT('Ctrl Pts',(-2.51458843547103,6.2851996894859,92.9239635631513));
#32118=CARTESIAN_POINT('Ctrl Pts',(-2.68647261718061,6.21367483971097,92.9327133834321));
#32119=CARTESIAN_POINT('Ctrl Pts',(-2.85511905908728,6.13519226743845,92.941463203713));
#32120=CARTESIAN_POINT('Ctrl Pts',(-3.02376230488879,6.0567111825294,92.9502128581715));
#32121=CARTESIAN_POINT('Ctrl Pts',(-3.18916767379896,5.97127275992637,92.9589625126301));
#32122=CARTESIAN_POINT('Ctrl Pts',(-3.35077334102777,5.87916720438002,92.9677121670886));
#32123=CARTESIAN_POINT('Ctrl Pts',(-3.51237616037348,5.78706327195655,92.976461667357));
#32124=CARTESIAN_POINT('Ctrl Pts',(-3.6701791630227,5.68829258362317,92.9852111676255));
#32125=CARTESIAN_POINT('Ctrl Pts',(-3.82364636566424,5.58319061741068,92.9939606678939));
#32126=CARTESIAN_POINT('Ctrl Pts',(-3.97711106778759,5.4780903636773,93.0027100256023));
#32127=CARTESIAN_POINT('Ctrl Pts',(-4.12623987481888,5.36665920043255,93.0114593833108));
#32128=CARTESIAN_POINT('Ctrl Pts',(-4.2705262821389,5.24927559512367,93.0202087410192));
#32129=CARTESIAN_POINT('Ctrl Pts',(-4.41481053024929,5.13189374643078,93.0289579677957));
#32130=CARTESIAN_POINT('Ctrl Pts',(-4.55425230136472,5.00855981477405,93.0377071945722));
#32131=CARTESIAN_POINT('Ctrl Pts',(-4.68837800630482,4.8796926819214,93.0464564213488));
#32132=CARTESIAN_POINT('Ctrl Pts',(-4.82250188228811,4.75082730631893,93.0552055288196));
#32133=CARTESIAN_POINT('Ctrl Pts',(-4.95130963052868,4.6164290790363,93.0639546362904));
#32134=CARTESIAN_POINT('Ctrl Pts',(-5.07436379033255,4.47695444731816,93.0727037437613));
#32135=CARTESIAN_POINT('Ctrl Pts',(-5.19741643562673,4.33748153220743,93.081452743551));
#32136=CARTESIAN_POINT('Ctrl Pts',(-5.31471544462622,4.19293255254778,93.0902017433407));
#32137=CARTESIAN_POINT('Ctrl Pts',(-5.42586245275461,4.04379841779826,93.0989507431304));
#32138=CARTESIAN_POINT('Ctrl Pts',(-5.53702160018989,3.89464799484576,93.1077006984726));
#32139=CARTESIAN_POINT('Ctrl Pts',(-5.6420272308109,3.74091164444093,93.1164506538148));
#32140=CARTESIAN_POINT('Ctrl Pts',(-5.74052265232809,3.58311159163486,93.1252006091569));
#32141=CARTESIAN_POINT('Ctrl Pts',(-5.83901427066769,3.42531763192038,93.1339502266394));
#32142=CARTESIAN_POINT('Ctrl Pts',(-5.93099603115599,3.26346052695869,93.1426998441218));
#32143=CARTESIAN_POINT('Ctrl Pts',(-6.01615550622621,3.09809004467333,93.1514494616042));
#32144=CARTESIAN_POINT('Ctrl Pts',(-6.10131214578678,2.93272506864081,93.1601987877553));
#32145=CARTESIAN_POINT('Ctrl Pts',(-6.17964682328636,2.76384720417144,93.1689481139064));
#32146=CARTESIAN_POINT('Ctrl Pts',(-6.25089348288462,2.59203002791839,93.1776974400575));
#32147=CARTESIAN_POINT('Ctrl Pts',(-6.32213814889227,2.42021765937297,93.1864465213891));
#32148=CARTESIAN_POINT('Ctrl Pts',(-6.38629508412482,2.24546640832209,93.1951956027207));
#32149=CARTESIAN_POINT('Ctrl Pts',(-6.44314639819711,2.06836976660356,93.2039446840522));
#32150=CARTESIAN_POINT('Ctrl Pts',(-6.50000285283612,1.8912571115858,93.2126945564866));
#32151=CARTESIAN_POINT('Ctrl Pts',(-6.54955227673173,1.71179891440549,93.221444428921));
#32152=CARTESIAN_POINT('Ctrl Pts',(-6.59162635926319,1.53060476278714,93.2301943013554));
#32153=CARTESIAN_POINT('Ctrl Pts',(-6.63369752055137,1.34942319164987,93.2389435662779));
#32154=CARTESIAN_POINT('Ctrl Pts',(-6.66829431424201,1.16650618643004,93.2476928312004));
#32155=CARTESIAN_POINT('Ctrl Pts',(-6.69529923745372,0.98247499762164,93.2564420961229));
#32156=CARTESIAN_POINT('Ctrl Pts',(-6.72230554731407,0.79843435918082,93.2651918103026));
#32157=CARTESIAN_POINT('Ctrl Pts',(-6.74171916496675,0.613279706243404,
93.2739415244823));
#32158=CARTESIAN_POINT('Ctrl Pts',(-6.75347414817256,0.427639953658433,
93.282691238662));
#32159=CARTESIAN_POINT('Ctrl Pts',(-6.76248837758731,0.285283364201734,
93.2894008978379));
#32160=CARTESIAN_POINT('Ctrl Pts',(-6.7669999999999,0.142641701108384,93.2961105570138));
#32161=CARTESIAN_POINT('Ctrl Pts',(-6.767,4.93710580834799E-12,93.3028202161897));
#32162=CARTESIAN_POINT('Ctrl Pts',(-6.76699943564324,-0.00276369392438207,
93.3028202161897));
#32163=CARTESIAN_POINT('Ctrl Pts',(-6.76692073666861,-0.19546083458944,
93.311844006505));
#32164=CARTESIAN_POINT('Ctrl Pts',(-6.75860706019009,-0.387883716665939,
93.3208677968202));
#32165=CARTESIAN_POINT('Ctrl Pts',(-6.74215322839483,-0.579360720833886,
93.3298915871354));
#32166=CARTESIAN_POINT('Ctrl Pts',(-6.72561737121243,-0.771792273194158,
93.3389603627103));
#32167=CARTESIAN_POINT('Ctrl Pts',(-6.70086007133121,-0.963268274798117,
93.348029138285));
#32168=CARTESIAN_POINT('Ctrl Pts',(-6.66802805393154,-1.15312222768533,
93.3570979138599));
#32169=CARTESIAN_POINT('Ctrl Pts',(-6.63511598923357,-1.34343906093151,
93.366188799894));
#32170=CARTESIAN_POINT('Ctrl Pts',(-6.59408989033998,-1.53212572130063,
93.375279685928));
#32171=CARTESIAN_POINT('Ctrl Pts',(-6.54514676617052,-1.71852925761759,
93.3843705719621));
#32172=CARTESIAN_POINT('Ctrl Pts',(-6.49602927726239,-1.90559687503779,
93.3934938451802));
#32173=CARTESIAN_POINT('Ctrl Pts',(-6.43893835629684,-2.09036486917792,
93.4026171183984));
#32174=CARTESIAN_POINT('Ctrl Pts',(-6.37412106298803,-2.27219490237356,
93.4117403916164));
#32175=CARTESIAN_POINT('Ctrl Pts',(-6.32111453265114,-2.42089255200888,
93.4192012563629));
#32176=CARTESIAN_POINT('Ctrl Pts',(-6.26294175426668,-2.56762573814302,
93.4266621211093));
#32177=CARTESIAN_POINT('Ctrl Pts',(-6.19976076501379,-2.71205742133084,
93.4341229858557));
#32178=CARTESIAN_POINT('Ctrl Pts',(-6.13072231116159,-2.86987926319289,
93.442275542069));
#32179=CARTESIAN_POINT('Ctrl Pts',(-6.05554564095145,-3.02531006094246,
93.4504280982822));
#32180=CARTESIAN_POINT('Ctrl Pts',(-5.97441769268714,-3.17783294609816,
93.4585806544955));
#32181=CARTESIAN_POINT('Ctrl Pts',(-5.89338373310665,-3.33017912981451,
93.4667237657758));
#32182=CARTESIAN_POINT('Ctrl Pts',(-5.80641238994543,-3.47962378758133,
93.4748668770562));
#32183=CARTESIAN_POINT('Ctrl Pts',(-5.71373902127651,-3.6256689585154,93.4830099883365));
#32184=CARTESIAN_POINT('Ctrl Pts',(-5.62115353351799,-3.77157563677606,
93.4911453776139));
#32185=CARTESIAN_POINT('Ctrl Pts',(-5.52287697972033,-3.91408893961336,
93.4992807668912));
#32186=CARTESIAN_POINT('Ctrl Pts',(-5.41919108118185,-4.05273451210897,
93.5074161561685));
#32187=CARTESIAN_POINT('Ctrl Pts',(-5.31558171967864,-4.19127774165127,
93.5155455402071));
#32188=CARTESIAN_POINT('Ctrl Pts',(-5.20657118215975,-4.32595863416734,
93.5236749242457));
#32189=CARTESIAN_POINT('Ctrl Pts',(-5.09248503410837,-4.45633090977121,
93.5318043082843));
#32190=CARTESIAN_POINT('Ctrl Pts',(-4.97845913661793,-4.58663433387233,
93.5399293990764));
#32191=CARTESIAN_POINT('Ctrl Pts',(-4.85936320713057,-4.7126333982141,93.5480544898686));
#32192=CARTESIAN_POINT('Ctrl Pts',(-4.7355636994504,-4.83391409195981,93.5561795806607));
#32193=CARTESIAN_POINT('Ctrl Pts',(-4.6112916222113,-4.95565774040562,93.5643356866858));
#32194=CARTESIAN_POINT('Ctrl Pts',(-4.4822802159272,-5.07264663169301,93.572491792711));
#32195=CARTESIAN_POINT('Ctrl Pts',(-4.34893856883504,-5.18449827124082,
93.5806478987361));
#32196=CARTESIAN_POINT('Ctrl Pts',(-4.21613359775723,-5.29589972816813,
93.5887711779095));
#32197=CARTESIAN_POINT('Ctrl Pts',(-4.07903347406898,-5.40220498938928,
93.5968944570829));
#32198=CARTESIAN_POINT('Ctrl Pts',(-3.93807637029669,-5.50307582191185,
93.6050177362563));
#32199=CARTESIAN_POINT('Ctrl Pts',(-3.79710049689509,-5.60396008623804,
93.613142097113));
#32200=CARTESIAN_POINT('Ctrl Pts',(-3.65226691796216,-5.69940826759409,
93.6212664579697));
#32201=CARTESIAN_POINT('Ctrl Pts',(-3.50404357691585,-5.78912494346726,
93.6293908188264));
#32202=CARTESIAN_POINT('Ctrl Pts',(-3.35577229842576,-5.87887063493322,
93.6375178072118));
#32203=CARTESIAN_POINT('Ctrl Pts',(-3.20410938755046,-5.96288094038789,
93.6456447955972));
#32204=CARTESIAN_POINT('Ctrl Pts',(-3.04954816703763,-6.04090597318957,
93.6537717839827));
#32205=CARTESIAN_POINT('Ctrl Pts',(-2.89398772583128,-6.11943542894502,
93.6619513124227));
#32206=CARTESIAN_POINT('Ctrl Pts',(-2.73549170607932,-6.19190178616823,
93.6701308408628));
#32207=CARTESIAN_POINT('Ctrl Pts',(-2.57458344338408,-6.25809947931899,
93.6783103693029));
#32208=CARTESIAN_POINT('Ctrl Pts',(-2.41443294957232,-6.32398542619154,
93.6864513777065));
#32209=CARTESIAN_POINT('Ctrl Pts',(-2.25189324911824,-6.38366155869766,
93.6945923861102));
#32210=CARTESIAN_POINT('Ctrl Pts',(-2.08749516385627,-6.43697544976495,
93.7027333945139));
#32211=CARTESIAN_POINT('Ctrl Pts',(-1.92193027838147,-6.49066773124564,
93.7109321829722));
#32212=CARTESIAN_POINT('Ctrl Pts',(-1.7544808950459,-6.5379070259825,93.7191309714305));
#32213=CARTESIAN_POINT('Ctrl Pts',(-1.58569885720144,-6.57859013271613,
93.7273297598887));
#32214=CARTESIAN_POINT('Ctrl Pts',(-1.41691681935687,-6.61927323944979,
93.735528548347));
#32215=CARTESIAN_POINT('Ctrl Pts',(-1.24680250385791,-6.6534001486529,93.7437273368052));
#32216=CARTESIAN_POINT('Ctrl Pts',(-1.07591179273701,-6.68092080586572,
93.7519261252635));
#32217=CARTESIAN_POINT('Ctrl Pts',(-0.904306951495498,-6.70855646833614,
93.7601591753955));
#32218=CARTESIAN_POINT('Ctrl Pts',(-0.731385791230929,-6.72961657496667,
93.7683922255275));
#32219=CARTESIAN_POINT('Ctrl Pts',(-0.557693213700642,-6.74398007703109,
93.7766252756595));
#32220=CARTESIAN_POINT('Ctrl Pts',(-0.384207477330789,-6.75832647437245,
93.7848485214944));
#32221=CARTESIAN_POINT('Ctrl Pts',(-0.209952506395458,-6.76599211737185,
93.7930717673292));
#32222=CARTESIAN_POINT('Ctrl Pts',(-0.0354831671871846,-6.76690697031121,
93.8012950131641));
#32223=CARTESIAN_POINT('Ctrl Pts',(0.138813326271391,-6.76782091691113,
93.8095101122776));
#32224=CARTESIAN_POINT('Ctrl Pts',(0.313323409343689,-6.76199739075653,
93.8177252113911));
#32225=CARTESIAN_POINT('Ctrl Pts',(0.48748722261307,-6.7494181384612,93.8259403105046));
#32226=CARTESIAN_POINT('Ctrl Pts',(0.661513339485855,-6.73684883150227,
93.8341489146435));
#32227=CARTESIAN_POINT('Ctrl Pts',(0.835193376198719,-6.71753446263811,
93.8423575187824));
#32228=CARTESIAN_POINT('Ctrl Pts',(1.00796750380458,-6.69150883667309,93.8505661229212));
#32229=CARTESIAN_POINT('Ctrl Pts',(1.18063959336153,-6.66549858108864,93.8587698791702));
#32230=CARTESIAN_POINT('Ctrl Pts',(1.35240648640268,-6.63278501759715,93.8669736354192));
#32231=CARTESIAN_POINT('Ctrl Pts',(1.5227134110507,-6.5934537890097,93.8751773916682));
#32232=CARTESIAN_POINT('Ctrl Pts',(1.69296994617221,-6.55413419754146,93.8833787206324));
#32233=CARTESIAN_POINT('Ctrl Pts',(1.86176702394338,-6.50820091797749,93.8915800495967));
#32234=CARTESIAN_POINT('Ctrl Pts',(2.02855975576241,-6.45579075848197,93.899781378561));
#32235=CARTESIAN_POINT('Ctrl Pts',(2.19532948527123,-6.40338782684784,93.9079815764837));
#32236=CARTESIAN_POINT('Ctrl Pts',(2.36009507742931,-6.34450990087382,93.9161817744064));
#32237=CARTESIAN_POINT('Ctrl Pts',(2.52232648966835,-6.27934376185262,93.9243819723291));
#32238=CARTESIAN_POINT('Ctrl Pts',(2.68456492827967,-6.21417480043378,93.9325825254089));
#32239=CARTESIAN_POINT('Ctrl Pts',(2.84426863580239,-6.14271721688352,93.9407830784887));
#32240=CARTESIAN_POINT('Ctrl Pts',(3.00092719746958,-6.06520609340585,93.9489836315686));
#32241=CARTESIAN_POINT('Ctrl Pts',(3.1576209337445,-5.98767756632549,93.9571860259218));
#32242=CARTESIAN_POINT('Ctrl Pts',(3.31126784130981,-5.90409295102151,93.965388420275));
#32243=CARTESIAN_POINT('Ctrl Pts',(3.46138172439311,-5.81473348985467,93.9735908146282));
#32244=CARTESIAN_POINT('Ctrl Pts',(3.61163599034558,-5.72529046188315,93.9818008796621));
#32245=CARTESIAN_POINT('Ctrl Pts',(3.75835032243735,-5.63006198181099,93.9900109446959));
#32246=CARTESIAN_POINT('Ctrl Pts',(3.90106637958895,-5.52937339144688,93.9982210097297));
#32247=CARTESIAN_POINT('Ctrl Pts',(4.0438507381137,-5.42863661330965,94.006435003955));
#32248=CARTESIAN_POINT('Ctrl Pts',(4.18263272211037,-5.32243473237826,94.0146489981803));
#32249=CARTESIAN_POINT('Ctrl Pts',(4.31698684499628,-5.21113361756624,94.0228629924056));
#32250=CARTESIAN_POINT('Ctrl Pts',(4.45152413729963,-5.09968076226482,94.0310881850408));
#32251=CARTESIAN_POINT('Ctrl Pts',(4.58162123725197,-4.9831150186645,94.039313377676));
#32252=CARTESIAN_POINT('Ctrl Pts',(4.7068884383998,-4.86184021009107,94.0475385703112));
#32253=CARTESIAN_POINT('Ctrl Pts',(4.81954096409286,-4.75277803448919,94.0549354684311));
#32254=CARTESIAN_POINT('Ctrl Pts',(4.92828775431794,-4.63990808496353,94.0623323665511));
#32255=CARTESIAN_POINT('Ctrl Pts',(5.03287358499152,-4.52354644913641,94.0697292646711));
#32256=CARTESIAN_POINT('Ctrl Pts',(5.15512017711148,-4.38753554458314,94.078375231162));
#32257=CARTESIAN_POINT('Ctrl Pts',(5.27195899930973,-4.24644513036207,94.0870211976529));
#32258=CARTESIAN_POINT('Ctrl Pts',(5.3829705552559,-4.10072152203098,94.0956671641438));
#32259=CARTESIAN_POINT('Ctrl Pts',(5.49384011233034,-3.9551843140056,94.1043020712681));
#32260=CARTESIAN_POINT('Ctrl Pts',(5.59889708268893,-3.8050259710503,94.1129369783925));
#32261=CARTESIAN_POINT('Ctrl Pts',(5.69776096585244,-3.65072718454943,94.1215718855169));
#32262=CARTESIAN_POINT('Ctrl Pts',(5.79990705014212,-3.49130580287416,94.1304934645884));
#32263=CARTESIAN_POINT('Ctrl Pts',(5.89544153356701,-3.32746455336801,94.1394150436598));
#32264=CARTESIAN_POINT('Ctrl Pts',(5.98399032744266,-3.15977036524377,94.1483366227313));
#32265=CARTESIAN_POINT('Ctrl Pts',(6.06945713552447,-2.99791285860198,94.156947681707));
#32266=CARTESIAN_POINT('Ctrl Pts',(6.14841614237943,-2.83246638633334,94.1655587406827));
#32267=CARTESIAN_POINT('Ctrl Pts',(6.22057492005191,-2.66397009443071,94.1741697996584));
#32268=CARTESIAN_POINT('Ctrl Pts',(6.29266564866576,-2.49563270231018,94.182772738008));
#32269=CARTESIAN_POINT('Ctrl Pts',(6.35796881414188,-2.3242515041962,94.1913756763575));
#32270=CARTESIAN_POINT('Ctrl Pts',(6.41623844991414,-2.15038907034132,94.1999786147071));
#32271=CARTESIAN_POINT('Ctrl Pts',(6.47444283717413,-1.97672132219192,94.2085719197558));
#32272=CARTESIAN_POINT('Ctrl Pts',(6.5256293102815,-1.800578169687,94.2171652248046));
#32273=CARTESIAN_POINT('Ctrl Pts',(6.56960038783988,-1.62254113787422,94.2257585298533));
#32274=CARTESIAN_POINT('Ctrl Pts',(6.57449948561295,-1.60270489836153,94.2267159646938));
#32275=CARTESIAN_POINT('Ctrl Pts',(6.57930906415589,-1.58284516773862,94.2276733995343));
#32276=CARTESIAN_POINT('Ctrl Pts',(6.58402888803372,-1.56296276396384,94.2286308343748));
#32277=CARTESIAN_POINT('Ctrl Pts',(6.6264030110611,-1.38446046272552,94.2372265919223));
#32278=CARTESIAN_POINT('Ctrl Pts',(6.66148888606537,-1.20433869060862,94.2458223494699));
#32279=CARTESIAN_POINT('Ctrl Pts',(6.68919571236195,-1.02320561067585,94.2544181070175));
#32280=CARTESIAN_POINT('Ctrl Pts',(6.71692839006948,-0.841903527421079,
94.2630218846991));
#32281=CARTESIAN_POINT('Ctrl Pts',(6.73726823038795,-0.659588554715393,
94.2716256623807));
#32282=CARTESIAN_POINT('Ctrl Pts',(6.75017631614964,-0.47687388363436,94.2802294400623));
#32283=CARTESIAN_POINT('Ctrl Pts',(6.76359170096919,-0.286978366205748,
94.2891713537304));
#32284=CARTESIAN_POINT('Ctrl Pts',(6.76897935589969,-0.0966514746789712,
94.2981132673984));
#32285=CARTESIAN_POINT('Ctrl Pts',(6.76635512778851,0.0934199371131073,
94.3070551810665));
#32286=CARTESIAN_POINT('Ctrl Pts',(6.76382325958695,0.276801770990058,94.3156823833972));
#32287=CARTESIAN_POINT('Ctrl Pts',(6.75383391928934,0.459945508383227,94.3243095857279));
#32288=CARTESIAN_POINT('Ctrl Pts',(6.73645427998343,0.642240401791198,94.3329367880586));
#32289=CARTESIAN_POINT('Ctrl Pts',(6.71905808923127,0.824708903182535,94.341572206479));
#32290=CARTESIAN_POINT('Ctrl Pts',(6.69425758892832,1.00632664457754,94.3502076248994));
#32291=CARTESIAN_POINT('Ctrl Pts',(6.66217129853548,1.18649171466561,94.3588430433199));
#32292=CARTESIAN_POINT('Ctrl Pts',(6.63003760521888,1.36692295298242,94.367491219341));
#32293=CARTESIAN_POINT('Ctrl Pts',(6.59059667366888,1.54589693265643,94.3761393953621));
#32294=CARTESIAN_POINT('Ctrl Pts',(6.54401757759243,1.72282411875424,94.3847875713833));
#32295=CARTESIAN_POINT('Ctrl Pts',(6.539089685841,1.74154234419046,94.3857025156151));
#32296=CARTESIAN_POINT('Ctrl Pts',(6.53408194301536,1.76023767644184,94.386617459847));
#32297=CARTESIAN_POINT('Ctrl Pts',(6.52899458127401,1.77890942931186,94.3875324040788));
#32298=CARTESIAN_POINT('Ctrl Pts',(6.48325069878245,1.94679968611338,94.3957592814969));
#32299=CARTESIAN_POINT('Ctrl Pts',(6.43096677510618,2.11314476249537,94.4039861589149));
#32300=CARTESIAN_POINT('Ctrl Pts',(6.37226362387557,2.27739880298383,94.412213036333));
#32301=CARTESIAN_POINT('Ctrl Pts',(6.31362342555486,2.44147669841715,94.4204310912968));
#32302=CARTESIAN_POINT('Ctrl Pts',(6.24857782899537,2.6034676890307,94.4286491462605));
#32303=CARTESIAN_POINT('Ctrl Pts',(6.17729809685386,2.76283861682251,94.4368672012242));
#32304=CARTESIAN_POINT('Ctrl Pts',(6.10608054068996,2.92207052833379,94.4450780877323));
#32305=CARTESIAN_POINT('Ctrl Pts',(6.02863982598939,3.07868660391034,94.4532889742403));
#32306=CARTESIAN_POINT('Ctrl Pts',(5.94519623557328,3.23217120841785,94.4614998607483));
#32307=CARTESIAN_POINT('Ctrl Pts',(5.86181360996178,3.38554367538576,94.4697047482924));
#32308=CARTESIAN_POINT('Ctrl Pts',(5.77243701925507,3.53578891695613,94.4779096358365));
#32309=CARTESIAN_POINT('Ctrl Pts',(5.6773338210649,3.68241356778305,94.4861145233806));
#32310=CARTESIAN_POINT('Ctrl Pts',(5.58226883254748,3.82897930913024,94.4943161144417));
#32311=CARTESIAN_POINT('Ctrl Pts',(5.4814820127794,3.97192705648257,94.5025177055029));
#32312=CARTESIAN_POINT('Ctrl Pts',(5.37528555289648,4.11078997576164,94.510719296564));
#32313=CARTESIAN_POINT('Ctrl Pts',(5.26911251457786,4.24962226890877,94.5189190787693));
#32314=CARTESIAN_POINT('Ctrl Pts',(5.15753243013563,4.38437124418564,94.5271188609746));
#32315=CARTESIAN_POINT('Ctrl Pts',(5.04089955210063,4.51460083569209,94.5353186431798));
#32316=CARTESIAN_POINT('Ctrl Pts',(4.92427126168953,4.64482530476311,94.5435181028558));
#32317=CARTESIAN_POINT('Ctrl Pts',(4.80259081330919,4.7705304781173,94.5517175625319));
#32318=CARTESIAN_POINT('Ctrl Pts',(4.67625133983461,4.89131499769694,94.5599170222079));
#32319=CARTESIAN_POINT('Ctrl Pts',(4.54984956301961,5.01215908123418,94.5681205253844));
#32320=CARTESIAN_POINT('Ctrl Pts',(4.41878442857251,5.1280774136718,94.5763240285609));
#32321=CARTESIAN_POINT('Ctrl Pts',(4.28348484926054,5.23870657187014,94.5845275317374));
#32322=CARTESIAN_POINT('Ctrl Pts',(4.14815093231874,5.34936380660134,94.5927331168779));
#32323=CARTESIAN_POINT('Ctrl Pts',(4.00858071140653,5.45472897168289,94.6009387020185));
#32324=CARTESIAN_POINT('Ctrl Pts',(3.86523446916498,5.55448030857784,94.609144287159));
#32325=CARTESIAN_POINT('Ctrl Pts',(3.72175727671629,5.65432277069536,94.6173573682971));
#32326=CARTESIAN_POINT('Ctrl Pts',(3.57449747044358,5.748540961385,94.6255704494351));
#32327=CARTESIAN_POINT('Ctrl Pts',(3.42394318831687,5.83685720599524,94.6337835305731));
#32328=CARTESIAN_POINT('Ctrl Pts',(3.31728028784536,5.89942644464998,94.6396022362494));
#32329=CARTESIAN_POINT('Ctrl Pts',(3.20896436658928,5.95903427537873,94.6454209419256));
#32330=CARTESIAN_POINT('Ctrl Pts',(3.09917575053252,6.01559628526642,94.6512396476019));
#32331=CARTESIAN_POINT('Origin',(0.,0.,-3.69717978381041));
#32332=CARTESIAN_POINT('',(3.09917575053274,6.01559628526631,97.0457515827422));
#32333=CARTESIAN_POINT('',(3.09917575053247,6.01559628526645,96.651556635143));
#32334=CARTESIAN_POINT('',(3.09917575053259,6.01559628526639,-3.69717978381041));
#32335=CARTESIAN_POINT('',(-6.767,5.25699960180013E-12,95.6971797838099));
#32336=CARTESIAN_POINT('Ctrl Pts',(-6.767,5.25699960145695E-12,95.6971797838099));
#32337=CARTESIAN_POINT('Ctrl Pts',(-6.76700000000015,-0.186007249410409,
95.7059292956159));
#32338=CARTESIAN_POINT('Ctrl Pts',(-6.75932637295467,-0.372014355522253,
95.7146788074218));
#32339=CARTESIAN_POINT('Ctrl Pts',(-6.74400518266972,-0.557389537149768,
95.7234283192278));
#32340=CARTESIAN_POINT('Ctrl Pts',(-6.72868405709704,-0.742763935806127,
95.7321777940783));
#32341=CARTESIAN_POINT('Ctrl Pts',(-6.70571545653064,-0.927506129689783,
95.7409272689288));
#32342=CARTESIAN_POINT('Ctrl Pts',(-6.67517739415737,-1.11098863924453,
95.7496767437794));
#32343=CARTESIAN_POINT('Ctrl Pts',(-6.64463945823168,-1.29447038906155,
95.7584261824014));
#32344=CARTESIAN_POINT('Ctrl Pts',(-6.60653217027232,-1.47669218227882,
95.7671756210234));
#32345=CARTESIAN_POINT('Ctrl Pts',(-6.56098496116793,-1.65703510503799,
95.7759250596454));
#32346=CARTESIAN_POINT('Ctrl Pts',(-6.51543793687604,-1.83737729603714,
95.7846744627656));
#32347=CARTESIAN_POINT('Ctrl Pts',(-6.4624511220273,-2.01584035396762,95.7934238658858));
#32348=CARTESIAN_POINT('Ctrl Pts',(-6.40220448416337,-2.19181813637868,
95.8021732690061));
#32349=CARTESIAN_POINT('Ctrl Pts',(-6.34195808575295,-2.36779521935654,
95.8109226373513));
#32350=CARTESIAN_POINT('Ctrl Pts',(-6.27445201489357,-2.54128677544523,
95.8196720056966));
#32351=CARTESIAN_POINT('Ctrl Pts',(-6.19991555136322,-2.71170355237524,
95.8284213740418));
#32352=CARTESIAN_POINT('Ctrl Pts',(-6.12537937789186,-2.88211966612758,
95.8371707083389));
#32353=CARTESIAN_POINT('Ctrl Pts',(-6.04381298133773,-3.04946076210134,
95.845920042636));
#32354=CARTESIAN_POINT('Ctrl Pts',(-5.95549339426472,-3.21315848206548,
95.854669376933));
#32355=CARTESIAN_POINT('Ctrl Pts',(-5.86717414355334,-3.37685557859334,
95.8634186779086));
#32356=CARTESIAN_POINT('Ctrl Pts',(-5.7721018898642,-3.53690907467015,95.8721679788841));
#32357=CARTESIAN_POINT('Ctrl Pts',(-5.67059953467257,-3.69277536784614,
95.8809172798597));
#32358=CARTESIAN_POINT('Ctrl Pts',(-5.56909755761964,-3.84864108035506,
95.8896665482405));
#32359=CARTESIAN_POINT('Ctrl Pts',(-5.46116568338277,-4.00031938103997,
95.8984158166212));
#32360=CARTESIAN_POINT('Ctrl Pts',(-5.3471704868633,-4.1472951166294,95.907165085002));
#32361=CARTESIAN_POINT('Ctrl Pts',(-5.23317570555735,-4.29427031687775,
95.9159143215146));
#32362=CARTESIAN_POINT('Ctrl Pts',(-5.11311782179024,-4.43654275986878,
95.9246635580272));
#32363=CARTESIAN_POINT('Ctrl Pts',(-4.98740459172233,-4.57362924147411,
95.9334127945399));
#32364=CARTESIAN_POINT('Ctrl Pts',(-4.86169180911071,-4.71071523514187,
95.942161999911));
#32365=CARTESIAN_POINT('Ctrl Pts',(-4.73032391415695,-4.84261509316265,
95.9509112052821));
#32366=CARTESIAN_POINT('Ctrl Pts',(-4.59374707237581,-4.96888084331257,
95.9596604106532));
#32367=CARTESIAN_POINT('Ctrl Pts',(-4.45717070537706,-5.09514615452458,
95.9684095856094));
#32368=CARTESIAN_POINT('Ctrl Pts',(-4.31538563819829,-5.21577720253367,
95.9771587605656));
#32369=CARTESIAN_POINT('Ctrl Pts',(-4.16887341290985,-5.33036429028386,
95.9859079355219));
#32370=CARTESIAN_POINT('Ctrl Pts',(-4.02236168477685,-5.4449509892092,95.9946570807898));
#32371=CARTESIAN_POINT('Ctrl Pts',(-3.87112305634796,-5.5534935923851,96.0034062260577));
#32372=CARTESIAN_POINT('Ctrl Pts',(-3.71567117317098,-5.65562346102233,
96.0121553713256));
#32373=CARTESIAN_POINT('Ctrl Pts',(-3.5602198045769,-5.75775299158528,96.0209044876318));
#32374=CARTESIAN_POINT('Ctrl Pts',(-3.400555448628,-5.85346967275113,96.0296536039379));
#32375=CARTESIAN_POINT('Ctrl Pts',(-3.23722036323839,-5.94244842803324,
96.0384027202441));
#32376=CARTESIAN_POINT('Ctrl Pts',(-3.07388580496494,-6.03142689616247,
96.047151808315));
#32377=CARTESIAN_POINT('Ctrl Pts',(-2.90688079258165,-6.11366734484605,
96.0559008963859));
#32378=CARTESIAN_POINT('Ctrl Pts',(-2.73677251095083,-6.18889046787095,
96.0646499844569));
#32379=CARTESIAN_POINT('Ctrl Pts',(-2.56666476417118,-6.26411335438077,
96.0733990450191));
#32380=CARTESIAN_POINT('Ctrl Pts',(-2.39345402972569,-6.3323188435011,96.0821481055814));
#32381=CARTESIAN_POINT('Ctrl Pts',(-2.21772856474518,-6.39327529620877,
96.0908971661436));
#32382=CARTESIAN_POINT('Ctrl Pts',(-2.04200363768799,-6.45423156231913,
96.0996461999236));
#32383=CARTESIAN_POINT('Ctrl Pts',(-1.86376426620674,-6.50793874251888,
96.1083952337035));
#32384=CARTESIAN_POINT('Ctrl Pts',(-1.6836157819532,-6.5542144379596,96.1171442674835));
#32385=CARTESIAN_POINT('Ctrl Pts',(-1.50346783420542,-6.60048999558525,
96.1258932752077));
#32386=CARTESIAN_POINT('Ctrl Pts',(-1.32141106257962,-6.63933404145352,
96.1346422829319));
#32387=CARTESIAN_POINT('Ctrl Pts',(-1.13806375959802,-6.67061465526901,
96.1433912906561));
#32388=CARTESIAN_POINT('Ctrl Pts',(-0.954716987426327,-6.70189517852379,
96.152140273051));
#32389=CARTESIAN_POINT('Ctrl Pts',(-0.770079973816635,-6.72561226535752,
96.1608892554459));
#32390=CARTESIAN_POINT('Ctrl Pts',(-0.58477977055879,-6.74168536939727,
96.1696382378408));
#32391=CARTESIAN_POINT('Ctrl Pts',(-0.391490647560252,-6.75845143942357,
96.1787644185169));
#32392=CARTESIAN_POINT('Ctrl Pts',(-0.197480213110674,-6.76689975924008,
96.187890599193));
#32393=CARTESIAN_POINT('Ctrl Pts',(-0.0034653263041271,-6.76699911271707,
96.197016779869));
#32394=CARTESIAN_POINT('Ctrl Pts',(0.184486595289811,-6.76709536139791,
96.205857767399));
#32395=CARTESIAN_POINT('Ctrl Pts',(0.372442378179076,-6.75935659726804,
96.2146987549289));
#32396=CARTESIAN_POINT('Ctrl Pts',(0.559750217716033,-6.74380965729067,
96.2235397424588));
#32397=CARTESIAN_POINT('Ctrl Pts',(0.745129914451711,-6.7284227571732,96.2322897210566));
#32398=CARTESIAN_POINT('Ctrl Pts',(0.929874656308157,-6.70538772273556,
96.2410396996544));
#32399=CARTESIAN_POINT('Ctrl Pts',(1.11335688289177,-6.67478280180843,96.2497896782521));
#32400=CARTESIAN_POINT('Ctrl Pts',(1.29683723118258,-6.6441781941814,96.2585395672771));
#32401=CARTESIAN_POINT('Ctrl Pts',(1.4790548072964,-6.60600390230208,96.267289456302));
#32402=CARTESIAN_POINT('Ctrl Pts',(1.65939064804216,-6.56038959797284,96.2760393453269));
#32403=CARTESIAN_POINT('Ctrl Pts',(1.8397247026367,-6.51477574543424,96.2847891476879));
#32404=CARTESIAN_POINT('Ctrl Pts',(2.0181767812525,-6.46172209820286,96.2935389500488));
#32405=CARTESIAN_POINT('Ctrl Pts',(2.1941407234708,-6.4014088672422,96.3022887524098));
#32406=CARTESIAN_POINT('Ctrl Pts',(2.3701029813151,-6.34109621361594,96.3110384710152));
#32407=CARTESIAN_POINT('Ctrl Pts',(2.54357687926338,-6.27352420826204,96.3197881896208));
#32408=CARTESIAN_POINT('Ctrl Pts',(2.7139731778941,-6.19892237325742,96.3285379082262));
#32409=CARTESIAN_POINT('Ctrl Pts',(2.88436790206651,-6.12432122757223,96.3372875459845));
#32410=CARTESIAN_POINT('Ctrl Pts',(3.05168482125718,-6.04269049717689,96.3460371837428));
#32411=CARTESIAN_POINT('Ctrl Pts',(3.21535561996863,-5.95430745235214,96.354786821501));
#32412=CARTESIAN_POINT('Ctrl Pts',(3.37902496074761,-5.86592519481816,96.36353638132));
#32413=CARTESIAN_POINT('Ctrl Pts',(3.53904799384362,-5.77079087940546,96.3722859411391));
#32414=CARTESIAN_POINT('Ctrl Pts',(3.69488118814479,-5.66922763747353,96.3810355009581));
#32415=CARTESIAN_POINT('Ctrl Pts',(3.85071304610328,-5.56766526649401,96.3897849857455));
#32416=CARTESIAN_POINT('Ctrl Pts',(4.00235489705464,-5.45967423581082,96.398534470533));
#32417=CARTESIAN_POINT('Ctrl Pts',(4.14929168607153,-5.34562133936718,96.4072839553204));
#32418=CARTESIAN_POINT('Ctrl Pts',(4.29622726385256,-5.23156938308942,96.4160333679837));
#32419=CARTESIAN_POINT('Ctrl Pts',(4.43845763091568,-5.11145583677635,96.424782780647));
#32420=CARTESIAN_POINT('Ctrl Pts',(4.57549970660466,-4.98568866204667,96.4335321933103));
#32421=CARTESIAN_POINT('Ctrl Pts',(4.71254069814814,-4.85992248226628,96.4422815367566));
#32422=CARTESIAN_POINT('Ctrl Pts',(4.84439326930848,-4.72850295734479,96.4510308802029));
#32423=CARTESIAN_POINT('Ctrl Pts',(4.97060959434248,-4.59187644222169,96.4597802236492));
#32424=CARTESIAN_POINT('Ctrl Pts',(5.09682496280083,-4.45525096257158,96.4685295007855));
#32425=CARTESIAN_POINT('Ctrl Pts',(5.21740397615425,-4.31341878218827,96.4772787779218));
#32426=CARTESIAN_POINT('Ctrl Pts',(5.33193710451538,-4.16686161439184,96.4860280550581));
#32427=CARTESIAN_POINT('Ctrl Pts',(5.44646940289005,-4.02030550865026,96.4947772687911));
#32428=CARTESIAN_POINT('Ctrl Pts',(5.55495572749305,-3.8690247098065,96.5035264825241));
#32429=CARTESIAN_POINT('Ctrl Pts',(5.65702762491114,-3.71353301466302,96.512275696257));
#32430=CARTESIAN_POINT('Ctrl Pts',(5.75909881654828,-3.5580423946742,96.5210248494931));
#32431=CARTESIAN_POINT('Ctrl Pts',(5.85475551250472,-3.39834117620087,96.5297740027293));
#32432=CARTESIAN_POINT('Ctrl Pts',(5.94367283727801,-3.23497174692509,96.5385231559654));
#32433=CARTESIAN_POINT('Ctrl Pts',(6.03258957676034,-3.0716033930151,96.5472722516109));
#32434=CARTESIAN_POINT('Ctrl Pts',(6.11476689685024,-2.90456712830052,96.5560213472564));
#32435=CARTESIAN_POINT('Ctrl Pts',(6.18992570525017,-2.73443024476456,96.564770442902));
#32436=CARTESIAN_POINT('Ctrl Pts',(6.26508404388482,-2.56429442463559,96.573519483863));
#32437=CARTESIAN_POINT('Ctrl Pts',(6.33322384283125,-2.39105828656497,96.5822685248241));
#32438=CARTESIAN_POINT('Ctrl Pts',(6.39411368719867,-2.2153101713256,96.5910175657851));
#32439=CARTESIAN_POINT('Ctrl Pts',(6.45500317120736,-2.03956309620002,96.5997665549675));
#32440=CARTESIAN_POINT('Ctrl Pts',(6.50864269269932,-1.86130434439128,96.6085155441499));
#32441=CARTESIAN_POINT('Ctrl Pts',(6.55485008446205,-1.68113930720447,96.6172645333323));
#32442=CARTESIAN_POINT('Ctrl Pts',(6.6019966474929,-1.49731239212341,96.6261913468617));
#32443=CARTESIAN_POINT('Ctrl Pts',(6.64140563640808,-1.3115011650017,96.6351181603911));
#32444=CARTESIAN_POINT('Ctrl Pts',(6.67293772282089,-1.12436255156156,96.6440449739204));
#32445=CARTESIAN_POINT('Ctrl Pts',(6.703844949498,-0.940932395056388,96.652794888076));
#32446=CARTESIAN_POINT('Ctrl Pts',(6.72718449348872,-0.756227260511841,
96.6615448022315));
#32447=CARTESIAN_POINT('Ctrl Pts',(6.74287707373888,-0.570874564546893,
96.670294716387));
#32448=CARTESIAN_POINT('Ctrl Pts',(6.75856934538641,-0.385525513637644,
96.679044458471));
#32449=CARTESIAN_POINT('Ctrl Pts',(6.76661493004088,-0.199529212423358,
96.687794200555));
#32450=CARTESIAN_POINT('Ctrl Pts',(6.76698649908906,-0.0135174386055113,
96.6965439426389));
#32451=CARTESIAN_POINT('Ctrl Pts',(6.76735806132402,0.172490924440769,96.7052935242848));
#32452=CARTESIAN_POINT('Ctrl Pts',(6.76005588896316,0.358514472896479,96.7140431059307));
#32453=CARTESIAN_POINT('Ctrl Pts',(6.74510478454623,0.54392135965737,96.7227926875766));
#32454=CARTESIAN_POINT('Ctrl Pts',(6.7301539344074,0.729325093145667,96.7315421204157));
#32455=CARTESIAN_POINT('Ctrl Pts',(6.70755443556962,0.914111900251644,96.7402915532547));
#32456=CARTESIAN_POINT('Ctrl Pts',(6.67738304682395,1.09765415591075,96.7490409860938));
#32457=CARTESIAN_POINT('Ctrl Pts',(6.6472121311195,1.28119353390807,96.7577902817551));
#32458=CARTESIAN_POINT('Ctrl Pts',(6.60946960955598,1.46348811672184,96.7665395774164));
#32459=CARTESIAN_POINT('Ctrl Pts',(6.56428366991301,1.64391876347752,96.7752888730777));
#32460=CARTESIAN_POINT('Ctrl Pts',(6.51909837867849,1.82434682109246,96.7840380431886));
#32461=CARTESIAN_POINT('Ctrl Pts',(6.46646995272066,2.00291071819976,96.7927872132994));
#32462=CARTESIAN_POINT('Ctrl Pts',(6.40657713281708,2.17900400212236,96.8015363834102));
#32463=CARTESIAN_POINT('Ctrl Pts',(6.34668509279232,2.35509499309194,96.810285439596));
#32464=CARTESIAN_POINT('Ctrl Pts',(6.27952894037711,2.52871516397663,96.8190344957818));
#32465=CARTESIAN_POINT('Ctrl Pts',(6.20533675061645,2.69927486770964,96.8277835519675));
#32466=CARTESIAN_POINT('Ctrl Pts',(6.12832117908122,2.87632521635486,96.8368655532498));
#32467=CARTESIAN_POINT('Ctrl Pts',(6.04372366626291,3.05007728919579,96.8459475545321));
#32468=CARTESIAN_POINT('Ctrl Pts',(5.95185378008084,3.21989527477796,96.8550295558144));
#32469=CARTESIAN_POINT('Ctrl Pts',(5.86334450817601,3.38350129286353,96.8637793361215));
#32470=CARTESIAN_POINT('Ctrl Pts',(5.76808562057499,3.54345567124565,96.8725291164286));
#32471=CARTESIAN_POINT('Ctrl Pts',(5.66640068804741,3.69921508464916,96.8812788967357));
#32472=CARTESIAN_POINT('Ctrl Pts',(5.56471941108188,3.85496889851902,96.8900283624892));
#32473=CARTESIAN_POINT('Ctrl Pts',(5.45661270815385,4.00652780919267,96.8987778282427));
#32474=CARTESIAN_POINT('Ctrl Pts',(5.34244776449392,4.15337704568872,96.9075272939962));
#32475=CARTESIAN_POINT('Ctrl Pts',(5.22828631819892,4.30022178355889,96.9162764917158));
#32476=CARTESIAN_POINT('Ctrl Pts',(5.10806717844385,4.44235690972315,96.9250256894354));
#32477=CARTESIAN_POINT('Ctrl Pts',(4.98219864545055,4.5792996907028,96.933774887155));
#32478=CARTESIAN_POINT('Ctrl Pts',(4.85633329944363,4.71623900429653,96.9425238633452));
#32479=CARTESIAN_POINT('Ctrl Pts',(4.72481904033988,4.84798602483286,96.9512728395354));
#32480=CARTESIAN_POINT('Ctrl Pts',(4.58810250737539,4.97409332258812,96.9600218157257));
#32481=CARTESIAN_POINT('Ctrl Pts',(4.45137708685986,5.10020881821835,96.9687713606619));
#32482=CARTESIAN_POINT('Ctrl Pts',(4.30944892636398,5.22068366307647,96.9775209055981));
#32483=CARTESIAN_POINT('Ctrl Pts',(4.16280009467009,5.33510865604578,96.9862704505342));
#32484=CARTESIAN_POINT('Ctrl Pts',(4.01615988349162,5.44952692272616,96.9950194811425));
#32485=CARTESIAN_POINT('Ctrl Pts',(3.86479978232629,5.55789587288348,97.0037685117508));
#32486=CARTESIAN_POINT('Ctrl Pts',(3.70923383581492,5.659847467136,97.012517542359));
#32487=CARTESIAN_POINT('Ctrl Pts',(3.55366577799975,5.76180044505114,97.0212666917071));
#32488=CARTESIAN_POINT('Ctrl Pts',(3.39389200027285,5.85733573570801,97.0300158410551));
#32489=CARTESIAN_POINT('Ctrl Pts',(3.23045513626497,5.9461288762168,97.0387649904031));
#32490=CARTESIAN_POINT('Ctrl Pts',(3.18695122151889,5.96976399206524,97.0410938545161));
#32491=CARTESIAN_POINT('Ctrl Pts',(3.14318791262828,5.99292165435248,97.0434227186292));
#32492=CARTESIAN_POINT('Ctrl Pts',(3.09917575053274,6.01559628526631,97.0457515827422));
#32493=CARTESIAN_POINT('Ctrl Pts',(3.09917575053267,6.01559628526635,95.0455637664379));
#32494=CARTESIAN_POINT('Ctrl Pts',(2.943906770375,6.09558932922995,95.0537737090146));
#32495=CARTESIAN_POINT('Ctrl Pts',(2.78564419716587,6.16951272082007,95.0619836515913));
#32496=CARTESIAN_POINT('Ctrl Pts',(2.62490874004041,6.23715825568499,95.070193594168));
#32497=CARTESIAN_POINT('Ctrl Pts',(2.46407107433121,6.30484680504367,95.0784087572891));
#32498=CARTESIAN_POINT('Ctrl Pts',(2.30075772543929,6.36624941518948,95.0866239204103));
#32499=CARTESIAN_POINT('Ctrl Pts',(2.13550538356776,6.42120749989853,95.0948390835315));
#32500=CARTESIAN_POINT('Ctrl Pts',(1.97003647291874,6.47623760903449,95.1030650129015));
#32501=CARTESIAN_POINT('Ctrl Pts',(1.80262383819817,6.52480622767291,95.1112909422715));
#32502=CARTESIAN_POINT('Ctrl Pts',(1.63381603663925,6.56680547590839,95.1195168716415));
#32503=CARTESIAN_POINT('Ctrl Pts',(1.58139506131994,6.57984777333096,95.1220713225407));
#32504=CARTESIAN_POINT('Ctrl Pts',(1.52883959571413,6.59225694302585,95.1246257734398));
#32505=CARTESIAN_POINT('Ctrl Pts',(1.47616617480197,6.60403077100422,95.127180224339));
#32506=CARTESIAN_POINT('Ctrl Pts',(1.30656773086973,6.64194026823597,95.1354050726611));
#32507=CARTESIAN_POINT('Ctrl Pts',(1.13526998503762,6.67336557312749,95.1436299209831));
#32508=CARTESIAN_POINT('Ctrl Pts',(0.962809917477377,6.69815542241349,95.1518547693052));
#32509=CARTESIAN_POINT('Ctrl Pts',(0.790544078190971,6.7229173528328,95.1600703546244));
#32510=CARTESIAN_POINT('Ctrl Pts',(0.617118875677853,6.74105865770386,95.1682859399436));
#32511=CARTESIAN_POINT('Ctrl Pts',(0.443084048288832,6.75247847283884,95.1765015252628));
#32512=CARTESIAN_POINT('Ctrl Pts',(0.269210255640676,6.76388772119821,95.184709508686));
#32513=CARTESIAN_POINT('Ctrl Pts',(0.0947283172537854,6.76858784255455,
95.1929174921093));
#32514=CARTESIAN_POINT('Ctrl Pts',(-0.0798041992942283,6.76652941246656,
95.2011254755325));
#32515=CARTESIAN_POINT('Ctrl Pts',(-0.254210276332712,6.76447247360149,
95.2093275127091));
#32516=CARTESIAN_POINT('Ctrl Pts',(-0.428666501257262,6.75566673983363,
95.2175295498856));
#32517=CARTESIAN_POINT('Ctrl Pts',(-0.602612485437827,6.7401147759066,95.2257315870622));
#32518=CARTESIAN_POINT('Ctrl Pts',(-0.77646738491674,6.72457095557656,95.2339293293416));
#32519=CARTESIAN_POINT('Ctrl Pts',(-0.949812219419549,6.70228797442919,
95.242127071621));
#32520=CARTESIAN_POINT('Ctrl Pts',(-1.12208881749832,6.67332043930495,95.2503248139004));
#32521=CARTESIAN_POINT('Ctrl Pts',(-1.29433266003202,6.6443584118783,95.2585209975147));
#32522=CARTESIAN_POINT('Ctrl Pts',(-1.46550831622571,6.60871441534547,95.2667171811291));
#32523=CARTESIAN_POINT('Ctrl Pts',(-1.63506463190266,6.56649470033298,95.2749133647434));
#32524=CARTESIAN_POINT('Ctrl Pts',(-1.80460846586917,6.52427809328054,95.2831089450043));
#32525=CARTESIAN_POINT('Ctrl Pts',(-1.97253284831188,6.47548681760763,95.2913045252652));
#32526=CARTESIAN_POINT('Ctrl Pts',(-2.13829874066011,6.42027783633165,95.2995001055261));
#32527=CARTESIAN_POINT('Ctrl Pts',(-2.30408258946872,6.36506287458604,95.3076965735667));
#32528=CARTESIAN_POINT('Ctrl Pts',(-2.46770714183432,6.30342893561063,95.3158930416074));
#32529=CARTESIAN_POINT('Ctrl Pts',(-2.62865034699279,6.23558227860516,95.3240895096481));
#32530=CARTESIAN_POINT('Ctrl Pts',(-2.78964026803451,6.16771592821465,95.3322883568215));
#32531=CARTESIAN_POINT('Ctrl Pts',(-2.94794696103396,6.09363340715741,95.3404872039949));
#32532=CARTESIAN_POINT('Ctrl Pts',(-3.10307006934435,6.01358837506686,95.3486860511683));
#32533=CARTESIAN_POINT('Ctrl Pts',(-3.25835529638719,5.93345968813414,95.3568934669343));
#32534=CARTESIAN_POINT('Ctrl Pts',(-3.41044997221247,5.84735620540302,95.3651008827003));
#32535=CARTESIAN_POINT('Ctrl Pts',(-3.55887912042718,5.75557715665314,95.3733082984662));
#32536=CARTESIAN_POINT('Ctrl Pts',(-3.70738782144522,5.66374891756092,95.3815201131184));
#32537=CARTESIAN_POINT('Ctrl Pts',(-3.85222678100859,5.56623924854325,95.3897319277705));
#32538=CARTESIAN_POINT('Ctrl Pts',(-3.99295167116383,5.46338960277866,95.3979437424227));
#32539=CARTESIAN_POINT('Ctrl Pts',(-4.13388380011314,5.36038849527525,95.4061676502203));
#32540=CARTESIAN_POINT('Ctrl Pts',(-4.27068947043723,5.25203191798305,95.4143915580179));
#32541=CARTESIAN_POINT('Ctrl Pts',(-4.40295800230478,5.13870118122666,95.4226154658155));
#32542=CARTESIAN_POINT('Ctrl Pts',(-4.52517168297585,5.03398567348949,95.4302142047389));
#32543=CARTESIAN_POINT('Ctrl Pts',(-4.6435120554334,4.92502408966409,95.4378129436624));
#32544=CARTESIAN_POINT('Ctrl Pts',(-4.75768487240652,4.81214335352493,95.4454116825858));
#32545=CARTESIAN_POINT('Ctrl Pts',(-4.87840941474031,4.6927850371587,95.4534464697021));
#32546=CARTESIAN_POINT('Ctrl Pts',(-4.99485389248265,4.56866854002903,95.4614812568183));
#32547=CARTESIAN_POINT('Ctrl Pts',(-5.10660816305721,4.44013987043173,95.4695160439346));
#32548=CARTESIAN_POINT('Ctrl Pts',(-5.21823051087443,4.31176292529563,95.4775413462118));
#32549=CARTESIAN_POINT('Ctrl Pts',(-5.32517342373367,4.17898445205639,95.485566648489));
#32550=CARTESIAN_POINT('Ctrl Pts',(-5.42706130152284,4.04218933617825,95.4935919507662));
#32551=CARTESIAN_POINT('Ctrl Pts',(-5.52885159927958,3.90552523168374,95.501609567053));
#32552=CARTESIAN_POINT('Ctrl Pts',(-5.62559627334275,3.76485243981903,95.5096271833397));
#32553=CARTESIAN_POINT('Ctrl Pts',(-5.71695805868633,3.62059105053601,95.5176447996264));
#32554=CARTESIAN_POINT('Ctrl Pts',(-5.80824657868332,3.47644534814162,95.5256559863821));
#32555=CARTESIAN_POINT('Ctrl Pts',(-5.89416060514533,3.32871709553155,95.5336671731378));
#32556=CARTESIAN_POINT('Ctrl Pts',(-5.97440465955954,3.17785744863317,95.5416783598935));
#32557=CARTESIAN_POINT('Ctrl Pts',(-6.05461363157628,3.02706375700254,95.5496860441886));
#32558=CARTESIAN_POINT('Ctrl Pts',(-6.1291573868748,2.87314172643022,95.5576937284837));
#32559=CARTESIAN_POINT('Ctrl Pts',(-6.19778506576384,2.71656939513695,95.5657014127788));
#32560=CARTESIAN_POINT('Ctrl Pts',(-6.26639652982033,2.56003405757821,95.5737072050784));
#32561=CARTESIAN_POINT('Ctrl Pts',(-6.32909454842009,2.40085001021319,95.581712997378));
#32562=CARTESIAN_POINT('Ctrl Pts',(-6.38567540637297,2.23951749366766,95.5897187896776));
#32563=CARTESIAN_POINT('Ctrl Pts',(-6.44225426242193,2.07819068527514,95.597724298722));
#32564=CARTESIAN_POINT('Ctrl Pts',(-6.49271626553911,1.91471591483534,95.6057298077663));
#32565=CARTESIAN_POINT('Ctrl Pts',(-6.53690686631789,1.74961070558169,95.6137353168106));
#32566=CARTESIAN_POINT('Ctrl Pts',(-6.58112025794606,1.58442034500872,95.6217449546141));
#32567=CARTESIAN_POINT('Ctrl Pts',(-6.61905568935104,1.41759823012135,95.6297545924177));
#32568=CARTESIAN_POINT('Ctrl Pts',(-6.65060917076422,1.2496746207501,95.6377642302212));
#32569=CARTESIAN_POINT('Ctrl Pts',(-6.68217182860439,1.0817021756031,95.6457761973987));
#32570=CARTESIAN_POINT('Ctrl Pts',(-6.70734878206237,0.912627969872602,
95.6537881645761));
#32571=CARTESIAN_POINT('Ctrl Pts',(-6.72608773376436,0.742989096625667,
95.6618001317536));
#32572=CARTESIAN_POINT('Ctrl Pts',(-6.74484382719967,0.573195043709559,
95.6698194279966));
#32573=CARTESIAN_POINT('Ctrl Pts',(-6.75715013196647,0.402835666939462,
95.6778387242395));
#32574=CARTESIAN_POINT('Ctrl Pts',(-6.7630064226757,0.232450267470704,95.6858580204825));
#32575=CARTESIAN_POINT('Ctrl Pts',(-6.7656701866882,0.15494959035367,95.6895056387102));
#32576=CARTESIAN_POINT('Ctrl Pts',(-6.76700020042621,0.0774435045898423,
95.6931532569379));
#32577=CARTESIAN_POINT('Ctrl Pts',(-6.76699999997734,-1.75112276718149E-5,
95.6968008751656));
#32578=CARTESIAN_POINT('',(-6.76699859668926,-0.00435802771595241,95.3028202161534));
#32579=CARTESIAN_POINT('Ctrl Pts',(3.09917575053252,6.01559628526642,94.6512396476019));
#32580=CARTESIAN_POINT('Ctrl Pts',(2.94401132479335,6.09553546382698,94.6594632335912));
#32581=CARTESIAN_POINT('Ctrl Pts',(2.78590477759022,6.16938874478998,94.6676868195806));
#32582=CARTESIAN_POINT('Ctrl Pts',(2.62538040155148,6.23695973589291,94.67591040557));
#32583=CARTESIAN_POINT('Ctrl Pts',(2.46463890552551,6.30462212129426,94.6841451145111));
#32584=CARTESIAN_POINT('Ctrl Pts',(2.30147338489664,6.36598512597349,94.6923798234522));
#32585=CARTESIAN_POINT('Ctrl Pts',(2.13642342298202,6.42090211401278,94.7006145323933));
#32586=CARTESIAN_POINT('Ctrl Pts',(2.10488202478951,6.431396867039,94.7021882027577));
#32587=CARTESIAN_POINT('Ctrl Pts',(2.07327183631911,6.44165636140993,94.7037618731221));
#32588=CARTESIAN_POINT('Ctrl Pts',(2.04159666135396,6.45167978687321,94.7053355434865));
#32589=CARTESIAN_POINT('Ctrl Pts',(1.87744184354736,6.50362562718925,94.7134910018933));
#32590=CARTESIAN_POINT('Ctrl Pts',(1.71103543735194,6.54938703930309,94.7216464603001));
#32591=CARTESIAN_POINT('Ctrl Pts',(1.54288826862621,6.58876200742868,94.7298019187068));
#32592=CARTESIAN_POINT('Ctrl Pts',(1.37494575710755,6.62808905104228,94.7379474508487));
#32593=CARTESIAN_POINT('Ctrl Pts',(1.20526705246651,6.66104504104213,94.7460929829906));
#32594=CARTESIAN_POINT('Ctrl Pts',(1.03438091509877,6.68747673808885,94.7542385151325));
#32595=CARTESIAN_POINT('Ctrl Pts',(0.86366683469625,6.71388182234152,94.762375845933));
#32596=CARTESIAN_POINT('Ctrl Pts',(0.691748100327034,6.73377563589263,94.7705131767336));
#32597=CARTESIAN_POINT('Ctrl Pts',(0.519166526651232,6.74705529231864,94.7786505075341));
#32598=CARTESIAN_POINT('Ctrl Pts',(0.346722448441673,6.76032436886341,94.7867813553361));
#32599=CARTESIAN_POINT('Ctrl Pts',(0.173616945133653,6.766989752579,94.7949122031381));
#32600=CARTESIAN_POINT('Ctrl Pts',(0.000399870219098874,6.76699998818559,
94.8030430509401));
#32601=CARTESIAN_POINT('Ctrl Pts',(-0.172715590171761,6.76701021778766,
94.8111691289339));
#32602=CARTESIAN_POINT('Ctrl Pts',(-0.345942127238149,6.76037307423085,
94.8192952069277));
#32603=CARTESIAN_POINT('Ctrl Pts',(-0.518726947958766,6.74708910223227,
94.8274212849215));
#32604=CARTESIAN_POINT('Ctrl Pts',(-0.692124432095885,6.73375802769519,
94.8355761765037));
#32605=CARTESIAN_POINT('Ctrl Pts',(-0.86507669044076,6.71373287892692,94.8437310680859));
#32606=CARTESIAN_POINT('Ctrl Pts',(-1.0370266241599,6.68706697893654,94.8518859596681));
#32607=CARTESIAN_POINT('Ctrl Pts',(-1.20830601325809,6.66050506663267,94.8600090500244));
#32608=CARTESIAN_POINT('Ctrl Pts',(-1.3785905197743,6.6273541767211,94.8681321403806));
#32609=CARTESIAN_POINT('Ctrl Pts',(-1.5473365971255,6.58771875957042,94.8762552307369));
#32610=CARTESIAN_POINT('Ctrl Pts',(-1.7160959251891,6.54808023006584,94.8843789589554));
#32611=CARTESIAN_POINT('Ctrl Pts',(-1.88331622730901,6.50195624267316,94.8925026871738));
#32612=CARTESIAN_POINT('Ctrl Pts',(-2.04846627137669,6.44950191371645,94.9006264153922));
#32613=CARTESIAN_POINT('Ctrl Pts',(-2.21366070337928,6.39703348643265,94.9087523270525));
#32614=CARTESIAN_POINT('Ctrl Pts',(-2.37678342085705,6.33823144041911,94.9168782387128));
#32615=CARTESIAN_POINT('Ctrl Pts',(-2.53732045830639,6.27330007985111,94.9250041503731));
#32616=CARTESIAN_POINT('Ctrl Pts',(-2.69888414679854,6.20795347648245,94.9331820280832));
#32617=CARTESIAN_POINT('Ctrl Pts',(-2.85782862088997,6.13639903207623,94.9413599057933));
#32618=CARTESIAN_POINT('Ctrl Pts',(-3.01365322584842,6.05889290500611,94.9495377835033));
#32619=CARTESIAN_POINT('Ctrl Pts',(-3.16873411376371,5.98175669787045,94.9576766299768));
#32620=CARTESIAN_POINT('Ctrl Pts',(-3.32072455663284,5.89872572514541,94.9658154764502));
#32621=CARTESIAN_POINT('Ctrl Pts',(-3.46915873002406,5.81009696183273,94.9739543229237));
#32622=CARTESIAN_POINT('Ctrl Pts',(-3.61866066578788,5.7208306468267,94.9821517162521));
#32623=CARTESIAN_POINT('Ctrl Pts',(-3.76455465845203,5.6258859081452,94.9903491095805));
#32624=CARTESIAN_POINT('Ctrl Pts',(-3.90639760901627,5.52560826699396,94.9985465029089));
#32625=CARTESIAN_POINT('Ctrl Pts',(-4.04824055958042,5.42533062584278,95.0067438962373));
#32626=CARTESIAN_POINT('Ctrl Pts',(-4.18603220978262,5.31972035716278,95.0149412895657));
#32627=CARTESIAN_POINT('Ctrl Pts',(-4.31936653152684,5.20916133041834,95.0231386828941));
#32628=CARTESIAN_POINT('Ctrl Pts',(-4.45143330188874,5.09965334023632,95.0312581471708));
#32629=CARTESIAN_POINT('Ctrl Pts',(-4.57954166030533,4.98494649229571,95.0393776114476));
#32630=CARTESIAN_POINT('Ctrl Pts',(-4.70324933048561,4.86536069940212,95.0474970757243));
#32631=CARTESIAN_POINT('Ctrl Pts',(-4.82681675105671,4.74591048307133,95.0556073348185));
#32632=CARTESIAN_POINT('Ctrl Pts',(-4.94599315118097,4.6215925855464,95.0637175939127));
#32633=CARTESIAN_POINT('Ctrl Pts',(-5.06036782651735,4.49276824022207,95.0718278530068));
#32634=CARTESIAN_POINT('Ctrl Pts',(-5.17463735853119,4.36406232163556,95.0799306564332));
#32635=CARTESIAN_POINT('Ctrl Pts',(-5.28411370980808,4.23085847657609,95.0880334598595));
#32636=CARTESIAN_POINT('Ctrl Pts',(-5.38842172690336,4.0935559472219,95.0961362632859));
#32637=CARTESIAN_POINT('Ctrl Pts',(-5.49265620418498,3.95635021965445,95.104233354029));
#32638=CARTESIAN_POINT('Ctrl Pts',(-5.59172938012883,3.81505185422318,95.1123304447722));
#32639=CARTESIAN_POINT('Ctrl Pts',(-5.68530527557364,3.67009440253716,95.1204275355154));
#32640=CARTESIAN_POINT('Ctrl Pts',(-5.77883951687644,3.52520147685166,95.1285210219396));
#32641=CARTESIAN_POINT('Ctrl Pts',(-5.86688114923733,3.37665301685795,95.1366145083639));
#32642=CARTESIAN_POINT('Ctrl Pts',(-5.94913655838172,3.22491289955653,95.1447079947882));
#32643=CARTESIAN_POINT('Ctrl Pts',(-6.0313740854861,3.07320577002914,95.1527997217166));
#32644=CARTESIAN_POINT('Ctrl Pts',(-6.107827717105,2.91830868845482,95.1608914486451));
#32645=CARTESIAN_POINT('Ctrl Pts',(-6.17824901137132,2.76071153029239,95.1689831755736));
#32646=CARTESIAN_POINT('Ctrl Pts',(-6.2486686519124,2.6031180730332,95.1770747124815));
#32647=CARTESIAN_POINT('Ctrl Pts',(-6.31305608682467,2.44282500258794,95.1851662493894));
#32648=CARTESIAN_POINT('Ctrl Pts',(-6.37121042519647,2.28034355259636,95.1932577862973));
#32649=CARTESIAN_POINT('Ctrl Pts',(-6.42937467534367,2.11783440940623,95.2013507023198));
#32650=CARTESIAN_POINT('Ctrl Pts',(-6.48130359055544,1.95313649195031,95.2094436183423));
#32651=CARTESIAN_POINT('Ctrl Pts',(-6.52684571990895,1.78677753190102,95.2175365343648));
#32652=CARTESIAN_POINT('Ctrl Pts',(-6.57242486755529,1.62028334926142,95.2256360286027));
#32653=CARTESIAN_POINT('Ctrl Pts',(-6.61160676440659,1.45212578406303,95.2337355228406));
#32654=CARTESIAN_POINT('Ctrl Pts',(-6.64429065493007,1.28284476567078,95.2418350170784));
#32655=CARTESIAN_POINT('Ctrl Pts',(-6.67698945208373,1.11348654075579,95.2499382053736));
#32656=CARTESIAN_POINT('Ctrl Pts',(-6.70318428156195,0.943004205998225,
95.2580413936688));
#32657=CARTESIAN_POINT('Ctrl Pts',(-6.72282616721505,0.771943861565483,
95.266144581964));
#32658=CARTESIAN_POINT('Ctrl Pts',(-6.74249097732885,0.600683868982252,
95.2742572276619));
#32659=CARTESIAN_POINT('Ctrl Pts',(-6.75558754225939,0.42884488681141,95.2823698733597));
#32660=CARTESIAN_POINT('Ctrl Pts',(-6.76211896818731,0.25697482382795,95.2904825190576));
#32661=CARTESIAN_POINT('Ctrl Pts',(-6.76542996181808,0.169848262164658,
95.2945950847562));
#32662=CARTESIAN_POINT('Ctrl Pts',(-6.76705467190439,0.0827136769254795,
95.2987076504548));
#32663=CARTESIAN_POINT('Ctrl Pts',(-6.76699859668926,-0.00435802771576677,
95.3028202161534));
#32664=CARTESIAN_POINT('Ctrl Pts',(-6.76699859668877,-0.00435802848384897,
95.3028202161897));
#32665=CARTESIAN_POINT('Ctrl Pts',(-6.76682533277866,-0.273396342687137,
95.3155274182271));
#32666=CARTESIAN_POINT('Ctrl Pts',(-6.75060771707868,-0.541919813427472,
95.3282346202645));
#32667=CARTESIAN_POINT('Ctrl Pts',(-6.71852819966011,-0.808497266768375,
95.3409418223019));
#32668=CARTESIAN_POINT('Ctrl Pts',(-6.69776103485891,-0.981070246392114,
95.3491680233207));
#32669=CARTESIAN_POINT('Ctrl Pts',(-6.67031147402146,-1.15308377659327,
95.3573942243396));
#32670=CARTESIAN_POINT('Ctrl Pts',(-6.63621604054561,-1.3239809904999,95.3656204253584));
#32671=CARTESIAN_POINT('Ctrl Pts',(-6.60215890610328,-1.49468623740521,
95.3738373859742));
#32672=CARTESIAN_POINT('Ctrl Pts',(-6.56147083387031,-1.66427731645193,
95.38205434659));
#32673=CARTESIAN_POINT('Ctrl Pts',(-6.51424011597687,-1.83220214807146,
95.3902713072057));
#32674=CARTESIAN_POINT('Ctrl Pts',(-6.4670529722603,-1.99997205538241,95.3984806870073));
#32675=CARTESIAN_POINT('Ctrl Pts',(-6.4133353005395,-2.16607843368287,95.4066900668089));
#32676=CARTESIAN_POINT('Ctrl Pts',(-6.35322649846421,-2.32997898256877,
95.4148994466105));
#32677=CARTESIAN_POINT('Ctrl Pts',(-6.29316109120236,-2.49376120546088,
95.4231028997509));
#32678=CARTESIAN_POINT('Ctrl Pts',(-6.22671386686271,-2.65534043552512,
95.4313063528913));
#32679=CARTESIAN_POINT('Ctrl Pts',(-6.1540741762698,-2.81418905423377,95.4395098060317));
#32680=CARTESIAN_POINT('Ctrl Pts',(-6.08147235567091,-2.97295485876479,
95.4477089823818));
#32681=CARTESIAN_POINT('Ctrl Pts',(-6.00268464912206,-3.12899256258344,
95.455908158732));
#32682=CARTESIAN_POINT('Ctrl Pts',(-5.91794873054344,-3.28179399454921,
95.4641073350821));
#32683=CARTESIAN_POINT('Ctrl Pts',(-5.8332287563066,-3.43456667461972,95.4723049686335));
#32684=CARTESIAN_POINT('Ctrl Pts',(-5.74256296776677,-3.5841039794754,95.4805026021849));
#32685=CARTESIAN_POINT('Ctrl Pts',(-5.64623538618265,-3.72992157609498,
95.4887002357363));
#32686=CARTESIAN_POINT('Ctrl Pts',(-5.54991474254855,-3.87572867026883,
95.4968972788568));
#32687=CARTESIAN_POINT('Ctrl Pts',(-5.44793331496594,-4.01781629000376,
95.5050943219774));
#32688=CARTESIAN_POINT('Ctrl Pts',(-5.34061889447139,-4.15572843482526,
95.513291365098));
#32689=CARTESIAN_POINT('Ctrl Pts',(-5.23329269903204,-4.29365571188979,
95.5214893076292));
#32690=CARTESIAN_POINT('Ctrl Pts',(-5.1206325651975,-4.4274063181409,95.5296872501603));
#32691=CARTESIAN_POINT('Ctrl Pts',(-5.00300709506265,-4.55655670509572,
95.5378851926915));
#32692=CARTESIAN_POINT('Ctrl Pts',(-4.88534734030277,-4.68574473587535,
95.5460855247));
#32693=CARTESIAN_POINT('Ctrl Pts',(-4.7627196079308,-4.81032961145549,95.5542858567084));
#32694=CARTESIAN_POINT('Ctrl Pts',(-4.63552995592562,-4.92992403873693,
95.5624861887169));
#32695=CARTESIAN_POINT('Ctrl Pts',(-4.50820773792677,-5.04964311573508,
95.5706950676877));
#32696=CARTESIAN_POINT('Ctrl Pts',(-4.3763143626688,-5.16436110680497,95.5789039466584));
#32697=CARTESIAN_POINT('Ctrl Pts',(-4.24029038600628,-5.2737298416152,95.5871128256291));
#32698=CARTESIAN_POINT('Ctrl Pts',(-4.10419338851791,-5.38315728809917,
95.5953261113166));
#32699=CARTESIAN_POINT('Ctrl Pts',(-3.96396165690328,-5.48722954013065,
95.603539397004));
#32700=CARTESIAN_POINT('Ctrl Pts',(-3.8200653395177,-5.58564139574101,95.6117526826914));
#32701=CARTESIAN_POINT('Ctrl Pts',(-3.67595851955472,-5.68419721576705,
95.6199779834034));
#32702=CARTESIAN_POINT('Ctrl Pts',(-3.52817670420056,-5.77707590056016,
95.6282032841155));
#32703=CARTESIAN_POINT('Ctrl Pts',(-3.37721638996576,-5.86401726253825,
95.6364285848276));
#32704=CARTESIAN_POINT('Ctrl Pts',(-3.24069099575598,-5.94264523689934,
95.6438673771215));
#32705=CARTESIAN_POINT('Ctrl Pts',(-3.10156638207696,-6.01641757989647,
95.6513061694154));
#32706=CARTESIAN_POINT('Ctrl Pts',(-2.96022349961675,-6.08517590808325,
95.6587449617093));
#32707=CARTESIAN_POINT('Ctrl Pts',(-2.80531854339851,-6.16053170691812,
95.6668975179225));
#32708=CARTESIAN_POINT('Ctrl Pts',(-2.64729201842329,-6.23008659198876,
95.6750500741358));
#32709=CARTESIAN_POINT('Ctrl Pts',(-2.48662143000296,-6.29356837285892,
95.683202630349));
#32710=CARTESIAN_POINT('Ctrl Pts',(-2.32613698233264,-6.35697660855556,
95.6913457416294));
#32711=CARTESIAN_POINT('Ctrl Pts',(-2.16301490534355,-6.41432561260147,
95.6994888529097));
#32712=CARTESIAN_POINT('Ctrl Pts',(-1.99775729792893,-6.4653889889605,95.7076319641901));
#32713=CARTESIAN_POINT('Ctrl Pts',(-1.8326564020831,-6.5164039426058,95.7157673534674));
#32714=CARTESIAN_POINT('Ctrl Pts',(-1.66542435438282,-6.56114502813015,
95.7239027427447));
#32715=CARTESIAN_POINT('Ctrl Pts',(-1.49658323480923,-6.5994338864245,95.7320381320221));
#32716=CARTESIAN_POINT('Ctrl Pts',(-1.32786674740724,-6.63769448132206,
95.7401675160607));
#32717=CARTESIAN_POINT('Ctrl Pts',(-1.15754390817,-6.66951225203777,95.7482969000992));
#32718=CARTESIAN_POINT('Ctrl Pts',(-0.986151962342344,-6.69475864442986,
95.7564262841378));
#32719=CARTESIAN_POINT('Ctrl Pts',(-0.814850531104618,-6.71999170383338,
95.76455137493));
#32720=CARTESIAN_POINT('Ctrl Pts',(-0.642481478574638,-6.73866024328767,
95.7726764657221));
#32721=CARTESIAN_POINT('Ctrl Pts',(-0.469592245319419,-6.7506867889968,
95.7808015565143));
#32722=CARTESIAN_POINT('Ctrl Pts',(-0.296043056380474,-6.76275924263811,
95.7889576625394));
#32723=CARTESIAN_POINT('Ctrl Pts',(-0.121970072306283,-6.76813881991057,
95.7971137685645));
#32724=CARTESIAN_POINT('Ctrl Pts',(0.0520672536939946,-6.76679968678642,
95.8052698745896));
#32725=CARTESIAN_POINT('Ctrl Pts',(0.225404110931855,-6.76546594343091,
95.813393153763));
#32726=CARTESIAN_POINT('Ctrl Pts',(0.398705228442972,-6.75746749683414,
95.8215164329364));
#32727=CARTESIAN_POINT('Ctrl Pts',(0.5714177203458,-6.7428310663159,95.8296397121098));
#32728=CARTESIAN_POINT('Ctrl Pts',(0.74415321037656,-6.72819268683324,95.8377640729665));
#32729=CARTESIAN_POINT('Ctrl Pts',(0.91629955412383,-6.70691459375123,95.8458884338232));
#32730=CARTESIAN_POINT('Ctrl Pts',(1.08730896929934,-6.67907540047881,95.8540127946799));
#32731=CARTESIAN_POINT('Ctrl Pts',(1.25837369124453,-6.65122720363283,95.8621397830653));
#32732=CARTESIAN_POINT('Ctrl Pts',(1.42830039152984,-6.61681373987404,95.8702667714507));
#32733=CARTESIAN_POINT('Ctrl Pts',(1.59655150175245,-6.57596474308158,95.8783937598361));
#32734=CARTESIAN_POINT('Ctrl Pts',(1.76589033624718,-6.53485166217554,95.8865732882762));
#32735=CARTESIAN_POINT('Ctrl Pts',(1.93353147535555,-6.48721963844231,95.8947528167163));
#32736=CARTESIAN_POINT('Ctrl Pts',(2.09894324979684,-6.43325160662416,95.9029323451564));
#32737=CARTESIAN_POINT('Ctrl Pts',(2.26357604686572,-6.37953772766642,95.9110733535601));
#32738=CARTESIAN_POINT('Ctrl Pts',(2.42600011122687,-6.31954757571661,95.9192143619638));
#32739=CARTESIAN_POINT('Ctrl Pts',(2.58571253791689,-6.25350938843618,95.9273553703674));
#32740=CARTESIAN_POINT('Ctrl Pts',(2.74655850879154,-6.18700250122608,95.9355541588257));
#32741=CARTESIAN_POINT('Ctrl Pts',(2.90465386627124,-6.1143615699947,95.943752947284));
#32742=CARTESIAN_POINT('Ctrl Pts',(3.059511629435,-6.03586593533621,95.9519517357423));
#32743=CARTESIAN_POINT('Ctrl Pts',(3.21436939259886,-5.95737030067766,95.9601505242005));
#32744=CARTESIAN_POINT('Ctrl Pts',(3.36598926841503,-5.87302019974696,95.9683493126588));
#32745=CARTESIAN_POINT('Ctrl Pts',(3.51391566987933,-5.7831380465087,95.9765481011171));
#32746=CARTESIAN_POINT('Ctrl Pts',(3.66246023659221,-5.69288028740801,95.9847811512491));
#32747=CARTESIAN_POINT('Ctrl Pts',(3.80774221389315,-5.59676367682404,95.9930142013811));
#32748=CARTESIAN_POINT('Ctrl Pts',(3.94926832976421,-5.49504946834161,96.0012472515131));
#32749=CARTESIAN_POINT('Ctrl Pts',(4.09062590978606,-5.39345638584642,96.009470497348));
#32750=CARTESIAN_POINT('Ctrl Pts',(4.22823624653368,-5.28627918585261,96.0176937431829));
#32751=CARTESIAN_POINT('Ctrl Pts',(4.36163156742462,-5.17382441430371,96.0259169890177));
#32752=CARTESIAN_POINT('Ctrl Pts',(4.49489473435468,-5.06148105103645,96.0341320881312));
#32753=CARTESIAN_POINT('Ctrl Pts',(4.62395092959647,-4.9438707580321,96.0423471872447));
#32754=CARTESIAN_POINT('Ctrl Pts',(4.74836216306603,-4.82134273500266,96.0505622863583));
#32755=CARTESIAN_POINT('Ctrl Pts',(4.87267503523879,-4.69891158437696,96.0587708904972));
#32756=CARTESIAN_POINT('Ctrl Pts',(4.99235000622279,-4.57157069810194,96.0669794946361));
#32757=CARTESIAN_POINT('Ctrl Pts',(5.10698287118173,-4.43970888161109,96.075188098775));
#32758=CARTESIAN_POINT('Ctrl Pts',(5.22154803553013,-4.30792494091517,96.083391855024));
#32759=CARTESIAN_POINT('Ctrl Pts',(5.33107679166752,-4.17162565859752,96.091595611273));
#32760=CARTESIAN_POINT('Ctrl Pts',(5.43520240333724,-4.0312360182402,96.0997993675219));
#32761=CARTESIAN_POINT('Ctrl Pts',(5.53929720686305,-3.89088791563881,96.1080006964862));
#32762=CARTESIAN_POINT('Ctrl Pts',(5.63799183417681,-3.74645215076367,96.1162020254505));
#32763=CARTESIAN_POINT('Ctrl Pts',(5.73096025495111,-3.5983862433278,96.1244033544148));
#32764=CARTESIAN_POINT('Ctrl Pts',(5.82391585449262,-3.45034075559415,96.1326035523375));
#32765=CARTESIAN_POINT('Ctrl Pts',(5.91114662916736,-3.29866642528091,96.1408037502602));
#32766=CARTESIAN_POINT('Ctrl Pts',(5.99237025890225,-3.14384918216886,96.149003948183));
#32767=CARTESIAN_POINT('Ctrl Pts',(6.07359740649754,-2.98902523379813,96.1572045012628));
#32768=CARTESIAN_POINT('Ctrl Pts',(6.14881672430619,-2.83105841870121,96.1654050543427));
#32769=CARTESIAN_POINT('Ctrl Pts',(6.21779215777247,-2.67045870268445,96.1736056074225));
#32770=CARTESIAN_POINT('Ctrl Pts',(6.28678307831959,-2.50982292715116,96.1818080017757));
#32771=CARTESIAN_POINT('Ctrl Pts',(6.34952718089141,-2.34655340240013,96.190010396129));
#32772=CARTESIAN_POINT('Ctrl Pts',(6.4058367827842,-2.18117952317754,96.1982127904822));
#32773=CARTESIAN_POINT('Ctrl Pts',(6.46219904405341,-2.01565099030683,96.206422855516));
#32774=CARTESIAN_POINT('Ctrl Pts',(6.51211466676788,-1.84801451078317,96.2146329205499));
#32775=CARTESIAN_POINT('Ctrl Pts',(6.55544577102335,-1.67881498181666,96.2228429855837));
#32776=CARTESIAN_POINT('Ctrl Pts',(6.59879761277662,-1.50953447695721,96.231056979809));
#32777=CARTESIAN_POINT('Ctrl Pts',(6.63555857770002,-1.33868978124384,96.2392709740343));
#32778=CARTESIAN_POINT('Ctrl Pts',(6.66564207759946,-1.16683533257079,96.2474849682597));
#32779=CARTESIAN_POINT('Ctrl Pts',(6.69576659132887,-0.994746589046405,
96.2557101608948));
#32780=CARTESIAN_POINT('Ctrl Pts',(6.71919539828306,-0.821645696495592,
96.2639353535301));
#32781=CARTESIAN_POINT('Ctrl Pts',(6.73589376039568,-0.648092777820142,
96.2721605461653));
#32782=CARTESIAN_POINT('Ctrl Pts',(6.75091056167843,-0.492017009776847,
96.2795574442851));
#32783=CARTESIAN_POINT('Ctrl Pts',(6.76048489711358,-0.335575896286213,
96.2869543424049));
#32784=CARTESIAN_POINT('Ctrl Pts',(6.76462749297208,-0.179175560069701,
96.2943512405248));
#32785=CARTESIAN_POINT('Ctrl Pts',(6.76946962333506,0.0036351322212177,
96.3029972070157));
#32786=CARTESIAN_POINT('Ctrl Pts',(6.76690119693744,0.186805049357144,96.3116431735065));
#32787=CARTESIAN_POINT('Ctrl Pts',(6.75689235845708,0.369722404277046,96.3202891399974));
#32788=CARTESIAN_POINT('Ctrl Pts',(6.74689632264179,0.552405783033099,96.3289240471218));
#32789=CARTESIAN_POINT('Ctrl Pts',(6.72947886938024,0.734836940739044,96.3375589542462));
#32790=CARTESIAN_POINT('Ctrl Pts',(6.70466212033849,0.916403214801301,96.3461938613706));
#32791=CARTESIAN_POINT('Ctrl Pts',(6.67902147525857,1.10399734261729,96.3551154404421));
#32792=CARTESIAN_POINT('Ctrl Pts',(6.64548175244634,1.29066785329551,96.3640370195136));
#32793=CARTESIAN_POINT('Ctrl Pts',(6.60412588314898,1.4757406003501,96.3729585985851));
#32794=CARTESIAN_POINT('Ctrl Pts',(6.56420942591019,1.65437179634198,96.3815696575608));
#32795=CARTESIAN_POINT('Ctrl Pts',(6.51701177788901,1.831514230476,96.3901807165365));
#32796=CARTESIAN_POINT('Ctrl Pts',(6.46266000992232,2.00656786482563,96.3987917755122));
#32797=CARTESIAN_POINT('Ctrl Pts',(6.40835949818211,2.18145641551627,96.4073947138618));
#32798=CARTESIAN_POINT('Ctrl Pts',(6.34691840770841,2.35425980347348,96.4159976522113));
#32799=CARTESIAN_POINT('Ctrl Pts',(6.27851436634138,2.52439029304997,96.4246005905608));
#32800=CARTESIAN_POINT('Ctrl Pts',(6.21018692167635,2.69433027583548,96.4331938956096));
#32801=CARTESIAN_POINT('Ctrl Pts',(6.13491219422502,2.86160304890591,96.4417872006583));
#32802=CARTESIAN_POINT('Ctrl Pts',(6.05291701063844,3.02563789345715,96.4503805057071));
#32803=CARTESIAN_POINT('Ctrl Pts',(6.04378140506187,3.04391406011823,96.4513379405476));
#32804=CARTESIAN_POINT('Ctrl Pts',(6.03456242450087,3.06215005045793,96.4522953753882));
#32805=CARTESIAN_POINT('Ctrl Pts',(6.02526042023025,3.08034508917538,96.4532528102288));
#32806=CARTESIAN_POINT('Ctrl Pts',(5.94174792410106,3.24369838984614,96.4618485677764));
#32807=CARTESIAN_POINT('Ctrl Pts',(5.8516374843168,3.40355764061782,96.4704443253239));
#32808=CARTESIAN_POINT('Ctrl Pts',(5.755254406341,3.55940103364211,96.4790400828715));
#32809=CARTESIAN_POINT('Ctrl Pts',(5.65878139967662,3.71538983385044,96.4876438605531));
#32810=CARTESIAN_POINT('Ctrl Pts',(5.55602423343683,3.86735503764123,96.4962476382347));
#32811=CARTESIAN_POINT('Ctrl Pts',(5.44735096650021,4.01480465873114,96.5048514159163));
#32812=CARTESIAN_POINT('Ctrl Pts',(5.33440674514439,4.16804917886619,96.5137933295843));
#32813=CARTESIAN_POINT('Ctrl Pts',(5.21507223743087,4.31641571057879,96.5227352432523));
#32814=CARTESIAN_POINT('Ctrl Pts',(5.08980496090979,4.45939171411282,96.5316771569203));
#32815=CARTESIAN_POINT('Ctrl Pts',(4.96894647579248,4.59733566623781,96.540304359251));
#32816=CARTESIAN_POINT('Ctrl Pts',(4.84256595275606,4.73026188209838,96.5489315615817));
#32817=CARTESIAN_POINT('Ctrl Pts',(4.71111061934437,4.85774903965826,96.5575587639125));
#32818=CARTESIAN_POINT('Ctrl Pts',(4.57953009484883,4.98535760922188,96.5661941823329));
#32819=CARTESIAN_POINT('Ctrl Pts',(4.44286533809791,5.10751657560102,96.5748296007532));
#32820=CARTESIAN_POINT('Ctrl Pts',(4.30159692963566,5.22384464307172,96.5834650191737));
#32821=CARTESIAN_POINT('Ctrl Pts',(4.16011981722177,5.34034456869268,96.5921131951948));
#32822=CARTESIAN_POINT('Ctrl Pts',(4.01402570236079,5.4509961935557,96.6007613712159));
#32823=CARTESIAN_POINT('Ctrl Pts',(3.8638256196798,5.55546042922691,96.6094095472371));
#32824=CARTESIAN_POINT('Ctrl Pts',(3.84793502044534,5.5665123492642,96.6103244914688));
#32825=CARTESIAN_POINT('Ctrl Pts',(3.83199848768264,5.57749505656461,96.6112394357006));
#32826=CARTESIAN_POINT('Ctrl Pts',(3.81601664313435,5.58840817937645,96.6121543799324));
#32827=CARTESIAN_POINT('Ctrl Pts',(3.67232792393951,5.68652530437489,96.6203804119402));
#32828=CARTESIAN_POINT('Ctrl Pts',(3.52466401370678,5.77922588014726,96.628606443948));
#32829=CARTESIAN_POINT('Ctrl Pts',(3.37347074535601,5.86617286910531,96.6368324759558));
#32830=CARTESIAN_POINT('Ctrl Pts',(3.28326144601996,5.9180496956257,96.6417405290182));
#32831=CARTESIAN_POINT('Ctrl Pts',(3.19179639537182,5.96787904446892,96.6466485820806));
#32832=CARTESIAN_POINT('Ctrl Pts',(3.09917575053247,6.01559628526645,96.651556635143));
#32833=CARTESIAN_POINT('Origin',(0.,0.,-3.69717978381041));
#32834=CARTESIAN_POINT('',(3.09917575053247,6.01559628526645,99.0459901976524));
#32835=CARTESIAN_POINT('',(3.09917575053261,6.01559628526638,98.651480357023));
#32836=CARTESIAN_POINT('',(3.09917575053259,6.01559628526639,-3.69717978381041));
#32837=CARTESIAN_POINT('',(-6.767,5.7875637604881E-12,97.6971797838098));
#32838=CARTESIAN_POINT('Ctrl Pts',(-6.76699999999471,8.46578452749734E-6,
97.6973614935111));
#32839=CARTESIAN_POINT('Ctrl Pts',(-6.76700021337811,-0.170556414612781,
97.7054249703505));
#32840=CARTESIAN_POINT('Ctrl Pts',(-6.76054739979175,-0.341397623773265,
97.7134884471898));
#32841=CARTESIAN_POINT('Ctrl Pts',(-6.74760473158323,-0.511975962634623,
97.7215519240292));
#32842=CARTESIAN_POINT('Ctrl Pts',(-6.73467609075469,-0.682369427161041,
97.7296066616));
#32843=CARTESIAN_POINT('Ctrl Pts',(-6.71527162008903,-0.852500219493756,
97.7376613991708));
#32844=CARTESIAN_POINT('Ctrl Pts',(-6.68940644912142,-1.02182697089708,
97.7457161367415));
#32845=CARTESIAN_POINT('Ctrl Pts',(-6.66356363433439,-1.19100736721027,
97.7537639123182));
#32846=CARTESIAN_POINT('Ctrl Pts',(-6.63127128930906,-1.35938473877313,
97.7618116878949));
#32847=CARTESIAN_POINT('Ctrl Pts',(-6.5925964979879,-1.52642078560198,97.7698594634716));
#32848=CARTESIAN_POINT('Ctrl Pts',(-6.55394665663113,-1.6933490737777,97.77790204725));
#32849=CARTESIAN_POINT('Ctrl Pts',(-6.508922649235,-1.85893739707862,97.7859446310284));
#32850=CARTESIAN_POINT('Ctrl Pts',(-6.45764297323504,-2.02265573695282,
97.7939872148069));
#32851=CARTESIAN_POINT('Ctrl Pts',(-6.40523311497251,-2.1899823594492,97.8022070537133));
#32852=CARTESIAN_POINT('Ctrl Pts',(-6.34628870140792,-2.35535522032763,
97.8104268926197));
#32853=CARTESIAN_POINT('Ctrl Pts',(-6.28099080763204,-2.51822228455747,
97.8186467315261));
#32854=CARTESIAN_POINT('Ctrl Pts',(-6.21713029979191,-2.67750419750625,
97.8266856292082));
#32855=CARTESIAN_POINT('Ctrl Pts',(-6.14719326565084,-2.83438912434916,
97.8347245268905));
#32856=CARTESIAN_POINT('Ctrl Pts',(-6.07139848128779,-2.98837907257703,
97.8427634245726));
#32857=CARTESIAN_POINT('Ctrl Pts',(-5.995599517674,-3.14237751166096,97.8508027655118));
#32858=CARTESIAN_POINT('Ctrl Pts',(-5.91394232559818,-3.29348031874414,
97.858842106451));
#32859=CARTESIAN_POINT('Ctrl Pts',(-5.82669233804939,-3.44121278006992,
97.8668814473902));
#32860=CARTESIAN_POINT('Ctrl Pts',(-5.73942023282579,-3.58898269124103,
97.8749228262842));
#32861=CARTESIAN_POINT('Ctrl Pts',(-5.64655270034893,-3.73338023438517,
97.8829642051781));
#32862=CARTESIAN_POINT('Ctrl Pts',(-5.54839922872049,-3.87395856956858,
97.8910055840721));
#32863=CARTESIAN_POINT('Ctrl Pts',(-5.4464199561355,-4.02001633120827,97.8993603977794));
#32864=CARTESIAN_POINT('Ctrl Pts',(-5.33873463199313,-4.16195079374431,
97.9077152114868));
#32865=CARTESIAN_POINT('Ctrl Pts',(-5.2257366285637,-4.29929827865987,97.9160700251941));
#32866=CARTESIAN_POINT('Ctrl Pts',(-5.11679902718726,-4.43171040195134,
97.9241246220684));
#32867=CARTESIAN_POINT('Ctrl Pts',(-5.0029242146891,-4.55985924051399,97.9321792189428));
#32868=CARTESIAN_POINT('Ctrl Pts',(-4.88450213959166,-4.68336714857212,
97.9402338158171));
#32869=CARTESIAN_POINT('Ctrl Pts',(-4.76599545906791,-4.8069632955773,97.9482941672148));
#32870=CARTESIAN_POINT('Ctrl Pts',(-4.64293531433775,-4.92591165192842,
97.9563545186125));
#32871=CARTESIAN_POINT('Ctrl Pts',(-4.51574499210935,-5.03987461810702,
97.9644148700102));
#32872=CARTESIAN_POINT('Ctrl Pts',(-4.38838244307443,-5.15399190009662,
97.9724861358278));
#32873=CARTESIAN_POINT('Ctrl Pts',(-4.25687884341894,-5.2631100865309,97.9805574016454));
#32874=CARTESIAN_POINT('Ctrl Pts',(-4.12168714011927,-5.36693433153187,
97.988628667463));
#32875=CARTESIAN_POINT('Ctrl Pts',(-4.10697705485094,-5.37823135242596,
97.9895068944954));
#32876=CARTESIAN_POINT('Ctrl Pts',(-4.09222332896915,-5.38946574072866,
97.9903851215279));
#32877=CARTESIAN_POINT('Ctrl Pts',(-4.07742656333619,-5.40063714950379,
97.9912633485603));
#32878=CARTESIAN_POINT('Ctrl Pts',(-3.93873395085177,-5.50534867272368,
97.9994951205912));
#32879=CARTESIAN_POINT('Ctrl Pts',(-3.79580153277411,-5.60486788247453,
98.007726892622));
#32880=CARTESIAN_POINT('Ctrl Pts',(-3.64905391587604,-5.69883273302786,
98.0159586646529));
#32881=CARTESIAN_POINT('Ctrl Pts',(-3.5024815302977,-5.79268538015929,98.0241806071252));
#32882=CARTESIAN_POINT('Ctrl Pts',(-3.35210331618632,-5.88099668353843,
98.0324025495976));
#32883=CARTESIAN_POINT('Ctrl Pts',(-3.1983765797827,-5.9634449988155,98.04062449207));
#32884=CARTESIAN_POINT('Ctrl Pts',(-3.04480260796148,-6.04581138180968,
98.0488382640599));
#32885=CARTESIAN_POINT('Ctrl Pts',(-2.88788705426437,-6.12232621155359,
98.0570520360498));
#32886=CARTESIAN_POINT('Ctrl Pts',(-2.72811589115529,-6.19271125472729,
98.0652658080397));
#32887=CARTESIAN_POINT('Ctrl Pts',(-2.56847149929502,-6.26304045052749,
98.0734730627701));
#32888=CARTESIAN_POINT('Ctrl Pts',(-2.40597633742626,-6.32724940341208,
98.0816803175005));
#32889=CARTESIAN_POINT('Ctrl Pts',(-2.24114073350772,-6.38510588891152,
98.0898875722309));
#32890=CARTESIAN_POINT('Ctrl Pts',(-2.07640291358334,-6.44292805271039,
98.0980899582428));
#32891=CARTESIAN_POINT('Ctrl Pts',(-1.90932775465298,-6.49440513791089,
98.1062923442547));
#32892=CARTESIAN_POINT('Ctrl Pts',(-1.74044539424744,-6.53935308953744,
98.1144947302666));
#32893=CARTESIAN_POINT('Ctrl Pts',(-1.5716134411293,-6.5842876252909,98.1226946680653));
#32894=CARTESIAN_POINT('Ctrl Pts',(-1.40097570583604,-6.62269681358711,
98.130894605864));
#32895=CARTESIAN_POINT('Ctrl Pts',(-1.22907755420387,-6.65444643571141,
98.1390945436627));
#32896=CARTESIAN_POINT('Ctrl Pts',(-1.05720343836997,-6.68619161841908,
98.1472933348984));
#32897=CARTESIAN_POINT('Ctrl Pts',(-0.884069609390594,-6.71127902364263,
98.1554921261342));
#32898=CARTESIAN_POINT('Ctrl Pts',(-0.710231717166204,-6.7296255399488,
98.1636909173699));
#32899=CARTESIAN_POINT('Ctrl Pts',(-0.536386596869409,-6.74797281909181,
98.1718900495063));
#32900=CARTESIAN_POINT('Ctrl Pts',(-0.361837711464924,-6.7595786132292,
98.1800891816428));
#32901=CARTESIAN_POINT('Ctrl Pts',(-0.187145984910275,-6.76441168028174,
98.1882883137792));
#32902=CARTESIAN_POINT('Ctrl Pts',(-0.0124153049127425,-6.76924582503042,
98.1964892741901));
#32903=CARTESIAN_POINT('Ctrl Pts',(0.162457921454999,-6.76730422488259,
98.204690234601));
#32904=CARTESIAN_POINT('Ctrl Pts',(0.336912557256312,-6.75860776556556,
98.2128911950119));
#32905=CARTESIAN_POINT('Ctrl Pts',(0.511530699047683,-6.74990315557265,
98.2210998416969));
#32906=CARTESIAN_POINT('Ctrl Pts',(0.68572910798653,-6.73443105547005,98.229308488382));
#32907=CARTESIAN_POINT('Ctrl Pts',(0.8589506080348,-6.71226436107493,98.237517135067));
#32908=CARTESIAN_POINT('Ctrl Pts',(1.03225480889225,-6.69008708367735,98.2457297007905));
#32909=CARTESIAN_POINT('Ctrl Pts',(1.20458081761655,-6.66120889854043,98.253942266514));
#32910=CARTESIAN_POINT('Ctrl Pts',(1.37538151702226,-6.625753895417,98.2621548322375));
#32911=CARTESIAN_POINT('Ctrl Pts',(1.54641657963445,-6.59025024291306,98.2703786667863));
#32912=CARTESIAN_POINT('Ctrl Pts',(1.71592180208878,-6.54815182324261,98.278602501335));
#32913=CARTESIAN_POINT('Ctrl Pts',(1.88336390244769,-6.49963302125258,98.2868263358838));
#32914=CARTESIAN_POINT('Ctrl Pts',(2.03721169533878,-6.45505336903916,98.2943824928582));
#32915=CARTESIAN_POINT('Ctrl Pts',(2.18931775827407,-6.40505417374424,98.3019386498325));
#32916=CARTESIAN_POINT('Ctrl Pts',(2.33928402396668,-6.34980623761184,98.3094948068069));
#32917=CARTESIAN_POINT('Ctrl Pts',(2.51087469564636,-6.28659181784823,98.3181405248593));
#32918=CARTESIAN_POINT('Ctrl Pts',(2.68005497109013,-6.21636147434551,98.3267862429117));
#32919=CARTESIAN_POINT('Ctrl Pts',(2.84624552993176,-6.13931391796701,98.3354319609641));
#32920=CARTESIAN_POINT('Ctrl Pts',(3.0122227339653,-6.06236527494869,98.3440665796765));
#32921=CARTESIAN_POINT('Ctrl Pts',(3.1752175995722,-5.97861699848319,98.3527011983889));
#32922=CARTESIAN_POINT('Ctrl Pts',(3.33466923044143,-5.8883164082399,98.3613358171013));
#32923=CARTESIAN_POINT('Ctrl Pts',(3.49975207349135,-5.79482675193983,98.3702753770037));
#32924=CARTESIAN_POINT('Ctrl Pts',(3.66103653636448,-5.69431361453289,98.3792149369062));
#32925=CARTESIAN_POINT('Ctrl Pts',(3.81792347095631,-5.58710563439791,98.3881544968086));
#32926=CARTESIAN_POINT('Ctrl Pts',(3.96903818031422,-5.48384207837845,98.3967651500791));
#32927=CARTESIAN_POINT('Ctrl Pts',(4.11607286612411,-5.3743676871414,98.4053758033496));
#32928=CARTESIAN_POINT('Ctrl Pts',(4.25851726878939,-5.25902269166264,98.4139864566201));
#32929=CARTESIAN_POINT('Ctrl Pts',(4.40082683829702,-5.1437868779395,98.4225889593312));
#32930=CARTESIAN_POINT('Ctrl Pts',(4.53855455119751,-5.02269173027942,98.4311914620423));
#32931=CARTESIAN_POINT('Ctrl Pts',(4.67122029642491,-4.89611988642721,98.4397939647534));
#32932=CARTESIAN_POINT('Ctrl Pts',(4.80373672902785,-4.76969049663619,98.4483867855209));
#32933=CARTESIAN_POINT('Ctrl Pts',(4.93120233938645,-4.63779691755874,98.4569796062884));
#32934=CARTESIAN_POINT('Ctrl Pts',(5.0531710449642,-4.50086118318877,98.4655724270559));
#32935=CARTESIAN_POINT('Ctrl Pts',(5.06754561092885,-4.48472268489698,98.4665851300141));
#32936=CARTESIAN_POINT('Ctrl Pts',(5.08184386603344,-4.46851419716626,98.4675978329723));
#32937=CARTESIAN_POINT('Ctrl Pts',(5.09606511214929,-4.45223644618464,98.4686105359305));
#32938=CARTESIAN_POINT('Ctrl Pts',(5.21676711568027,-4.31407997660005,98.4772057936906));
#32939=CARTESIAN_POINT('Ctrl Pts',(5.33177651931316,-4.17109364975173,98.4858010514507));
#32940=CARTESIAN_POINT('Ctrl Pts',(5.44072957655019,-4.02377318879332,98.4943963092107));
#32941=CARTESIAN_POINT('Ctrl Pts',(5.54978466370526,-3.87631476847024,98.5029996160652));
#32942=CARTESIAN_POINT('Ctrl Pts',(5.65277190234388,-3.72451435815284,98.5116029229197));
#32943=CARTESIAN_POINT('Ctrl Pts',(5.7493711082545,-3.56889630832397,98.5202062297742));
#32944=CARTESIAN_POINT('Ctrl Pts',(5.84997535073926,-3.40682628018653,98.5291662327142));
#32945=CARTESIAN_POINT('Ctrl Pts',(5.94365038361258,-3.2406156366243,98.5381262356541));
#32946=CARTESIAN_POINT('Ctrl Pts',(6.03008829914884,-3.0708832775715,98.5470862385941));
#32947=CARTESIAN_POINT('Ctrl Pts',(6.11331219419341,-2.90746207580094,98.5557130817989));
#32948=CARTESIAN_POINT('Ctrl Pts',(6.18982738122912,-2.74077662017317,98.5643399250036));
#32949=CARTESIAN_POINT('Ctrl Pts',(6.25940878415947,-2.57139858302585,98.5729667682084));
#32950=CARTESIAN_POINT('Ctrl Pts',(6.32905668932188,-2.40185866329124,98.5816018564945));
#32951=CARTESIAN_POINT('Ctrl Pts',(6.39175747526719,-2.22962131062627,98.5902369447806));
#32952=CARTESIAN_POINT('Ctrl Pts',(6.4473356177723,-2.05527429600155,98.5988720330667));
#32953=CARTESIAN_POINT('Ctrl Pts',(6.50299630497266,-1.8806683410715,98.6075199461918));
#32954=CARTESIAN_POINT('Ctrl Pts',(6.55151312418768,-1.70394675572282,98.616167859317));
#32955=CARTESIAN_POINT('Ctrl Pts',(6.59276104946669,-1.52570991496907,98.6248157724421));
#32956=CARTESIAN_POINT('Ctrl Pts',(6.59738843875867,-1.50571445476685,98.6257859366461));
#32957=CARTESIAN_POINT('Ctrl Pts',(6.60192439938738,-1.48569993195239,98.62675610085));
#32958=CARTESIAN_POINT('Ctrl Pts',(6.60636879538482,-1.46566719938933,98.627726265054));
#32959=CARTESIAN_POINT('Ctrl Pts',(6.64404667773131,-1.29583738651382,98.6359509445728));
#32960=CARTESIAN_POINT('Ctrl Pts',(6.67522128892439,-1.12432995693657,98.6441756240916));
#32961=CARTESIAN_POINT('Ctrl Pts',(6.69974528392764,-0.95168383956509,98.6524003036103));
#32962=CARTESIAN_POINT('Ctrl Pts',(6.72424350143763,-0.779219192795254,
98.6606163380605));
#32963=CARTESIAN_POINT('Ctrl Pts',(6.74210497342658,-0.60561859359595,98.6688323725106));
#32964=CARTESIAN_POINT('Ctrl Pts',(6.75323287948293,-0.431433280439463,
98.6770484069607));
#32965=CARTESIAN_POINT('Ctrl Pts',(6.76435131779029,-0.257396166127547,
98.6852574511153));
#32966=CARTESIAN_POINT('Ctrl Pts',(6.76874757741193,-0.0827756843283776,
98.6934664952699));
#32967=CARTESIAN_POINT('Ctrl Pts',(6.76637635560913,0.0918695501989991,
98.7016755394246));
#32968=CARTESIAN_POINT('Ctrl Pts',(6.76400667644305,0.266401166441519,98.7098792430526));
#32969=CARTESIAN_POINT('Ctrl Pts',(6.75487829047703,0.440957146231089,98.7180829466806));
#32970=CARTESIAN_POINT('Ctrl Pts',(6.73899791488554,0.614976506192181,98.7262866503086));
#32971=CARTESIAN_POINT('Ctrl Pts',(6.72312469120729,0.788917494495235,98.7344866593026));
#32972=CARTESIAN_POINT('Ctrl Pts',(6.700505568594,0.962321988254316,98.7426866682966));
#32973=CARTESIAN_POINT('Ctrl Pts',(6.67119929074061,1.13463166852598,98.7508866772905));
#32974=CARTESIAN_POINT('Ctrl Pts',(6.64189535627904,1.30692757055193,98.7590860305945));
#32975=CARTESIAN_POINT('Ctrl Pts',(6.60590538309038,1.47812847892829,98.7672853838984));
#32976=CARTESIAN_POINT('Ctrl Pts',(6.56333971309382,1.64768346794082,98.7754847372023));
#32977=CARTESIAN_POINT('Ctrl Pts',(6.52077432061295,1.81723735150458,98.7836840370488));
#32978=CARTESIAN_POINT('Ctrl Pts',(6.47163340295877,1.98514498908865,98.7918833368954));
#32979=CARTESIAN_POINT('Ctrl Pts',(6.41607791618785,2.15086800464523,98.800082636742));
#32980=CARTESIAN_POINT('Ctrl Pts',(6.36051271331179,2.31662000351808,98.808283370565));
#32981=CARTESIAN_POINT('Ctrl Pts',(6.29853082018612,2.48018627922513,98.816484104388));
#32982=CARTESIAN_POINT('Ctrl Pts',(6.23034234743438,2.6410458598377,98.824684838211));
#32983=CARTESIAN_POINT('Ctrl Pts',(6.16212957900082,2.80196275502311,98.832888493971));
#32984=CARTESIAN_POINT('Ctrl Pts',(6.08770596552259,2.96017070410215,98.841092149731));
#32985=CARTESIAN_POINT('Ctrl Pts',(6.00732883561685,3.11517082368949,98.849295805491));
#32986=CARTESIAN_POINT('Ctrl Pts',(5.92685962854182,3.2703485058779,98.857508859066));
#32987=CARTESIAN_POINT('Ctrl Pts',(5.84042344468821,3.42231069834952,98.865721912641));
#32988=CARTESIAN_POINT('Ctrl Pts',(5.74832300072423,3.5705842210127,98.873934966216));
#32989=CARTESIAN_POINT('Ctrl Pts',(5.65616805886127,3.71894548044576,98.8821528796391));
#32990=CARTESIAN_POINT('Ctrl Pts',(5.55834237625173,3.86361342269772,98.8903707930621));
#32991=CARTESIAN_POINT('Ctrl Pts',(5.4551906321931,4.00414587227197,98.8985887064852));
#32992=CARTESIAN_POINT('Ctrl Pts',(5.35187800620843,4.14489750506377,98.9068194370812));
#32993=CARTESIAN_POINT('Ctrl Pts',(5.24322294116174,4.28150047496693,98.9150501676772));
#32994=CARTESIAN_POINT('Ctrl Pts',(5.12960972230994,4.41354654408258,98.9232808982731));
#32995=CARTESIAN_POINT('Ctrl Pts',(5.02526956867612,4.53481506615697,98.930839839949));
#32996=CARTESIAN_POINT('Ctrl Pts',(4.91674818224055,4.6522404656876,98.9383987816248));
#32997=CARTESIAN_POINT('Ctrl Pts',(4.80436851752053,4.76553587205654,98.9459577233007));
#32998=CARTESIAN_POINT('Ctrl Pts',(4.68043564866504,4.89047862548467,98.95429376283));
#32999=CARTESIAN_POINT('Ctrl Pts',(4.55141798359906,5.01079282400249,98.9626298023593));
#33000=CARTESIAN_POINT('Ctrl Pts',(4.41769880299643,5.12603416746357,98.9709658418886));
#33001=CARTESIAN_POINT('Ctrl Pts',(4.28706592412992,5.23861568638195,98.9791094816952));
#33002=CARTESIAN_POINT('Ctrl Pts',(4.15194643805172,5.3463556469886,98.9872531215018));
#33003=CARTESIAN_POINT('Ctrl Pts',(4.01273794638276,5.44887356924896,98.9953967613083));
#33004=CARTESIAN_POINT('Ctrl Pts',(3.86859609398656,5.55502458806437,99.003829000699));
#33005=CARTESIAN_POINT('Ctrl Pts',(3.7200703367406,5.6555763442914,99.0122612400897));
#33006=CARTESIAN_POINT('Ctrl Pts',(3.56764291884306,5.75014895490795,99.0206934794804));
#33007=CARTESIAN_POINT('Ctrl Pts',(3.41521550094564,5.84472156552443,99.0291257188711));
#33008=CARTESIAN_POINT('Ctrl Pts',(3.25888676068621,5.93331475135205,99.0375579582617));
#33009=CARTESIAN_POINT('Ctrl Pts',(3.09917575053247,6.01559628526645,99.0459901976524));
#33010=CARTESIAN_POINT('Ctrl Pts',(3.09917575053274,6.01559628526631,97.0457515827422));
#33011=CARTESIAN_POINT('Ctrl Pts',(2.93382384459274,6.10078395293755,97.0545010306546));
#33012=CARTESIAN_POINT('Ctrl Pts',(2.76495772122987,6.17915010267048,97.063250478567));
#33013=CARTESIAN_POINT('Ctrl Pts',(2.59315093316709,6.25042856433178,97.0719999264794));
#33014=CARTESIAN_POINT('Ctrl Pts',(2.42134553245619,6.3217064504145,97.0807493037395));
#33015=CARTESIAN_POINT('Ctrl Pts',(2.24659977927597,6.38589665313455,97.0894986809995));
#33016=CARTESIAN_POINT('Ctrl Pts',(2.0695071868993,6.44278115439072,97.0982480582595));
#33017=CARTESIAN_POINT('Ctrl Pts',(1.89241596572865,6.49966521519723,97.1069973677741));
#33018=CARTESIAN_POINT('Ctrl Pts',(1.71297821457194,6.54924360009547,97.1157466772888));
#33019=CARTESIAN_POINT('Ctrl Pts',(1.53180337335832,6.59134792173559,97.1244959868035));
#33020=CARTESIAN_POINT('Ctrl Pts',(1.35062987477769,6.63345193135307,97.1332452314796));
#33021=CARTESIAN_POINT('Ctrl Pts',(1.16771959102938,6.6680819236824,97.1419944761557));
#33022=CARTESIAN_POINT('Ctrl Pts',(0.983693746906691,6.69512028363171,97.1507437208318));
#33023=CARTESIAN_POINT('Ctrl Pts',(0.799669205419827,6.72215845218867,97.159492903576));
#33024=CARTESIAN_POINT('Ctrl Pts',(0.614529402873543,6.74160505424578,97.1682420863202));
#33025=CARTESIAN_POINT('Ctrl Pts',(0.428903127363426,6.75339404354121,97.1769912690643));
#33026=CARTESIAN_POINT('Ctrl Pts',(0.243278104164192,6.76518295330329,97.1857403927829));
#33027=CARTESIAN_POINT('Ctrl Pts',(0.0571669005395649,6.76931433552275,
97.1944895165015));
#33028=CARTESIAN_POINT('Ctrl Pts',(-0.128798404776931,6.76577415902474,
97.2032386402201));
#33029=CARTESIAN_POINT('Ctrl Pts',(-0.314762517258624,6.76223400523444,
97.2119877078193));
#33030=CARTESIAN_POINT('Ctrl Pts',(-0.500580446819143,6.75102239665092,
97.2207367754186));
#33031=CARTESIAN_POINT('Ctrl Pts',(-0.685621118842352,6.732177410125,97.2294858430178));
#33032=CARTESIAN_POINT('Ctrl Pts',(-0.870660665414071,6.71333253821777,
97.2382348574035));
#33033=CARTESIAN_POINT('Ctrl Pts',(-1.05492267885429,6.68685441030621,97.2469838717893));
#33034=CARTESIAN_POINT('Ctrl Pts',(-1.23778137635179,6.65283295028191,97.2557328861751));
#33035=CARTESIAN_POINT('Ctrl Pts',(-1.42999922978773,6.61707018861881,97.2649296965425));
#33036=CARTESIAN_POINT('Ctrl Pts',(-1.62066601233621,6.57297172934431,97.2741265069099));
#33037=CARTESIAN_POINT('Ctrl Pts',(-1.80906628500311,6.52070304311315,97.2833233172773));
#33038=CARTESIAN_POINT('Ctrl Pts',(-1.98831342545455,6.47097374915053,97.292073315015));
#33039=CARTESIAN_POINT('Ctrl Pts',(-2.16550875896632,6.41384933989552,97.3008233127528));
#33040=CARTESIAN_POINT('Ctrl Pts',(-2.34005036713943,6.34952386240501,97.3095733104905));
#33041=CARTESIAN_POINT('Ctrl Pts',(-2.51458843547022,6.28519968948623,97.3183231307714));
#33042=CARTESIAN_POINT('Ctrl Pts',(-2.68647261717989,6.21367483971128,97.3270729510523));
#33043=CARTESIAN_POINT('Ctrl Pts',(-2.85511905908666,6.13519226743874,97.3358227713331));
#33044=CARTESIAN_POINT('Ctrl Pts',(-3.02376230488815,6.05671118252972,97.3445724257917));
#33045=CARTESIAN_POINT('Ctrl Pts',(-3.18916767379831,5.97127275992672,97.3533220802502));
#33046=CARTESIAN_POINT('Ctrl Pts',(-3.3507733410271,5.87916720438041,97.3620717347087));
#33047=CARTESIAN_POINT('Ctrl Pts',(-3.5123761603729,5.7870632719569,97.3708212349772));
#33048=CARTESIAN_POINT('Ctrl Pts',(-3.67017916302221,5.68829258362349,97.3795707352456));
#33049=CARTESIAN_POINT('Ctrl Pts',(-3.82364636566383,5.58319061741096,97.3883202355141));
#33050=CARTESIAN_POINT('Ctrl Pts',(-3.97711106778727,5.47809036367754,97.3970695932225));
#33051=CARTESIAN_POINT('Ctrl Pts',(-4.12623987481864,5.36665920043274,97.4058189509309));
#33052=CARTESIAN_POINT('Ctrl Pts',(-4.27052628213874,5.2492755951238,97.4145683086394));
#33053=CARTESIAN_POINT('Ctrl Pts',(-4.41481053024941,5.13189374643069,97.4233175354159));
#33054=CARTESIAN_POINT('Ctrl Pts',(-4.5542523013651,5.00855981477372,97.4320667621924));
#33055=CARTESIAN_POINT('Ctrl Pts',(-4.68837800630544,4.87969268192081,97.440815988969));
#33056=CARTESIAN_POINT('Ctrl Pts',(-4.82250188228888,4.75082730631816,97.4495650964398));
#33057=CARTESIAN_POINT('Ctrl Pts',(-4.95130963052957,4.61642907903535,97.4583142039106));
#33058=CARTESIAN_POINT('Ctrl Pts',(-5.07436379033356,4.47695444731702,97.4670633113815));
#33059=CARTESIAN_POINT('Ctrl Pts',(-5.19741643562794,4.33748153220599,97.4758123111712));
#33060=CARTESIAN_POINT('Ctrl Pts',(-5.31471544462761,4.19293255254604,97.484561310961));
#33061=CARTESIAN_POINT('Ctrl Pts',(-5.42586245275616,4.04379841779619,97.4933103107507));
#33062=CARTESIAN_POINT('Ctrl Pts',(-5.53702160019136,3.89464799484367,97.5020602660929));
#33063=CARTESIAN_POINT('Ctrl Pts',(-5.64202723081229,3.74091164443883,97.510810221435));
#33064=CARTESIAN_POINT('Ctrl Pts',(-5.74052265232941,3.58311159163275,97.5195601767772));
#33065=CARTESIAN_POINT('Ctrl Pts',(-5.83901427066893,3.42531763191826,97.5283097942596));
#33066=CARTESIAN_POINT('Ctrl Pts',(-5.93099603115716,3.26346052695656,97.5370594117421));
#33067=CARTESIAN_POINT('Ctrl Pts',(-6.01615550622731,3.09809004467121,97.5458090292245));
#33068=CARTESIAN_POINT('Ctrl Pts',(-6.10131214578774,2.9327250686388,97.5545583553756));
#33069=CARTESIAN_POINT('Ctrl Pts',(-6.1796468232872,2.76384720416954,97.5633076815267));
#33070=CARTESIAN_POINT('Ctrl Pts',(-6.25089348288535,2.59203002791662,97.5720570076778));
#33071=CARTESIAN_POINT('Ctrl Pts',(-6.32213814889309,2.42021765937085,97.5808060890094));
#33072=CARTESIAN_POINT('Ctrl Pts',(-6.3862950841257,2.24546640831962,97.5895551703409));
#33073=CARTESIAN_POINT('Ctrl Pts',(-6.44314639819802,2.06836976660073,97.5983042516725));
#33074=CARTESIAN_POINT('Ctrl Pts',(-6.5000028528369,1.8912571115831,97.6070541241069));
#33075=CARTESIAN_POINT('Ctrl Pts',(-6.5495522767324,1.71179891440292,97.6158039965413));
#33076=CARTESIAN_POINT('Ctrl Pts',(-6.59162635926376,1.53060476278471,97.6245538689757));
#33077=CARTESIAN_POINT('Ctrl Pts',(-6.63369752055186,1.34942319164746,97.6333031338982));
#33078=CARTESIAN_POINT('Ctrl Pts',(-6.66829431424243,1.16650618642765,97.6420523988207));
#33079=CARTESIAN_POINT('Ctrl Pts',(-6.69529923745407,0.982474997619267,
97.6508016637432));
#33080=CARTESIAN_POINT('Ctrl Pts',(-6.72230554731435,0.798434359178469,
97.6595513779229));
#33081=CARTESIAN_POINT('Ctrl Pts',(-6.74171916496696,0.613279706241085,
97.6683010921026));
#33082=CARTESIAN_POINT('Ctrl Pts',(-6.7534741481727,0.427639953656142,97.6770508062823));
#33083=CARTESIAN_POINT('Ctrl Pts',(-6.76248837758734,0.285283364200488,
97.6837604654581));
#33084=CARTESIAN_POINT('Ctrl Pts',(-6.76699999999988,0.142641701108184,
97.690470124634));
#33085=CARTESIAN_POINT('Ctrl Pts',(-6.767,5.78756373465266E-12,97.6971797838098));
#33086=CARTESIAN_POINT('',(-6.76699828620706,0.00481606382174074,97.3028202162221));
#33087=CARTESIAN_POINT('Ctrl Pts',(3.09917575053247,6.01559628526645,96.651556635143));
#33088=CARTESIAN_POINT('Ctrl Pts',(2.94418678798982,6.09544506692237,96.6597696426594));
#33089=CARTESIAN_POINT('Ctrl Pts',(2.7859605775845,6.16937712803934,96.6679826501758));
#33090=CARTESIAN_POINT('Ctrl Pts',(2.62498916978028,6.23712440620966,96.6761956576923));
#33091=CARTESIAN_POINT('Ctrl Pts',(2.46413507988091,6.30482230934598,96.6844026794697));
#33092=CARTESIAN_POINT('Ctrl Pts',(2.30054010645421,6.36634426930046,96.6926097012472));
#33093=CARTESIAN_POINT('Ctrl Pts',(2.13471964029275,6.42146876168906,96.7008167230246));
#33094=CARTESIAN_POINT('Ctrl Pts',(1.96898685975561,6.47656410432527,96.7090194049407));
#33095=CARTESIAN_POINT('Ctrl Pts',(1.80103127000067,6.52526860599149,96.7172220868568));
#33096=CARTESIAN_POINT('Ctrl Pts',(1.63138701126607,6.56740933850422,96.7254247687729));
#33097=CARTESIAN_POINT('Ctrl Pts',(1.45513466268568,6.61119156332967,96.7339469667132));
#33098=CARTESIAN_POINT('Ctrl Pts',(1.27705981573491,6.64788823092621,96.7424691646535));
#33099=CARTESIAN_POINT('Ctrl Pts',(1.09777802498692,6.67736268356421,96.7509913625938));
#33100=CARTESIAN_POINT('Ctrl Pts',(0.92526260422526,6.70572472511539,96.759191919702));
#33101=CARTESIAN_POINT('Ctrl Pts',(0.751630058849052,6.72739969300063,96.7673924768102));
#33102=CARTESIAN_POINT('Ctrl Pts',(0.577438170068366,6.74231815919036,96.7755930339184));
#33103=CARTESIAN_POINT('Ctrl Pts',(0.403227077395019,6.75723827007563,96.7837944951021));
#33104=CARTESIAN_POINT('Ctrl Pts',(0.228456875528297,6.76540036430465,96.7919959562857));
#33105=CARTESIAN_POINT('Ctrl Pts',(0.0536892855156084,6.76678701161939,
96.8001974174694));
#33106=CARTESIAN_POINT('Ctrl Pts',(-0.121129244273583,6.76817406310234,
96.8084012691455));
#33107=CARTESIAN_POINT('Ctrl Pts',(-0.295944802446117,6.76278173074403,
96.8166051208216));
#33108=CARTESIAN_POINT('Ctrl Pts',(-0.470196793716727,6.75064470811333,
96.8248089724977));
#33109=CARTESIAN_POINT('Ctrl Pts',(-0.644531154044458,6.73850194830222,
96.8330167021411));
#33110=CARTESIAN_POINT('Ctrl Pts',(-0.818301059778924,6.71960817195363,
96.8412244317846));
#33111=CARTESIAN_POINT('Ctrl Pts',(-0.990952093649598,6.69404981667238,
96.849432161428));
#33112=CARTESIAN_POINT('Ctrl Pts',(-1.16380661045559,6.66846133884255,96.8576495645317));
#33113=CARTESIAN_POINT('Ctrl Pts',(-1.33553926760618,6.63619264851488,96.8658669676354));
#33114=CARTESIAN_POINT('Ctrl Pts',(-1.5056059627311,6.59738127479294,96.8740843707391));
#33115=CARTESIAN_POINT('Ctrl Pts',(-1.67579101629611,6.55854289017598,96.8823074927698));
#33116=CARTESIAN_POINT('Ctrl Pts',(-1.84430745232475,6.51315283974987,96.8905306148005));
#33117=CARTESIAN_POINT('Ctrl Pts',(-2.01062746299856,6.46139816177861,96.8987537368312));
#33118=CARTESIAN_POINT('Ctrl Pts',(-2.17717562068841,6.40957249009289,96.906988138808));
#33119=CARTESIAN_POINT('Ctrl Pts',(-2.34152100074633,6.35136487683304,96.9152225407848));
#33120=CARTESIAN_POINT('Ctrl Pts',(-2.50315604394867,6.28701032444223,96.9234569427616));
#33121=CARTESIAN_POINT('Ctrl Pts',(-2.54568983406041,6.27007561170981,96.9256238016211));
#33122=CARTESIAN_POINT('Ctrl Pts',(-2.58803607787279,6.25271549130404,96.9277906604806));
#33123=CARTESIAN_POINT('Ctrl Pts',(-2.63018582661199,6.23493476449349,96.9299575193402));
#33124=CARTESIAN_POINT('Ctrl Pts',(-2.78882584194334,6.16801301861826,96.938112977747));
#33125=CARTESIAN_POINT('Ctrl Pts',(-2.94516883681524,6.09492357467407,96.9462684361538));
#33126=CARTESIAN_POINT('Ctrl Pts',(-3.09869496624633,6.01584395626745,96.9544238945606));
#33127=CARTESIAN_POINT('Ctrl Pts',(-3.25203423419721,5.93686058815129,96.9625694267025));
#33128=CARTESIAN_POINT('Ctrl Pts',(-3.40256313992362,5.85190172383188,96.9707149588443));
#33129=CARTESIAN_POINT('Ctrl Pts',(-3.54977982079,5.76119364575711,96.9788604909862));
#33130=CARTESIAN_POINT('Ctrl Pts',(-3.69684827631917,5.6705768972476,96.9869978217868));
#33131=CARTESIAN_POINT('Ctrl Pts',(-3.840610837371,5.57422264936697,96.9951351525874));
#33132=CARTESIAN_POINT('Ctrl Pts',(-3.98058836081621,5.47240397830191,97.0032724833879));
#33133=CARTESIAN_POINT('Ctrl Pts',(-4.12045436439032,5.37066642601072,97.01140333119));
#33134=CARTESIAN_POINT('Ctrl Pts',(-4.25654104045743,5.2634733328904,97.0195341789919));
#33135=CARTESIAN_POINT('Ctrl Pts',(-4.38839648230385,5.15114213685695,97.027665026794));
#33136=CARTESIAN_POINT('Ctrl Pts',(-4.52017457364671,5.03887683779716,97.0357911047877));
#33137=CARTESIAN_POINT('Ctrl Pts',(-4.64772609644033,4.92147967492004,97.0439171827815));
#33138=CARTESIAN_POINT('Ctrl Pts',(-4.77063063078348,4.79930957374396,97.0520432607753));
#33139=CARTESIAN_POINT('Ctrl Pts',(-4.89397096215797,4.67670627970242,97.0601981523575));
#33140=CARTESIAN_POINT('Ctrl Pts',(-5.01263099277457,4.5492963609996,97.0683530439397));
#33141=CARTESIAN_POINT('Ctrl Pts',(-5.12622125432085,4.41748170927161,97.0765079355219));
#33142=CARTESIAN_POINT('Ctrl Pts',(-5.23936855356286,4.28618108859761,97.0846310258782));
#33143=CARTESIAN_POINT('Ctrl Pts',(-5.34748532593959,4.15051031727124,97.0927541162345));
#33144=CARTESIAN_POINT('Ctrl Pts',(-5.45022557716558,4.0109014146461,97.1008772065908));
#33145=CARTESIAN_POINT('Ctrl Pts',(-5.55297389602525,3.87128154929244,97.1090009348093));
#33146=CARTESIAN_POINT('Ctrl Pts',(-5.65034463591282,3.7277232312892,97.1171246630277));
#33147=CARTESIAN_POINT('Ctrl Pts',(-5.74203403516257,3.58068905925029,97.1252483912461));
#33148=CARTESIAN_POINT('Ctrl Pts',(-5.83374807808185,3.43361536834032,97.1333743029065));
#33149=CARTESIAN_POINT('Ctrl Pts',(-5.91977754634236,3.28306427347978,97.1415002145668));
#33150=CARTESIAN_POINT('Ctrl Pts',(-5.99986372172797,3.12952461576716,97.1496261262271));
#33151=CARTESIAN_POINT('Ctrl Pts',(-6.08046205652998,2.97500305598333,97.1578040039371));
#33152=CARTESIAN_POINT('Ctrl Pts',(-6.1550406449525,2.81745490935106,97.1659818816472));
#33153=CARTESIAN_POINT('Ctrl Pts',(-6.22338453038556,2.65739985454912,97.1741597593573));
#33154=CARTESIAN_POINT('Ctrl Pts',(-6.29140222527644,2.49810870780968,97.1822986058307));
#33155=CARTESIAN_POINT('Ctrl Pts',(-6.35324452736506,2.33633489402152,97.1904374523042));
#33156=CARTESIAN_POINT('Ctrl Pts',(-6.40874946345606,2.17260657152915,97.1985762987776));
#33157=CARTESIAN_POINT('Ctrl Pts',(-6.46465367473332,2.00770046808498,97.206773692106));
#33158=CARTESIAN_POINT('Ctrl Pts',(-6.51412889310712,1.84081199255287,97.2149710854344));
#33159=CARTESIAN_POINT('Ctrl Pts',(-6.55706192782659,1.67249151706282,97.2231684787627));
#33160=CARTESIAN_POINT('Ctrl Pts',(-6.59999496254606,1.50417104157277,97.2313658720911));
#33161=CARTESIAN_POINT('Ctrl Pts',(-6.63638579533957,1.33441894289787,97.2395632654195));
#33162=CARTESIAN_POINT('Ctrl Pts',(-6.6661743235188,1.16379074083731,97.2477606587479));
#33163=CARTESIAN_POINT('Ctrl Pts',(-6.71425349866384,0.888394012197591,
97.2609913866038));
#33164=CARTESIAN_POINT('Ctrl Pts',(-6.74526879236158,0.609985568231809,
97.2742221144597));
#33165=CARTESIAN_POINT('Ctrl Pts',(-6.75893709278174,0.330239876179668,
97.2874528423156));
#33166=CARTESIAN_POINT('Ctrl Pts',(-6.76422896296622,0.221932490367087,
97.2925753002736));
#33167=CARTESIAN_POINT('Ctrl Pts',(-6.766920989389,0.11342495687927,97.2976977582316));
#33168=CARTESIAN_POINT('Ctrl Pts',(-6.76699828620657,0.00481606451017424,
97.3028202161896));
#33169=CARTESIAN_POINT('Ctrl Pts',(-6.76699828620706,0.00481606382155593,
97.3028202162221));
#33170=CARTESIAN_POINT('Ctrl Pts',(-6.76712025881665,-0.166566307894805,
97.3109033388349));
#33171=CARTESIAN_POINT('Ctrl Pts',(-6.76072737653059,-0.338175828425599,
97.3189864614477));
#33172=CARTESIAN_POINT('Ctrl Pts',(-6.74779449262844,-0.50946882657651,
97.3270695840605));
#33173=CARTESIAN_POINT('Ctrl Pts',(-6.73487283404632,-0.680613148010278,
97.3351456907874));
#33174=CARTESIAN_POINT('Ctrl Pts',(-6.71542250083884,-0.851441125803964,
97.3432217975143));
#33175=CARTESIAN_POINT('Ctrl Pts',(-6.68947038760751,-1.02140830881792,
97.3512979042412));
#33176=CARTESIAN_POINT('Ctrl Pts',(-6.66353517089355,-1.19126483211662,
97.3593687528961));
#33177=CARTESIAN_POINT('Ctrl Pts',(-6.63110665762757,-1.3602613105025,97.3674396015511));
#33178=CARTESIAN_POINT('Ctrl Pts',(-6.59226363117107,-1.52785772149739,
97.3755104502061));
#33179=CARTESIAN_POINT('Ctrl Pts',(-6.55343387311752,-1.69539688317585,
97.3835785419371));
#33180=CARTESIAN_POINT('Ctrl Pts',(-6.50819404361204,-1.86153656734075,
97.391646633668));
#33181=CARTESIAN_POINT('Ctrl Pts',(-6.45667416967614,-2.02574619995618,
97.399714725399));
#33182=CARTESIAN_POINT('Ctrl Pts',(-6.40516252369416,-2.18992960756005,
97.4077815286197));
#33183=CARTESIAN_POINT('Ctrl Pts',(-6.34737293978065,-2.35218322242499,
97.4158483318404));
#33184=CARTESIAN_POINT('Ctrl Pts',(-6.28348549366712,-2.51199105310406,
97.4239151350611));
#33185=CARTESIAN_POINT('Ctrl Pts',(-6.21959571070349,-2.67180472917167,
97.4319822333462));
#33186=CARTESIAN_POINT('Ctrl Pts',(-6.14960775937732,-2.82917209784169,
97.4400493316312));
#33187=CARTESIAN_POINT('Ctrl Pts',(-6.07375004952149,-2.98359671134316,
97.4481164299163));
#33188=CARTESIAN_POINT('Ctrl Pts',(-5.99787467369683,-3.13805728770739,
97.4561854068912));
#33189=CARTESIAN_POINT('Ctrl Pts',(-5.91612698246284,-3.28957341148217,
97.4642543838661));
#33190=CARTESIAN_POINT('Ctrl Pts',(-5.82878150112226,-3.43767293560265,
97.472323360841));
#33191=CARTESIAN_POINT('Ctrl Pts',(-5.74135010679053,-3.58591813037385,
97.4804002744595));
#33192=CARTESIAN_POINT('Ctrl Pts',(-5.64831011398757,-3.73073969288594,
97.4884771880779));
#33193=CARTESIAN_POINT('Ctrl Pts',(-5.54998000547121,-3.87169354919392,
97.4965541016963));
#33194=CARTESIAN_POINT('Ctrl Pts',(-5.45159966181049,-4.01271941637859,
97.5046351416696));
#33195=CARTESIAN_POINT('Ctrl Pts',(-5.34792404227063,-4.14987334519492,
97.5127161816428));
#33196=CARTESIAN_POINT('Ctrl Pts',(-5.23931186014527,-4.28274447429929,
97.520797221616));
#33197=CARTESIAN_POINT('Ctrl Pts',(-5.13054413930407,-4.41580588228756,
97.5288898340903));
#33198=CARTESIAN_POINT('Ctrl Pts',(-5.01682597900833,-4.54457196028276,
97.5369824465645));
#33199=CARTESIAN_POINT('Ctrl Pts',(-4.89855359269738,-4.66866808623954,
97.5450750590387));
#33200=CARTESIAN_POINT('Ctrl Pts',(-4.79874025159647,-4.77339624245397,
97.5519046387443));
#33201=CARTESIAN_POINT('Ctrl Pts',(-4.69568404062259,-4.87479898062165,
97.55873421845));
#33202=CARTESIAN_POINT('Ctrl Pts',(-4.5896407234342,-4.97267403212743,97.5655637981556));
#33203=CARTESIAN_POINT('Ctrl Pts',(-4.46191197854839,-5.09056413417182,
97.5737899991745));
#33204=CARTESIAN_POINT('Ctrl Pts',(-4.32945957728245,-5.20369456492042,
97.5820162001933));
#33205=CARTESIAN_POINT('Ctrl Pts',(-4.19267247336223,-5.31166513732847,
97.5902424012122));
#33206=CARTESIAN_POINT('Ctrl Pts',(-4.05603902092366,-5.41951442755457,
97.5984593618279));
#33207=CARTESIAN_POINT('Ctrl Pts',(-3.91508084053274,-5.52221518069341,
97.6066763224437));
#33208=CARTESIAN_POINT('Ctrl Pts',(-3.77022318628941,-5.61940442801243,
97.6148932830595));
#33209=CARTESIAN_POINT('Ctrl Pts',(-3.62549917500851,-5.71650401034968,
97.6231026628611));
#33210=CARTESIAN_POINT('Ctrl Pts',(-3.47688315053867,-5.80810201490232,
97.6313120426627));
#33211=CARTESIAN_POINT('Ctrl Pts',(-3.32483292508749,-5.89387606081551,
97.6395214224643));
#33212=CARTESIAN_POINT('Ctrl Pts',(-3.1728924704349,-5.97958818320646,97.6477248756047));
#33213=CARTESIAN_POINT('Ctrl Pts',(-3.01752306419753,-6.05948454617642,
97.6559283287451));
#33214=CARTESIAN_POINT('Ctrl Pts',(-2.85921101992569,-6.13328634123139,
97.6641317818855));
#33215=CARTESIAN_POINT('Ctrl Pts',(-2.70098151009317,-6.20704966044074,
97.6723309582356));
#33216=CARTESIAN_POINT('Ctrl Pts',(-2.53981274273586,-6.27472459039795,
97.6805301345857));
#33217=CARTESIAN_POINT('Ctrl Pts',(-2.37621520132246,-6.33607846518681,
97.6887293109359));
#33218=CARTESIAN_POINT('Ctrl Pts',(-2.21264844325523,-6.39742079531828,
97.6969269444872));
#33219=CARTESIAN_POINT('Ctrl Pts',(-2.04665415471598,-6.45244430781402,
97.7051245780386));
#33220=CARTESIAN_POINT('Ctrl Pts',(-1.87876263760626,-6.50096454009209,
97.71332221159));
#33221=CARTESIAN_POINT('Ctrl Pts',(-1.71088321280617,-6.54948127772265,
97.7215192547105));
#33222=CARTESIAN_POINT('Ctrl Pts',(-1.54110717590793,-6.59149556754008,
97.7297162978311));
#33223=CARTESIAN_POINT('Ctrl Pts',(-1.36997977043031,-6.62687289968743,
97.7379133409517));
#33224=CARTESIAN_POINT('Ctrl Pts',(-1.19883358820531,-6.66225411356973,
97.7461112834829));
#33225=CARTESIAN_POINT('Ctrl Pts',(-1.02633609331553,-6.69099684630272,
97.7543092260141));
#33226=CARTESIAN_POINT('Ctrl Pts',(-0.853042547145141,-6.71301775751861,
97.7625071685453));
#33227=CARTESIAN_POINT('Ctrl Pts',(-0.679698490620669,-6.73504508723101,
97.7707075005537));
#33228=CARTESIAN_POINT('Ctrl Pts',(-0.505558276374564,-6.75034664767691,
97.7789078325621));
#33229=CARTESIAN_POINT('Ctrl Pts',(-0.331182163106764,-6.75889098705105,
97.7871081645706));
#33230=CARTESIAN_POINT('Ctrl Pts',(-0.15662430279854,-6.76744423193618,
97.7953170435413));
#33231=CARTESIAN_POINT('Ctrl Pts',(0.0181695890206001,-6.76922616762182,
97.8035259225121));
#33232=CARTESIAN_POINT('Ctrl Pts',(0.192638367528336,-6.76425749505118,
97.8117348014828));
#33233=CARTESIAN_POINT('Ctrl Pts',(0.367200804923314,-6.75928615518185,
97.8199480871702));
#33234=CARTESIAN_POINT('Ctrl Pts',(0.541437423555891,-6.74755700678809,
97.8281613728576));
#33235=CARTESIAN_POINT('Ctrl Pts',(0.714792420378166,-6.72914264938483,
97.836374658545));
#33236=CARTESIAN_POINT('Ctrl Pts',(0.888401014194871,-6.71070135404626,
97.8445999592571));
#33237=CARTESIAN_POINT('Ctrl Pts',(1.06112505389687,-6.68555535740216,97.8528252599692));
#33238=CARTESIAN_POINT('Ctrl Pts',(1.2324178746684,-6.65382861082233,97.8610505606813));
#33239=CARTESIAN_POINT('Ctrl Pts',(1.38733156837646,-6.62513559566919,97.8684893529752));
#33240=CARTESIAN_POINT('Ctrl Pts',(1.54107463423423,-6.59106087741857,97.8759281452692));
#33241=CARTESIAN_POINT('Ctrl Pts',(1.69325438273099,-6.55173096176593,97.8833669375632));
#33242=CARTESIAN_POINT('Ctrl Pts',(1.86003601946873,-6.50862727832513,97.8915194937764));
#33243=CARTESIAN_POINT('Ctrl Pts',(2.02543157073591,-6.45908359806189,97.8996720499897));
#33244=CARTESIAN_POINT('Ctrl Pts',(2.18890104298948,-6.4032024194148,97.9078246062029));
#33245=CARTESIAN_POINT('Ctrl Pts',(2.3521811319184,-6.3473859804604,97.9159677174833));
#33246=CARTESIAN_POINT('Ctrl Pts',(2.5135392412929,-6.28524677540145,97.9241108287636));
#33247=CARTESIAN_POINT('Ctrl Pts',(2.6724463572164,-6.21693811034024,97.932253940044));
#33248=CARTESIAN_POINT('Ctrl Pts',(2.83120278365768,-6.14869422146799,97.9403893293213));
#33249=CARTESIAN_POINT('Ctrl Pts',(2.98751251038381,-6.07429266339949,97.9485247185987));
#33250=CARTESIAN_POINT('Ctrl Pts',(3.14086246844589,-5.99393626545261,97.9566601078761));
#33251=CARTESIAN_POINT('Ctrl Pts',(3.29409922932973,-5.91363918358,97.9647894919147));
#33252=CARTESIAN_POINT('Ctrl Pts',(3.44438024941538,-5.8273961832761,97.9729188759533));
#33253=CARTESIAN_POINT('Ctrl Pts',(3.59121321704769,-5.73545783958892,97.9810482599919));
#33254=CARTESIAN_POINT('Ctrl Pts',(3.73796864004484,-5.64356804988408,97.9891733507841));
#33255=CARTESIAN_POINT('Ctrl Pts',(3.88127932797551,-5.54598910051285,97.9972984415762));
#33256=CARTESIAN_POINT('Ctrl Pts',(4.02067833662184,-5.44301705981341,98.0054235323684));
#33257=CARTESIAN_POINT('Ctrl Pts',(4.16060946150365,-5.33965195251193,98.0135796383935));
#33258=CARTESIAN_POINT('Ctrl Pts',(4.29659865865841,-5.23085267910821,98.0217357444186));
#33259=CARTESIAN_POINT('Ctrl Pts',(4.42820333081417,-5.11696240566278,98.0298918504437));
#33260=CARTESIAN_POINT('Ctrl Pts',(4.55927831796567,-5.00353051997053,98.0380151296171));
#33261=CARTESIAN_POINT('Ctrl Pts',(4.68600374401133,-4.885048796181,98.0461384087905));
#33262=CARTESIAN_POINT('Ctrl Pts',(4.80797609376235,-4.7618961435346,98.0542616879639));
#33263=CARTESIAN_POINT('Ctrl Pts',(4.92996468516247,-4.63872709207181,98.0623860488206));
#33264=CARTESIAN_POINT('Ctrl Pts',(5.04719868216898,-4.51088613284269,98.0705104096772));
#33265=CARTESIAN_POINT('Ctrl Pts',(5.15931210995732,-4.37878836575231,98.0786347705339));
#33266=CARTESIAN_POINT('Ctrl Pts',(5.2714617967521,-4.24664787644852,98.0867617589193));
#33267=CARTESIAN_POINT('Ctrl Pts',(5.37848737999048,-4.11024811658775,98.0948887473047));
#33268=CARTESIAN_POINT('Ctrl Pts',(5.48006381332114,-3.97003647362694,98.1030157356901));
#33269=CARTESIAN_POINT('Ctrl Pts',(5.58229692672876,-3.82891837835755,98.1111952641302));
#33270=CARTESIAN_POINT('Ctrl Pts',(5.67900996920538,-3.68393924668254,98.1193747925702));
#33271=CARTESIAN_POINT('Ctrl Pts',(5.7699168878031,-3.5355831354735,98.1275543210103));
#33272=CARTESIAN_POINT('Ctrl Pts',(5.86039569641415,-3.38792568101986,98.135695329414));
#33273=CARTESIAN_POINT('Ctrl Pts',(5.94512282658121,-3.23692333524932,98.1438363378176));
#33274=CARTESIAN_POINT('Ctrl Pts',(6.0238635010454,-3.08307598361979,98.1519773462213));
#33275=CARTESIAN_POINT('Ctrl Pts',(6.10316303016758,-2.92813671463416,98.1601761346796));
#33276=CARTESIAN_POINT('Ctrl Pts',(6.17639065570741,-2.77031224946982,98.1683749231378));
#33277=CARTESIAN_POINT('Ctrl Pts',(6.24335686394399,-2.61013104449633,98.1765737115961));
#33278=CARTESIAN_POINT('Ctrl Pts',(6.31032307218052,-2.44994983952296,98.1847725000543));
#33279=CARTESIAN_POINT('Ctrl Pts',(6.37102779387041,-2.28741226530144,98.1929712885126));
#33280=CARTESIAN_POINT('Ctrl Pts',(6.4253333466101,-2.12305920429465,98.2011700769708));
#33281=CARTESIAN_POINT('Ctrl Pts',(6.47986583521257,-1.95801933315856,98.2094031271028));
#33282=CARTESIAN_POINT('Ctrl Pts',(6.52811519062759,-1.79063577524243,98.2176361772349));
#33283=CARTESIAN_POINT('Ctrl Pts',(6.56987538026672,-1.62142729956208,98.2258692273669));
#33284=CARTESIAN_POINT('Ctrl Pts',(6.61158583993922,-1.45242032516615,98.2340924732018));
#33285=CARTESIAN_POINT('Ctrl Pts',(6.64682243641483,-1.28159310471467,98.2423157190366));
#33286=CARTESIAN_POINT('Ctrl Pts',(6.67542792079323,-1.10948234519267,98.2505389648715));
#33287=CARTESIAN_POINT('Ctrl Pts',(6.70400506588621,-0.937542094789563,
98.258754063985));
#33288=CARTESIAN_POINT('Ctrl Pts',(6.72596412360857,-0.764321188618504,
98.2669691630985));
#33289=CARTESIAN_POINT('Ctrl Pts',(6.74119817767269,-0.590369485443122,
98.275184262212));
#33290=CARTESIAN_POINT('Ctrl Pts',(6.75642018747615,-0.416555310968091,
98.2833928663509));
#33291=CARTESIAN_POINT('Ctrl Pts',(6.76492775268185,-0.242011845518606,
98.2916014704897));
#33292=CARTESIAN_POINT('Ctrl Pts',(6.76666535962014,-0.0672971835734554,
98.2998100746286));
#33293=CARTESIAN_POINT('Ctrl Pts',(6.76840194035141,0.107314294270125,98.3080138308775));
#33294=CARTESIAN_POINT('Ctrl Pts',(6.7633765243107,0.282096409987835,98.3162175871265));
#33295=CARTESIAN_POINT('Ctrl Pts',(6.75158558117908,0.456487831179224,98.3244213433754));
#33296=CARTESIAN_POINT('Ctrl Pts',(6.73979812669032,0.630827654345044,98.3326226723397));
#33297=CARTESIAN_POINT('Ctrl Pts',(6.72124915280194,0.804776656076253,98.340824001304));
#33298=CARTESIAN_POINT('Ctrl Pts',(6.69598721473029,0.977775137835097,98.3490253302683));
#33299=CARTESIAN_POINT('Ctrl Pts',(6.67072876052111,1.15074976145157,98.357225528191));
#33300=CARTESIAN_POINT('Ctrl Pts',(6.63875923692142,1.32277377165659,98.3654257261137));
#33301=CARTESIAN_POINT('Ctrl Pts',(6.60017889556942,1.49329419287695,98.3736259240364));
#33302=CARTESIAN_POINT('Ctrl Pts',(6.56159688327189,1.66382199947359,98.3818264771163));
#33303=CARTESIAN_POINT('Ctrl Pts',(6.51640356181274,1.83284573786251,98.3900270301961));
#33304=CARTESIAN_POINT('Ctrl Pts',(6.46474998749758,1.99982414205601,98.398227583276));
#33305=CARTESIAN_POINT('Ctrl Pts',(6.41308481538515,2.166840037976,98.4064299776292));
#33306=CARTESIAN_POINT('Ctrl Pts',(6.35495660724463,2.33180934281354,98.4146323719825));
#33307=CARTESIAN_POINT('Ctrl Pts',(6.29056583944162,2.49420737302459,98.4228347663357));
#33308=CARTESIAN_POINT('Ctrl Pts',(6.22611485495184,2.65675727394085,98.4310448313696));
#33309=CARTESIAN_POINT('Ctrl Pts',(6.15538974204171,2.81673076256253,98.4392548964034));
#33310=CARTESIAN_POINT('Ctrl Pts',(6.07863893984624,2.97362365456442,98.4474649614372));
#33311=CARTESIAN_POINT('Ctrl Pts',(6.00185140607834,3.13059163272124,98.4556789556625));
#33312=CARTESIAN_POINT('Ctrl Pts',(5.91903260292534,3.28447575938713,98.4638929498879));
#33313=CARTESIAN_POINT('Ctrl Pts',(5.83047619913612,3.43479785304859,98.4721069441132));
#33314=CARTESIAN_POINT('Ctrl Pts',(5.74179906347384,3.58532488579015,98.4803321367484));
#33315=CARTESIAN_POINT('Ctrl Pts',(5.64736888802309,3.7322798787694,98.4885573293835));
#33316=CARTESIAN_POINT('Ctrl Pts',(5.54752249562304,3.8752139502944,98.4967825220187));
#33317=CARTESIAN_POINT('Ctrl Pts',(5.45773084879053,4.00375425467799,98.5041794201387));
#33318=CARTESIAN_POINT('Ctrl Pts',(5.36355958090421,4.12904297003078,98.5115763182586));
#33319=CARTESIAN_POINT('Ctrl Pts',(5.26528024522293,4.25077792165919,98.5189732163786));
#33320=CARTESIAN_POINT('Ctrl Pts',(5.15038784002089,4.39309086356896,98.5276204809347));
#33321=CARTESIAN_POINT('Ctrl Pts',(5.02961995337024,4.53086980111672,98.5362677454909));
#33322=CARTESIAN_POINT('Ctrl Pts',(4.90335080295773,4.66362947747072,98.544915010047));
#33323=CARTESIAN_POINT('Ctrl Pts',(4.77367669485546,4.79996913420325,98.5537954556283));
#33324=CARTESIAN_POINT('Ctrl Pts',(4.63820061448258,4.93101474878858,98.5626759012097));
#33325=CARTESIAN_POINT('Ctrl Pts',(4.49737371021885,5.05627518145841,98.571556346791));
#33326=CARTESIAN_POINT('Ctrl Pts',(4.36064724662039,5.17788842061395,98.5801782214666));
#33327=CARTESIAN_POINT('Ctrl Pts',(4.21887741583759,5.29404839263359,98.5888000961422));
#33328=CARTESIAN_POINT('Ctrl Pts',(4.07251623075589,5.40434089878034,98.5974219708178));
#33329=CARTESIAN_POINT('Ctrl Pts',(3.91957096524828,5.5195949302826,98.606431701852));
#33330=CARTESIAN_POINT('Ctrl Pts',(3.76161192035452,5.62844114554434,98.6154414328862));
#33331=CARTESIAN_POINT('Ctrl Pts',(3.59919627489112,5.73045156814102,98.6244511639204));
#33332=CARTESIAN_POINT('Ctrl Pts',(3.43678062942783,5.83246199073764,98.6334608949546));
#33333=CARTESIAN_POINT('Ctrl Pts',(3.2699086754152,5.92763636981966,98.6424706259888));
#33334=CARTESIAN_POINT('Ctrl Pts',(3.09917575053261,6.01559628526638,98.651480357023));
#33335=CARTESIAN_POINT('Origin',(0.,0.,-3.69717978381041));
#33336=CARTESIAN_POINT('',(3.09917575053253,6.01559628526642,101.045648756765));
#33337=CARTESIAN_POINT('',(3.0991757505325,6.01559628526644,100.651392015122));
#33338=CARTESIAN_POINT('',(3.09917575053259,6.01559628526639,-3.69717978381041));
#33339=CARTESIAN_POINT('',(-6.76699843452386,0.00460295031038521,99.6971797837795));
#33340=CARTESIAN_POINT('Ctrl Pts',(-6.76699843452431,0.00460294966435506,
99.6971797838098));
#33341=CARTESIAN_POINT('Ctrl Pts',(-6.76712147278358,-0.176280998367531,
99.7056577969028));
#33342=CARTESIAN_POINT('Ctrl Pts',(-6.75998706702004,-0.357203135436458,
99.7141358099958));
#33343=CARTESIAN_POINT('Ctrl Pts',(-6.74561582556332,-0.537546401634019,
99.7226138230887));
#33344=CARTESIAN_POINT('Ctrl Pts',(-6.73162618285362,-0.713101023467001,
99.7308667199882));
#33345=CARTESIAN_POINT('Ctrl Pts',(-6.71077918971529,-0.888106761828978,
99.7391196168876));
#33346=CARTESIAN_POINT('Ctrl Pts',(-6.68314655339852,-1.06199865621265,
99.747372513787));
#33347=CARTESIAN_POINT('Ctrl Pts',(-6.65550828022493,-1.23592602327798,
99.7556270942174));
#33348=CARTESIAN_POINT('Ctrl Pts',(-6.62108166028766,-1.40873874611643,
99.7638816746477));
#33349=CARTESIAN_POINT('Ctrl Pts',(-6.57998975001323,-1.57988097327644,
99.7721362550781));
#33350=CARTESIAN_POINT('Ctrl Pts',(-6.53888239501195,-1.75108752562679,
99.7803939380592));
#33351=CARTESIAN_POINT('Ctrl Pts',(-6.49110483947996,-1.92062198926723,
99.7886516210404));
#33352=CARTESIAN_POINT('Ctrl Pts',(-6.43683037080898,-2.08794247464608,
99.7969093040216));
#33353=CARTESIAN_POINT('Ctrl Pts',(-6.38000869095953,-2.2631156506395,99.8055545368565));
#33354=CARTESIAN_POINT('Ctrl Pts',(-6.31606570320358,-2.43586160856736,
99.8141997696915));
#33355=CARTESIAN_POINT('Ctrl Pts',(-6.24525690462115,-2.60558154646557,
99.8228450025265));
#33356=CARTESIAN_POINT('Ctrl Pts',(-6.17749876946579,-2.76798942120558,
99.8311177718236));
#33357=CARTESIAN_POINT('Ctrl Pts',(-6.1034542234713,-2.92762626111469,99.8393905411208));
#33358=CARTESIAN_POINT('Ctrl Pts',(-6.02339433608997,-3.08399248895961,
99.8476633104179));
#33359=CARTESIAN_POINT('Ctrl Pts',(-5.94327424283882,-3.24047630583778,
99.8559423009238));
#33360=CARTESIAN_POINT('Ctrl Pts',(-5.85712996145528,-3.39368430193884,
99.8642212914297));
#33361=CARTESIAN_POINT('Ctrl Pts',(-5.76527650926265,-3.54314489849685,
99.8725002819356));
#33362=CARTESIAN_POINT('Ctrl Pts',(-5.67329733532742,-3.69281006490175,
99.8807906040691));
#33363=CARTESIAN_POINT('Ctrl Pts',(-5.57559358157656,-3.83871729907965,
99.8890809262026));
#33364=CARTESIAN_POINT('Ctrl Pts',(-5.47252174286387,-3.98042645628357,
99.8973712483361));
#33365=CARTESIAN_POINT('Ctrl Pts',(-5.45892503712293,-3.99911999794697,
99.8984648649045));
#33366=CARTESIAN_POINT('Ctrl Pts',(-5.44523497269768,-4.01774053746264,
99.8995584814728));
#33367=CARTESIAN_POINT('Ctrl Pts',(-5.43145241659336,-4.03628711147784,
99.9006520980411));
#33368=CARTESIAN_POINT('Ctrl Pts',(-5.32872777582496,-4.1745191011593,99.9088030802154));
#33369=CARTESIAN_POINT('Ctrl Pts',(-5.22056125470119,-4.3090441211298,99.9169540623897));
#33370=CARTESIAN_POINT('Ctrl Pts',(-5.10725086796601,-4.43940058697798,
99.925105044564));
#33371=CARTESIAN_POINT('Ctrl Pts',(-4.99407210174695,-4.56960563170927,
99.933246558617));
#33372=CARTESIAN_POINT('Ctrl Pts',(-4.87576160121589,-4.69565148783513,
99.9413880726701));
#33373=CARTESIAN_POINT('Ctrl Pts',(-4.75266032672034,-4.81710585505639,
99.9495295867231));
#33374=CARTESIAN_POINT('Ctrl Pts',(-4.6296761407412,-4.93844470022698,99.9576633569261));
#33375=CARTESIAN_POINT('Ctrl Pts',(-4.50191051119424,-5.05520049591546,
99.9657971271292));
#33376=CARTESIAN_POINT('Ctrl Pts',(-4.36974428504397,-5.16697434513909,
99.9739308973322));
#33377=CARTESIAN_POINT('Ctrl Pts',(-4.2376759723153,-5.27866538833625,99.9820586417502));
#33378=CARTESIAN_POINT('Ctrl Pts',(-4.10121383244336,-5.38538159887556,
99.9901863861682));
#33379=CARTESIAN_POINT('Ctrl Pts',(-3.96077514037961,-5.48676127486433,
99.9983141305862));
#33380=CARTESIAN_POINT('Ctrl Pts',(-3.82041096409603,-5.58808715951158,
100.00643756248));
#33381=CARTESIAN_POINT('Ctrl Pts',(-3.67607473345162,-5.68408193508003,
100.014560994374));
#33382=CARTESIAN_POINT('Ctrl Pts',(-3.52821632843498,-5.77442452022406,
100.022684426268));
#33383=CARTESIAN_POINT('Ctrl Pts',(-3.3794199678544,-5.86534020319357,100.030859390019));
#33384=CARTESIAN_POINT('Ctrl Pts',(-3.22705688234896,-5.95053149976472,
100.03903435377));
#33385=CARTESIAN_POINT('Ctrl Pts',(-3.07161512742359,-6.02971554129899,
100.047209317521));
#33386=CARTESIAN_POINT('Ctrl Pts',(-2.91718825626933,-6.10838258790662,
100.055330906694));
#33387=CARTESIAN_POINT('Ctrl Pts',(-2.75972313929371,-6.18112044471976,
100.063452495867));
#33388=CARTESIAN_POINT('Ctrl Pts',(-2.59972259339031,-6.24769809109051,
100.07157408504));
#33389=CARTESIAN_POINT('Ctrl Pts',(-2.43970092413312,-6.31428452707614,
100.079696746429));
#33390=CARTESIAN_POINT('Ctrl Pts',(-2.27714349716172,-6.37470899210375,
100.087819407819));
#33391=CARTESIAN_POINT('Ctrl Pts',(-2.1125725176687,-6.42878887175422,100.095942069208));
#33392=CARTESIAN_POINT('Ctrl Pts',(-1.94794847224879,-6.48288618946667,
100.10406734975));
#33393=CARTESIAN_POINT('Ctrl Pts',(-1.78130992892538,-6.53063473376461,
100.112192630293));
#33394=CARTESIAN_POINT('Ctrl Pts',(-1.61319358738926,-6.57190196591567,
100.120317910835));
#33395=CARTESIAN_POINT('Ctrl Pts',(-1.44324565319637,-6.61361879599802,
100.128531714623));
#33396=CARTESIAN_POINT('Ctrl Pts',(-1.27178790456063,-6.64871216986633,
100.13674551841));
#33397=CARTESIAN_POINT('Ctrl Pts',(-1.09938370566036,-6.67709850666654,
100.144959322198));
#33398=CARTESIAN_POINT('Ctrl Pts',(-0.928542451599543,-6.70522750473082,
100.153098663053));
#33399=CARTESIAN_POINT('Ctrl Pts',(-0.75677220700001,-6.72677059055827,
100.161238003909));
#33400=CARTESIAN_POINT('Ctrl Pts',(-0.584624310447284,-6.74169885233938,
100.169377344764));
#33401=CARTESIAN_POINT('Ctrl Pts',(-0.410114065865435,-6.7568319714002,
100.177628380018));
#33402=CARTESIAN_POINT('Ctrl Pts',(-0.235216121394139,-6.76516738364924,
100.185879415272));
#33403=CARTESIAN_POINT('Ctrl Pts',(-0.0605023203693838,-6.766729525349,
100.194130450526));
#33404=CARTESIAN_POINT('Ctrl Pts',(0.114211480655372,-6.76829166704876,
100.20238148578));
#33405=CARTESIAN_POINT('Ctrl Pts',(0.288740756527682,-6.76308061669069,
100.210632521034));
#33406=CARTESIAN_POINT('Ctrl Pts',(0.462521958286907,-6.75117489316508,
100.218883556288));
#33407=CARTESIAN_POINT('Ctrl Pts',(0.635897442947746,-6.73929696525575,
100.227115328319));
#33408=CARTESIAN_POINT('Ctrl Pts',(0.809069602165128,-6.72071868441591,
100.23534710035));
#33409=CARTESIAN_POINT('Ctrl Pts',(0.981480455201753,-6.69544510216139,
100.243578872381));
#33410=CARTESIAN_POINT('Ctrl Pts',(1.15368543245004,-6.67020169908979,100.251800814853));
#33411=CARTESIAN_POINT('Ctrl Pts',(1.32513056266644,-6.6382789656706,100.260022757325));
#33412=CARTESIAN_POINT('Ctrl Pts',(1.49525966648751,-6.59973389840649,100.268244699798));
#33413=CARTESIAN_POINT('Ctrl Pts',(1.66521970601936,-6.56122713496138,100.276458471788));
#33414=CARTESIAN_POINT('Ctrl Pts',(1.83386597656863,-6.5161112221054,100.284672243778));
#33415=CARTESIAN_POINT('Ctrl Pts',(2.00064911876799,-6.46449472917821,100.292886015768));
#33416=CARTESIAN_POINT('Ctrl Pts',(2.16729992602677,-6.41291919162237,100.301093270498));
#33417=CARTESIAN_POINT('Ctrl Pts',(2.33209020865481,-6.35485345290745,100.309300525228));
#33418=CARTESIAN_POINT('Ctrl Pts',(2.49448238538121,-6.29045679017215,100.317507779959));
#33419=CARTESIAN_POINT('Ctrl Pts',(2.65677822760844,-6.22609832890922,100.325710165971));
#33420=CARTESIAN_POINT('Ctrl Pts',(2.8166784657489,-6.15541655703321,100.333912551983));
#33421=CARTESIAN_POINT('Ctrl Pts',(2.97366214565786,-6.07862011014683,100.342114937995));
#33422=CARTESIAN_POINT('Ctrl Pts',(3.13059896974563,-6.00184658513734,100.350314875793));
#33423=CARTESIAN_POINT('Ctrl Pts',(3.28462064648304,-5.91896217437964,100.358514813592));
#33424=CARTESIAN_POINT('Ctrl Pts',(3.43522740073952,-5.83022312653714,100.366714751391));
#33425=CARTESIAN_POINT('Ctrl Pts',(3.58581309628472,-5.74149648670379,100.374913542626));
#33426=CARTESIAN_POINT('Ctrl Pts',(3.7329845112302,-5.64691702137982,100.383112333862));
#33427=CARTESIAN_POINT('Ctrl Pts',(3.87626761592042,-5.54678631008683,100.391311125098));
#33428=CARTESIAN_POINT('Ctrl Pts',(4.01955667823318,-5.44665143542102,100.399510257234));
#33429=CARTESIAN_POINT('Ctrl Pts',(4.1589568143405,-5.34096506020348,100.407709389371));
#33430=CARTESIAN_POINT('Ctrl Pts',(4.29402402246869,-5.23007138521663,100.415908521507));
#33431=CARTESIAN_POINT('Ctrl Pts',(4.42912134841042,-5.11915298272507,100.424109481918));
#33432=CARTESIAN_POINT('Ctrl Pts',(4.55988354506914,-5.0030251951959,100.432310442329));
#33433=CARTESIAN_POINT('Ctrl Pts',(4.68590062930382,-4.8820717213382,100.44051140274));
#33434=CARTESIAN_POINT('Ctrl Pts',(4.8120358218826,-4.76100488495828,100.448720049425));
#33435=CARTESIAN_POINT('Ctrl Pts',(4.93341675764953,-4.63510357443739,100.45692869611));
#33436=CARTESIAN_POINT('Ctrl Pts',(5.04967054633178,-4.50478816078063,100.465137342795));
#33437=CARTESIAN_POINT('Ctrl Pts',(5.16597983783781,-4.37441053088539,100.473349908519));
#33438=CARTESIAN_POINT('Ctrl Pts',(5.27715687373246,-4.23961487238904,100.481562474242));
#33439=CARTESIAN_POINT('Ctrl Pts',(5.38286992563477,-4.10085361402925,100.489775039966));
#33440=CARTESIAN_POINT('Ctrl Pts',(5.48872803109883,-3.96190195519954,100.497998874514));
#33441=CARTESIAN_POINT('Ctrl Pts',(5.58910696261734,-3.81897411506567,100.506222709063));
#33442=CARTESIAN_POINT('Ctrl Pts',(5.68371841565184,-3.67255142531458,100.514446543612));
#33443=CARTESIAN_POINT('Ctrl Pts',(5.77064854373808,-3.5380165168384,100.522002700586));
#33444=CARTESIAN_POINT('Ctrl Pts',(5.85271009104159,-3.40053169453125,100.52955885756));
#33445=CARTESIAN_POINT('Ctrl Pts',(5.92971449565611,-3.26048692682639,100.537115014535));
#33446=CARTESIAN_POINT('Ctrl Pts',(6.01782256082213,-3.10024838487717,100.545760732587));
#33447=CARTESIAN_POINT('Ctrl Pts',(6.0995104558487,-2.93629304170823,100.554406450639));
#33448=CARTESIAN_POINT('Ctrl Pts',(6.17447106581951,-2.76915078270537,100.563052168692));
#33449=CARTESIAN_POINT('Ctrl Pts',(6.24933544164374,-2.60222310030022,100.571686787404));
#33450=CARTESIAN_POINT('Ctrl Pts',(6.31748962976128,-2.43211693737029,100.580321406116));
#33451=CARTESIAN_POINT('Ctrl Pts',(6.3786722981306,-2.25938680023173,100.588956024829));
#33452=CARTESIAN_POINT('Ctrl Pts',(6.44201570067107,-2.08055650565231,100.597895584731));
#33453=CARTESIAN_POINT('Ctrl Pts',(6.49788600240192,-1.8989137845199,100.606835144634));
#33454=CARTESIAN_POINT('Ctrl Pts',(6.54604630935398,-1.71509962270219,100.615774704536));
#33455=CARTESIAN_POINT('Ctrl Pts',(6.5924346896645,-1.53804839972416,100.624385357806));
#33456=CARTESIAN_POINT('Ctrl Pts',(6.63167015877937,-1.35898299510614,100.632996011077));
#33457=CARTESIAN_POINT('Ctrl Pts',(6.66359053769349,-1.17849486463109,100.641606664347));
#33458=CARTESIAN_POINT('Ctrl Pts',(6.69548070183318,-0.998177578247951,
100.650209167058));
#33459=CARTESIAN_POINT('Ctrl Pts',(6.7200695278703,-0.816440550316719,100.658811669769));
#33460=CARTESIAN_POINT('Ctrl Pts',(6.73724540547018,-0.633887487233368,
100.66741417248));
#33461=CARTESIAN_POINT('Ctrl Pts',(6.75440195196575,-0.451539883945666,
100.676006993248));
#33462=CARTESIAN_POINT('Ctrl Pts',(6.76416216579936,-0.268378380753643,
100.684599814015));
#33463=CARTESIAN_POINT('Ctrl Pts',(6.76646596088498,-0.0850141175624732,
100.693192634783));
#33464=CARTESIAN_POINT('Ctrl Pts',(6.76673747360029,-0.0634038062546583,
100.694205337741));
#33465=CARTESIAN_POINT('Ctrl Pts',(6.76690547795264,-0.041790686436373,
100.6952180407));
#33466=CARTESIAN_POINT('Ctrl Pts',(6.76696992298183,-0.0201757641571949,
100.696230743658));
#33467=CARTESIAN_POINT('Ctrl Pts',(6.76751689643798,0.163279637956664,100.704826001418));
#33468=CARTESIAN_POINT('Ctrl Pts',(6.76059889533746,0.346649193364827,100.713421259178));
#33469=CARTESIAN_POINT('Ctrl Pts',(6.74626631702619,0.529320110857158,100.722016516938));
#33470=CARTESIAN_POINT('Ctrl Pts',(6.73192031686319,0.712162091916675,100.730619823793));
#33471=CARTESIAN_POINT('Ctrl Pts',(6.71014590400629,0.894303824750037,100.739223130647));
#33472=CARTESIAN_POINT('Ctrl Pts',(6.68104513733997,1.07513946668602,100.747826437502));
#33473=CARTESIAN_POINT('Ctrl Pts',(6.65073784279662,1.26347261704365,100.756786440442));
#33474=CARTESIAN_POINT('Ctrl Pts',(6.61248381678592,1.45038869262551,100.765746443382));
#33475=CARTESIAN_POINT('Ctrl Pts',(6.56645638204994,1.63521851219818,100.774706446322));
#33476=CARTESIAN_POINT('Ctrl Pts',(6.52214038514164,1.81317580570644,100.783333289527));
#33477=CARTESIAN_POINT('Ctrl Pts',(6.47061876047074,1.98919892111022,100.791960132731));
#33478=CARTESIAN_POINT('Ctrl Pts',(6.41209640505305,2.16270864711494,100.800586975936));
#33479=CARTESIAN_POINT('Ctrl Pts',(6.35351811705737,2.33638420455647,100.809222064222));
#33480=CARTESIAN_POINT('Ctrl Pts',(6.28792584884988,2.50754129194284,100.817857152508));
#33481=CARTESIAN_POINT('Ctrl Pts',(6.21557246644582,2.67562103339778,100.826492240794));
#33482=CARTESIAN_POINT('Ctrl Pts',(6.14311162474885,2.84395040699941,100.83514015392));
#33483=CARTESIAN_POINT('Ctrl Pts',(6.06386973016573,3.00919302443718,100.843788067045));
#33484=CARTESIAN_POINT('Ctrl Pts',(5.97814604092336,3.17081360432813,100.85243598017));
#33485=CARTESIAN_POINT('Ctrl Pts',(5.96852914797797,3.18894497301187,100.853406144374));
#33486=CARTESIAN_POINT('Ctrl Pts',(5.95883072418472,3.20703078618554,100.854376308578));
#33487=CARTESIAN_POINT('Ctrl Pts',(5.94905122609331,3.22507031075567,100.855346472781));
#33488=CARTESIAN_POINT('Ctrl Pts',(5.86615315497012,3.37798631696225,100.863570283494));
#33489=CARTESIAN_POINT('Ctrl Pts',(5.77724617322386,3.52790551519329,100.871794094208));
#33490=CARTESIAN_POINT('Ctrl Pts',(5.68257231884336,3.67432454215944,100.880017904921));
#33491=CARTESIAN_POINT('Ctrl Pts',(5.58799266104182,3.82059788823486,100.888233533281));
#33492=CARTESIAN_POINT('Ctrl Pts',(5.48765774697219,3.96337769808229,100.896449161642));
#33493=CARTESIAN_POINT('Ctrl Pts',(5.38185586416934,4.10218435194057,100.904664790003));
#33494=CARTESIAN_POINT('Ctrl Pts',(5.27614004912307,4.24087808930834,100.912873735111));
#33495=CARTESIAN_POINT('Ctrl Pts',(5.16496633698996,4.37560482318377,100.921082680219));
#33496=CARTESIAN_POINT('Ctrl Pts',(5.0486667791945,4.50591308756149,100.929291625327));
#33497=CARTESIAN_POINT('Ctrl Pts',(4.93244072621485,4.6361389931998,100.937495382135));
#33498=CARTESIAN_POINT('Ctrl Pts',(4.81109551777379,4.76195172485433,100.945699138944));
#33499=CARTESIAN_POINT('Ctrl Pts',(4.68500405485413,4.88293211154941,100.953902895752));
#33500=CARTESIAN_POINT('Ctrl Pts',(4.55896454466797,5.00386265139806,100.962103272414));
#33501=CARTESIAN_POINT('Ctrl Pts',(4.42818293267857,5.11996456382018,100.970303649076));
#33502=CARTESIAN_POINT('Ctrl Pts',(4.2930697041237,5.23085475955271,100.978504025737));
#33503=CARTESIAN_POINT('Ctrl Pts',(4.15799079295077,5.34171679030657,100.986702319587));
#33504=CARTESIAN_POINT('Ctrl Pts',(4.01858273469258,5.44736951538114,100.994900613437));
#33505=CARTESIAN_POINT('Ctrl Pts',(3.87528989711106,5.54746944230872,101.003098907287));
#33506=CARTESIAN_POINT('Ctrl Pts',(3.7319796150341,5.64758155541913,101.011298199198));
#33507=CARTESIAN_POINT('Ctrl Pts',(3.58478390008576,5.74213931093279,101.01949749111));
#33508=CARTESIAN_POINT('Ctrl Pts',(3.43417727668268,5.83084174303473,101.027696783022));
#33509=CARTESIAN_POINT('Ctrl Pts',(3.32426184422437,5.8955783792084,101.033680774269));
#33510=CARTESIAN_POINT('Ctrl Pts',(3.21253028801932,5.95719714790205,101.039664765517));
#33511=CARTESIAN_POINT('Ctrl Pts',(3.09917575053253,6.01559628526642,101.045648756765));
#33512=CARTESIAN_POINT('Ctrl Pts',(3.09917575053247,6.01559628526645,99.0459901976524));
#33513=CARTESIAN_POINT('Ctrl Pts',(2.9453019261631,6.09487055875705,99.054114251979));
#33514=CARTESIAN_POINT('Ctrl Pts',(2.78828904708904,6.16828618756218,99.0622383063056));
#33515=CARTESIAN_POINT('Ctrl Pts',(2.62862901059509,6.23559127305967,99.0703623606321));
#33516=CARTESIAN_POINT('Ctrl Pts',(2.46900589338129,6.30288079514278,99.0784845363782));
#33517=CARTESIAN_POINT('Ctrl Pts',(2.30673717191679,6.36406243989334,99.0866067121242));
#33518=CARTESIAN_POINT('Ctrl Pts',(2.14233674687458,6.41893155151158,99.0947288878703));
#33519=CARTESIAN_POINT('Ctrl Pts',(1.97795210363151,6.47379539590926,99.1028502839191));
#33520=CARTESIAN_POINT('Ctrl Pts',(1.81143651095054,6.52234779680194,99.110971679968));
#33521=CARTESIAN_POINT('Ctrl Pts',(1.64332100676458,6.56443333949902,99.1190930760168));
#33522=CARTESIAN_POINT('Ctrl Pts',(1.47518962954841,6.60652285580397,99.1272152388669));
#33523=CARTESIAN_POINT('Ctrl Pts',(1.30545839498646,6.64214420889851,99.1353374017169));
#33524=CARTESIAN_POINT('Ctrl Pts',(1.13467051781992,6.6711926831707,99.143459564567));
#33525=CARTESIAN_POINT('Ctrl Pts',(0.963833993153826,6.70024943165803,99.1515840409472));
#33526=CARTESIAN_POINT('Ctrl Pts',(0.791940587215222,6.7227295120575,99.1597085173274));
#33527=CARTESIAN_POINT('Ctrl Pts',(0.619540608498186,6.73857985293799,99.1678329937077));
#33528=CARTESIAN_POINT('Ctrl Pts',(0.446956624270756,6.75444711116431,99.1759661414836));
#33529=CARTESIAN_POINT('Ctrl Pts',(0.273865352014489,6.76367046088517,99.1840992892594));
#33530=CARTESIAN_POINT('Ctrl Pts',(0.100820022460005,6.76624891081249,99.1922324370353));
#33531=CARTESIAN_POINT('Ctrl Pts',(-0.0723196613544442,6.76882876665891,
99.2003700194708));
#33532=CARTESIAN_POINT('Ctrl Pts',(-0.245412987278003,6.76475651143226,
99.2085076019064));
#33533=CARTESIAN_POINT('Ctrl Pts',(-0.417910158476497,6.75408321679872,
99.2166451843419));
#33534=CARTESIAN_POINT('Ctrl Pts',(-0.590670436730441,6.74339364236707,
99.224795178896));
#33535=CARTESIAN_POINT('Ctrl Pts',(-0.762832379482159,6.72608294650915,
99.2329451734502));
#33536=CARTESIAN_POINT('Ctrl Pts',(-0.933853479637257,6.70225385065124,
99.2410951680044));
#33537=CARTESIAN_POINT('Ctrl Pts',(-1.09538993126271,6.67974629113467,99.2487931725187));
#33538=CARTESIAN_POINT('Ctrl Pts',(-1.2559084081125,6.65142379097088,99.2564911770331));
#33539=CARTESIAN_POINT('Ctrl Pts',(-1.41496405507995,6.61741382436007,99.2641891815474));
#33540=CARTESIAN_POINT('Ctrl Pts',(-1.58490571297841,6.58107616379215,99.272414049225));
#33541=CARTESIAN_POINT('Ctrl Pts',(-1.75368527277329,6.5381368794794,99.2806389169026));
#33542=CARTESIAN_POINT('Ctrl Pts',(-1.92075162863111,6.48868262292979,99.2888637845802));
#33543=CARTESIAN_POINT('Ctrl Pts',(-2.08762976553951,6.43928408213554,99.2970793860238));
#33544=CARTESIAN_POINT('Ctrl Pts',(-2.25279820098518,6.38338528551219,99.3052949874673));
#33545=CARTESIAN_POINT('Ctrl Pts',(-2.41571526919148,6.32112400908218,99.3135105889108));
#33546=CARTESIAN_POINT('Ctrl Pts',(-2.57848152639321,6.25892036740921,99.321718585239));
#33547=CARTESIAN_POINT('Ctrl Pts',(-2.73900023380844,6.19036610264663,99.3299265815671));
#33548=CARTESIAN_POINT('Ctrl Pts',(-2.89674407920975,6.11564900395398,99.3381345778952));
#33549=CARTESIAN_POINT('Ctrl Pts',(-3.05437358608738,6.04098606295437,99.3463366247666));
#33550=CARTESIAN_POINT('Ctrl Pts',(-3.20923191420068,5.96016933849633,99.3545386716381));
#33551=CARTESIAN_POINT('Ctrl Pts',(-3.36081088534313,5.87343504203112,99.3627407185095));
#33552=CARTESIAN_POINT('Ctrl Pts',(-3.51231042490358,5.78674619674117,99.370938467281));
#33553=CARTESIAN_POINT('Ctrl Pts',(-3.66053372030914,5.69414613483585,99.3791362160525));
#33554=CARTESIAN_POINT('Ctrl Pts',(-3.80499632793892,5.59591743544983,99.387333964824));
#33555=CARTESIAN_POINT('Ctrl Pts',(-3.94943138222869,5.4977074712147,99.3955301500396));
#33556=CARTESIAN_POINT('Ctrl Pts',(-4.09010687758579,5.39387120425928,99.4037263352552));
#33557=CARTESIAN_POINT('Ctrl Pts',(-4.22656630109052,5.28473521592956,99.4119225204709));
#33558=CARTESIAN_POINT('Ctrl Pts',(-4.36301562963498,5.17560730123402,99.4201180993512));
#33559=CARTESIAN_POINT('Ctrl Pts',(-4.49524922669044,5.06118066938256,99.4283136782316));
#33560=CARTESIAN_POINT('Ctrl Pts',(-4.62284275408058,4.94182292995659,99.4365092571119));
#33561=CARTESIAN_POINT('Ctrl Pts',(-4.7504500565209,4.82245230461952,99.4447057207904));
#33562=CARTESIAN_POINT('Ctrl Pts',(-4.87341602916203,4.6981497562585,99.4529021844689));
#33563=CARTESIAN_POINT('Ctrl Pts',(-4.9913523451223,4.56932060232614,99.4610986481473));
#33564=CARTESIAN_POINT('Ctrl Pts',(-5.10932285074251,4.44045410090732,99.4692974879751));
#33565=CARTESIAN_POINT('Ctrl Pts',(-5.22226055311114,4.30705864467148,99.477496327803));
#33566=CARTESIAN_POINT('Ctrl Pts',(-5.32981662230743,4.16957357203053,99.4856951676308));
#33567=CARTESIAN_POINT('Ctrl Pts',(-5.43748503687707,4.03194489232089,99.49390257138));
#33568=CARTESIAN_POINT('Ctrl Pts',(-5.53976036631841,3.89021834486554,99.5021099751293));
#33569=CARTESIAN_POINT('Ctrl Pts',(-5.63633586376882,3.74486408709227,99.5103173788785));
#33570=CARTESIAN_POINT('Ctrl Pts',(-5.73296309216669,3.59943196988601,99.5185291789475));
#33571=CARTESIAN_POINT('Ctrl Pts',(-5.82388421540091,3.45036857460691,99.5267409790165));
#33572=CARTESIAN_POINT('Ctrl Pts',(-5.90883796009994,3.29816963803895,99.5349527790856));
#33573=CARTESIAN_POINT('Ctrl Pts',(-5.99391676858159,3.1457466433699,99.5431766680717));
#33574=CARTESIAN_POINT('Ctrl Pts',(-6.07301047969293,2.99017920242219,99.5514005570579));
#33575=CARTESIAN_POINT('Ctrl Pts',(-6.14590503211473,2.83198522881508,99.5596244460441));
#33576=CARTESIAN_POINT('Ctrl Pts',(-6.21325833836466,2.68581673203086,99.5672231772942));
#33577=CARTESIAN_POINT('Ctrl Pts',(-6.27531960375733,2.53740626967087,99.5748219085443));
#33578=CARTESIAN_POINT('Ctrl Pts',(-6.33195787521391,2.38717374032905,99.5824206397944));
#33579=CARTESIAN_POINT('Ctrl Pts',(-6.40323906825369,2.19810098705693,99.5919839017931));
#33580=CARTESIAN_POINT('Ctrl Pts',(-6.46610086863492,2.00569185012578,99.6015471637919));
#33581=CARTESIAN_POINT('Ctrl Pts',(-6.52026103456438,1.81065873127475,99.6111104257907));
#33582=CARTESIAN_POINT('Ctrl Pts',(-6.57312998749973,1.6202753267113,99.6204456935072));
#33583=CARTESIAN_POINT('Ctrl Pts',(-6.61770733335403,1.42739178948677,99.6297809612236));
#33584=CARTESIAN_POINT('Ctrl Pts',(-6.65377763927682,1.23269303845678,99.6391162289401));
#33585=CARTESIAN_POINT('Ctrl Pts',(-6.69116935725116,1.03086162610188,99.64879348808));
#33586=CARTESIAN_POINT('Ctrl Pts',(-6.71941885109214,0.827079589550037,
99.6584707472199));
#33587=CARTESIAN_POINT('Ctrl Pts',(-6.73834104999955,0.622132537238636,
99.6681480063598));
#33588=CARTESIAN_POINT('Ctrl Pts',(-6.75726324890696,0.417185484927235,
99.6778252654997));
#33589=CARTESIAN_POINT('Ctrl Pts',(-6.76685799203185,0.211073596220982,
99.6875025246397));
#33590=CARTESIAN_POINT('Ctrl Pts',(-6.76699843452387,0.0046029503101877,
99.6971797837796));
#33591=CARTESIAN_POINT('',(-6.767,5.7588601855979E-12,99.3028202161897));
#33592=CARTESIAN_POINT('Ctrl Pts',(3.09917575053261,6.01559628526638,98.651480357023));
#33593=CARTESIAN_POINT('Ctrl Pts',(2.93245238380909,6.10149051597834,98.6602785000427));
#33594=CARTESIAN_POINT('Ctrl Pts',(2.76204767700999,6.18050514918712,98.6690766430624));
#33595=CARTESIAN_POINT('Ctrl Pts',(2.58854694694294,6.25233665947959,98.6778747860822));
#33596=CARTESIAN_POINT('Ctrl Pts',(2.41903728943524,6.3225158149404,98.6864705436297));
#33597=CARTESIAN_POINT('Ctrl Pts',(2.24677147783188,6.38575632069298,98.6950663011773));
#33598=CARTESIAN_POINT('Ctrl Pts',(2.07233554270395,6.4418719638352,98.7036620587248));
#33599=CARTESIAN_POINT('Ctrl Pts',(1.89773685291709,6.4980399647806,98.7122658364065));
#33600=CARTESIAN_POINT('Ctrl Pts',(1.72096428866876,6.5470697404895,98.7208696140881));
#33601=CARTESIAN_POINT('Ctrl Pts',(1.54261708282097,6.58882550503418,98.7294733917698));
#33602=CARTESIAN_POINT('Ctrl Pts',(1.35726067582878,6.63222230763853,98.7384153054378));
#33603=CARTESIAN_POINT('Ctrl Pts',(1.17020372440459,6.66776171376448,98.7473572191058));
#33604=CARTESIAN_POINT('Ctrl Pts',(0.982126885110365,6.69535031059193,98.7562991327739));
#33605=CARTESIAN_POINT('Ctrl Pts',(0.800669424599743,6.72196792463811,98.7649263351046));
#33606=CARTESIAN_POINT('Ctrl Pts',(0.618262942848151,6.74118486718215,98.7735535374353));
#33607=CARTESIAN_POINT('Ctrl Pts',(0.43552110515076,6.75297048468067,98.782180739766));
#33608=CARTESIAN_POINT('Ctrl Pts',(0.252605233822827,6.76476732617599,98.7908161581865));
#33609=CARTESIAN_POINT('Ctrl Pts',(0.0693536736601038,6.76911870559685,
98.7994515766069));
#33610=CARTESIAN_POINT('Ctrl Pts',(-0.113620481361248,6.76604606740268,
98.8080869950274));
#33611=CARTESIAN_POINT('Ctrl Pts',(-0.296864954634215,6.76296888982324,
98.8167351710485));
#33612=CARTESIAN_POINT('Ctrl Pts',(-0.47983089916059,6.75244579019949,98.8253833470697));
#33613=CARTESIAN_POINT('Ctrl Pts',(-0.661909413332708,6.73455009102624,
98.8340315230909));
#33614=CARTESIAN_POINT('Ctrl Pts',(-0.681172629746129,6.73265679390873,
98.8349464673227));
#33615=CARTESIAN_POINT('Ctrl Pts',(-0.700425922149364,6.73068102372902,
98.8358614115545));
#33616=CARTESIAN_POINT('Ctrl Pts',(-0.71966857618888,6.72862290074621,98.8367763557863));
#33617=CARTESIAN_POINT('Ctrl Pts',(-0.892673578136568,6.7101189267144,98.8450023483276));
#33618=CARTESIAN_POINT('Ctrl Pts',(-1.06519153420927,6.68491397747257,98.853228340869));
#33619=CARTESIAN_POINT('Ctrl Pts',(-1.23666451091438,6.65304064976646,98.8614543334104));
#33620=CARTESIAN_POINT('Ctrl Pts',(-1.4079577203671,6.62120073712467,98.8696717020618));
#33621=CARTESIAN_POINT('Ctrl Pts',(-1.57820778268713,6.58270643249318,98.8778890707133));
#33622=CARTESIAN_POINT('Ctrl Pts',(-1.74686124829024,6.53764214218107,98.8861064393647));
#33623=CARTESIAN_POINT('Ctrl Pts',(-1.91537164936142,6.4926160787834,98.8943168374271));
#33624=CARTESIAN_POINT('Ctrl Pts',(-2.08228780689118,6.44103122136321,98.9025272354895));
#33625=CARTESIAN_POINT('Ctrl Pts',(-2.2470657452993,6.38302315022455,98.9107376335518));
#33626=CARTESIAN_POINT('Ctrl Pts',(-2.4117368687555,6.3250526819919,98.9189427093406));
#33627=CARTESIAN_POINT('Ctrl Pts',(-2.57427219729211,6.26066741249165,98.9271477851294));
#33628=CARTESIAN_POINT('Ctrl Pts',(-2.73414213310794,6.19005297198368,98.9353528609181));
#33629=CARTESIAN_POINT('Ctrl Pts',(-2.89394040928929,6.11947018348689,98.9435542588876));
#33630=CARTESIAN_POINT('Ctrl Pts',(-3.05107534594188,6.04266393121495,98.9517556568572));
#33631=CARTESIAN_POINT('Ctrl Pts',(-3.20503649257048,5.95986829395512,98.9599570548266));
#33632=CARTESIAN_POINT('Ctrl Pts',(-3.35898557968034,5.87707914193888,98.9681578103944));
#33633=CARTESIAN_POINT('Ctrl Pts',(-3.50976105251121,5.78830170128249,98.9763585659621));
#33634=CARTESIAN_POINT('Ctrl Pts',(-3.65687595058967,5.69381658310126,98.9845593215298));
#33635=CARTESIAN_POINT('Ctrl Pts',(-3.80399010139447,5.59933194485946,98.9927600354416));
#33636=CARTESIAN_POINT('Ctrl Pts',(-3.94744341236865,5.49913987960917,99.0009607493534));
#33637=CARTESIAN_POINT('Ctrl Pts',(-4.08677698325455,5.39356495178661,99.0091614632652));
#33638=CARTESIAN_POINT('Ctrl Pts',(-4.22613509710495,5.28797142742848,99.0173636216948));
#33639=CARTESIAN_POINT('Ctrl Pts',(-4.36137173944622,5.1769933678733,99.0255657801245));
#33640=CARTESIAN_POINT('Ctrl Pts',(-4.49206020250443,5.06099635813699,99.0337679385541));
#33641=CARTESIAN_POINT('Ctrl Pts',(-4.62279536998506,4.94495789429513,99.0419730282071));
#33642=CARTESIAN_POINT('Ctrl Pts',(-4.74897885245106,4.82389714499411,99.05017811786));
#33643=CARTESIAN_POINT('Ctrl Pts',(-4.87021995362528,4.69821738570175,99.058383207513));
#33644=CARTESIAN_POINT('Ctrl Pts',(-4.9915995584228,4.57239405214399,99.0665976705108));
#33645=CARTESIAN_POINT('Ctrl Pts',(-5.10802525297673,4.44194142491324,99.0748121335086));
#33646=CARTESIAN_POINT('Ctrl Pts',(-5.21914519615482,4.30729757753677,99.0830265965063));
#33647=CARTESIAN_POINT('Ctrl Pts',(-5.33033097438728,4.17257395793616,99.0912459263138));
#33648=CARTESIAN_POINT('Ctrl Pts',(-5.43620451819687,4.03365445283905,99.0994652561213));
#33649=CARTESIAN_POINT('Ctrl Pts',(-5.5364567655613,3.89100700115928,99.1076845859288));
#33650=CARTESIAN_POINT('Ctrl Pts',(-5.63686434770489,3.74813852590161,99.1159166510895));
#33651=CARTESIAN_POINT('Ctrl Pts',(-5.7316330332971,3.60153086166351,99.1241487162502));
#33652=CARTESIAN_POINT('Ctrl Pts',(-5.82049857341232,3.45167862885657,99.1323807814109));
#33653=CARTESIAN_POINT('Ctrl Pts',(-5.90037730176227,3.31698068203152,99.1397803526719));
#33654=CARTESIAN_POINT('Ctrl Pts',(-5.97548700482453,3.17966170855554,99.1471799239329));
#33655=CARTESIAN_POINT('Ctrl Pts',(-6.04566906188862,3.04009450414338,99.1545794951939));
#33656=CARTESIAN_POINT('Ctrl Pts',(-6.12835566695495,2.87566019152554,99.163297470302));
#33657=CARTESIAN_POINT('Ctrl Pts',(-6.20443031847366,2.7076506828572,99.1720154454101));
#33658=CARTESIAN_POINT('Ctrl Pts',(-6.27358858800675,2.53660703074629,99.1807334205182));
#33659=CARTESIAN_POINT('Ctrl Pts',(-6.34261135922391,2.36589849585226,99.1894343149365));
#33660=CARTESIAN_POINT('Ctrl Pts',(-6.40474465693939,2.19216793913221,99.1981352093549));
#33661=CARTESIAN_POINT('Ctrl Pts',(-6.45972999030447,2.01598051884464,99.2068361037733));
#33662=CARTESIAN_POINT('Ctrl Pts',(-6.51456218618164,1.84028379120709,99.215512765673));
#33663=CARTESIAN_POINT('Ctrl Pts',(-6.56228603910053,1.66214412621012,99.2241894275727));
#33664=CARTESIAN_POINT('Ctrl Pts',(-6.6026914331339,1.48214535009902,99.2328660894725));
#33665=CARTESIAN_POINT('Ctrl Pts',(-6.64302991800459,1.30244464229498,99.2415283832861));
#33666=CARTESIAN_POINT('Ctrl Pts',(-6.67607403775892,1.12089124316773,99.2501906770997));
#33667=CARTESIAN_POINT('Ctrl Pts',(-6.7016628272348,0.93808547055124,99.2588529709132));
#33668=CARTESIAN_POINT('Ctrl Pts',(-6.72719076008196,0.755714456407419,
99.2674946635961));
#33669=CARTESIAN_POINT('Ctrl Pts',(-6.74529868753324,0.572097297730524,
99.2761363562789));
#33670=CARTESIAN_POINT('Ctrl Pts',(-6.75587633535769,0.387845254391387,
99.2847780489617));
#33671=CARTESIAN_POINT('Ctrl Pts',(-6.76323768989523,0.259617822565879,
99.2907921047043));
#33672=CARTESIAN_POINT('Ctrl Pts',(-6.76695297056617,0.131083220982737,
99.296806160447));
#33673=CARTESIAN_POINT('Ctrl Pts',(-6.76699955621847,0.00245074255190249,
99.3028202161897));
#33674=CARTESIAN_POINT('Ctrl Pts',(-6.767,5.7588599325272E-12,99.3028202161897));
#33675=CARTESIAN_POINT('Ctrl Pts',(-6.76700000000016,-0.186007249409913,
99.3115697279957));
#33676=CARTESIAN_POINT('Ctrl Pts',(-6.7593263729547,-0.372014355521765,
99.3203192398016));
#33677=CARTESIAN_POINT('Ctrl Pts',(-6.74400518266976,-0.557389537149286,
99.3290687516076));
#33678=CARTESIAN_POINT('Ctrl Pts',(-6.72868405709709,-0.742763935805651,
99.3378182264581));
#33679=CARTESIAN_POINT('Ctrl Pts',(-6.7057154565307,-0.927506129689313,
99.3465677013087));
#33680=CARTESIAN_POINT('Ctrl Pts',(-6.67517739415745,-1.11098863924406,
99.3553171761592));
#33681=CARTESIAN_POINT('Ctrl Pts',(-6.64463945823175,-1.29447038906122,
99.3640666147812));
#33682=CARTESIAN_POINT('Ctrl Pts',(-6.60653217027237,-1.47669218227862,
99.3728160534032));
#33683=CARTESIAN_POINT('Ctrl Pts',(-6.56098496116795,-1.65703510503792,
99.3815654920252));
#33684=CARTESIAN_POINT('Ctrl Pts',(-6.51543793687602,-1.8373772960372,99.3903148951455));
#33685=CARTESIAN_POINT('Ctrl Pts',(-6.46245112202725,-2.01584035396781,
99.3990642982657));
#33686=CARTESIAN_POINT('Ctrl Pts',(-6.40220448416326,-2.19181813637899,
99.4078137013859));
#33687=CARTESIAN_POINT('Ctrl Pts',(-6.34195808575275,-2.36779521935709,
99.4165630697312));
#33688=CARTESIAN_POINT('Ctrl Pts',(-6.27445201489326,-2.54128677544603,
99.4253124380765));
#33689=CARTESIAN_POINT('Ctrl Pts',(-6.19991555136278,-2.71170355237626,
99.4340618064218));
#33690=CARTESIAN_POINT('Ctrl Pts',(-6.12537937789138,-2.88211966612859,
99.4428111407188));
#33691=CARTESIAN_POINT('Ctrl Pts',(-6.04381298133723,-3.04946076210234,
99.4515604750159));
#33692=CARTESIAN_POINT('Ctrl Pts',(-5.95549339426418,-3.21315848206647,
99.4603098093129));
#33693=CARTESIAN_POINT('Ctrl Pts',(-5.86717414355284,-3.37685557859421,
99.4690591102885));
#33694=CARTESIAN_POINT('Ctrl Pts',(-5.77210188986374,-3.5369090746709,99.4778084112641));
#33695=CARTESIAN_POINT('Ctrl Pts',(-5.67059953467216,-3.69277536784678,
99.4865577122396));
#33696=CARTESIAN_POINT('Ctrl Pts',(-5.56909755761921,-3.84864108035569,
99.4953069806204));
#33697=CARTESIAN_POINT('Ctrl Pts',(-5.46116568338232,-4.00031938104058,
99.5040562490011));
#33698=CARTESIAN_POINT('Ctrl Pts',(-5.34717048686283,-4.14729511663001,
99.5128055173819));
#33699=CARTESIAN_POINT('Ctrl Pts',(-5.23317570555686,-4.29427031687835,
99.5215547538945));
#33700=CARTESIAN_POINT('Ctrl Pts',(-5.11311782178972,-4.43654275986937,
99.5303039904071));
#33701=CARTESIAN_POINT('Ctrl Pts',(-4.98740459172179,-4.57362924147469,
99.5390532269198));
#33702=CARTESIAN_POINT('Ctrl Pts',(-4.86169180910972,-4.71071523514291,
99.5478024322909));
#33703=CARTESIAN_POINT('Ctrl Pts',(-4.73032391415547,-4.84261509316412,
99.5565516376621));
#33704=CARTESIAN_POINT('Ctrl Pts',(-4.59374707237381,-4.96888084331443,
99.5653008430332));
#33705=CARTESIAN_POINT('Ctrl Pts',(-4.45717070537491,-5.09514615452647,
99.5740500179894));
#33706=CARTESIAN_POINT('Ctrl Pts',(-4.31538563819599,-5.21577720253558,
99.5827991929456));
#33707=CARTESIAN_POINT('Ctrl Pts',(-4.16887341290739,-5.33036429028579,
99.5915483679019));
#33708=CARTESIAN_POINT('Ctrl Pts',(-4.02236168477423,-5.44495098921114,
99.6002975131698));
#33709=CARTESIAN_POINT('Ctrl Pts',(-3.87112305634517,-5.55349359238705,
99.6090466584377));
#33710=CARTESIAN_POINT('Ctrl Pts',(-3.71567117316803,-5.65562346102427,
99.6177958037056));
#33711=CARTESIAN_POINT('Ctrl Pts',(-3.56021980457389,-5.75775299158714,
99.6265449200118));
#33712=CARTESIAN_POINT('Ctrl Pts',(-3.40055544862494,-5.85346967275291,
99.635294036318));
#33713=CARTESIAN_POINT('Ctrl Pts',(-3.23722036323528,-5.94244842803493,
99.6440431526241));
#33714=CARTESIAN_POINT('Ctrl Pts',(-3.07388580496189,-6.03142689616402,
99.6527922406951));
#33715=CARTESIAN_POINT('Ctrl Pts',(-2.90688079257867,-6.11366734484746,
99.661541328766));
#33716=CARTESIAN_POINT('Ctrl Pts',(-2.73677251094793,-6.18889046787223,
99.6702904168369));
#33717=CARTESIAN_POINT('Ctrl Pts',(-2.56666476416847,-6.26411335438187,
99.6790394773992));
#33718=CARTESIAN_POINT('Ctrl Pts',(-2.39345402972319,-6.33231884350204,
99.6877885379614));
#33719=CARTESIAN_POINT('Ctrl Pts',(-2.2177285647429,-6.39327529620956,99.6965375985236));
#33720=CARTESIAN_POINT('Ctrl Pts',(-2.04200363768508,-6.45423156232007,
99.7052866323036));
#33721=CARTESIAN_POINT('Ctrl Pts',(-1.86376426620317,-6.50793874251992,
99.7140356660836));
#33722=CARTESIAN_POINT('Ctrl Pts',(-1.68361578194898,-6.55421443796069,
99.7227846998636));
#33723=CARTESIAN_POINT('Ctrl Pts',(-1.50346783420054,-6.60048999558638,
99.7315337075879));
#33724=CARTESIAN_POINT('Ctrl Pts',(-1.32141106257408,-6.63933404145464,
99.7402827153121));
#33725=CARTESIAN_POINT('Ctrl Pts',(-1.13806375959181,-6.67061465527006,
99.7490317230363));
#33726=CARTESIAN_POINT('Ctrl Pts',(-0.95471698742034,-6.70189517852464,
99.7577807054312));
#33727=CARTESIAN_POINT('Ctrl Pts',(-0.770079973810876,-6.72561226535817,
99.7665296878261));
#33728=CARTESIAN_POINT('Ctrl Pts',(-0.584779770553267,-6.74168536939775,
99.775278670221));
#33729=CARTESIAN_POINT('Ctrl Pts',(-0.391490647554711,-6.75845143942389,
99.7844048508971));
#33730=CARTESIAN_POINT('Ctrl Pts',(-0.197480213105126,-6.76689975924024,
99.7935310315731));
#33731=CARTESIAN_POINT('Ctrl Pts',(-0.00346532629857358,-6.76699911271707,
99.8026572122492));
#33732=CARTESIAN_POINT('Ctrl Pts',(0.184486595295242,-6.76709536139775,
99.8114981997791));
#33733=CARTESIAN_POINT('Ctrl Pts',(0.372442378184379,-6.75935659726775,
99.820339187309));
#33734=CARTESIAN_POINT('Ctrl Pts',(0.559750217721202,-6.74380965729024,
99.829180174839));
#33735=CARTESIAN_POINT('Ctrl Pts',(0.745129914456873,-6.72842275717263,
99.8379301534367));
#33736=CARTESIAN_POINT('Ctrl Pts',(0.929874656313306,-6.70538772273485,
99.8466801320345));
#33737=CARTESIAN_POINT('Ctrl Pts',(1.1133568828969,-6.67478280180757,99.8554301106323));
#33738=CARTESIAN_POINT('Ctrl Pts',(1.29683723118757,-6.64417819418043,99.8641799996572));
#33739=CARTESIAN_POINT('Ctrl Pts',(1.47905480730123,-6.606003902301,99.8729298886822));
#33740=CARTESIAN_POINT('Ctrl Pts',(1.65939064804684,-6.56038959797166,99.8816797777071));
#33741=CARTESIAN_POINT('Ctrl Pts',(1.83972470264148,-6.51477574543289,99.8904295800681));
#33742=CARTESIAN_POINT('Ctrl Pts',(2.01817678125737,-6.46172209820135,99.899179382429));
#33743=CARTESIAN_POINT('Ctrl Pts',(2.19414072347575,-6.4014088672405,99.9079291847899));
#33744=CARTESIAN_POINT('Ctrl Pts',(2.37010298132,-6.34109621361411,99.9166789033954));
#33745=CARTESIAN_POINT('Ctrl Pts',(2.54357687926824,-6.27352420826007,99.9254286220009));
#33746=CARTESIAN_POINT('Ctrl Pts',(2.71397317789891,-6.19892237325532,99.9341783406064));
#33747=CARTESIAN_POINT('Ctrl Pts',(2.88436790207115,-6.12432122757004,99.9429279783647));
#33748=CARTESIAN_POINT('Ctrl Pts',(3.05168482126165,-6.04269049717463,99.9516776161229));
#33749=CARTESIAN_POINT('Ctrl Pts',(3.21535561997292,-5.95430745234982,99.9604272538812));
#33750=CARTESIAN_POINT('Ctrl Pts',(3.37902496075184,-5.86592519481572,99.9691768137002));
#33751=CARTESIAN_POINT('Ctrl Pts',(3.53904799384779,-5.77079087940291,99.9779263735192));
#33752=CARTESIAN_POINT('Ctrl Pts',(3.69488118814889,-5.66922763747086,99.9866759333382));
#33753=CARTESIAN_POINT('Ctrl Pts',(3.85071304610742,-5.56766526649115,99.9954254181257));
#33754=CARTESIAN_POINT('Ctrl Pts',(4.00235489705881,-5.45967423580778,100.004174902913));
#33755=CARTESIAN_POINT('Ctrl Pts',(4.14929168607571,-5.34562133936393,100.012924387701));
#33756=CARTESIAN_POINT('Ctrl Pts',(4.29622726385676,-5.23156938308597,100.021673800364));
#33757=CARTESIAN_POINT('Ctrl Pts',(4.43845763091988,-5.11145583677271,100.030423213027));
#33758=CARTESIAN_POINT('Ctrl Pts',(4.57549970660886,-4.98568866204282,100.03917262569));
#33759=CARTESIAN_POINT('Ctrl Pts',(4.71254069815223,-4.85992248226231,100.047921969137));
#33760=CARTESIAN_POINT('Ctrl Pts',(4.84439326931247,-4.72850295734071,100.056671312583));
#33761=CARTESIAN_POINT('Ctrl Pts',(4.97060959434635,-4.59187644221749,100.065420656029));
#33762=CARTESIAN_POINT('Ctrl Pts',(5.09682496280459,-4.45525096256728,100.074169933166));
#33763=CARTESIAN_POINT('Ctrl Pts',(5.2174039761579,-4.31341878218386,100.082919210302));
#33764=CARTESIAN_POINT('Ctrl Pts',(5.3319371045189,-4.16686161438733,100.091668487438));
#33765=CARTESIAN_POINT('Ctrl Pts',(5.44646940289338,-4.02030550864575,100.100417701171));
#33766=CARTESIAN_POINT('Ctrl Pts',(5.55495572749618,-3.869024709802,100.109166914904));
#33767=CARTESIAN_POINT('Ctrl Pts',(5.65702762491408,-3.71353301465854,100.117916128637));
#33768=CARTESIAN_POINT('Ctrl Pts',(5.7590988165511,-3.55804239466964,100.126665281873));
#33769=CARTESIAN_POINT('Ctrl Pts',(5.85475551250742,-3.39834117619623,100.135414435109));
#33770=CARTESIAN_POINT('Ctrl Pts',(5.94367283728058,-3.23497174692037,100.144163588346));
#33771=CARTESIAN_POINT('Ctrl Pts',(6.03258957676285,-3.0716033930102,100.152912683991));
#33772=CARTESIAN_POINT('Ctrl Pts',(6.11476689685266,-2.90456712829543,100.161661779637));
#33773=CARTESIAN_POINT('Ctrl Pts',(6.1899257052525,-2.73443024475929,100.170410875282));
#33774=CARTESIAN_POINT('Ctrl Pts',(6.2650840438869,-2.56429442463048,100.179159916243));
#33775=CARTESIAN_POINT('Ctrl Pts',(6.33322384283311,-2.39105828656004,100.187908957204));
#33776=CARTESIAN_POINT('Ctrl Pts',(6.39411368720031,-2.21531017132087,100.196657998165));
#33777=CARTESIAN_POINT('Ctrl Pts',(6.45500317120883,-2.03956309619536,100.205406987348));
#33778=CARTESIAN_POINT('Ctrl Pts',(6.50864269270062,-1.8613043443867,100.21415597653));
#33779=CARTESIAN_POINT('Ctrl Pts',(6.5548500844632,-1.68113930719997,100.222904965713));
#33780=CARTESIAN_POINT('Ctrl Pts',(6.60199664749393,-1.49731239211887,100.231831779242));
#33781=CARTESIAN_POINT('Ctrl Pts',(6.64140563640898,-1.31150116499713,100.240758592771));
#33782=CARTESIAN_POINT('Ctrl Pts',(6.67293772282166,-1.12436255155696,100.249685406301));
#33783=CARTESIAN_POINT('Ctrl Pts',(6.70384494949865,-0.940932395051767,
100.258435320456));
#33784=CARTESIAN_POINT('Ctrl Pts',(6.72718449348925,-0.756227260507198,
100.267185234612));
#33785=CARTESIAN_POINT('Ctrl Pts',(6.74287707373928,-0.570874564542234,
100.275935148767));
#33786=CARTESIAN_POINT('Ctrl Pts',(6.75856934538666,-0.385525513633097,
100.284684890851));
#33787=CARTESIAN_POINT('Ctrl Pts',(6.76661493004101,-0.199529212418929,
100.293434632935));
#33788=CARTESIAN_POINT('Ctrl Pts',(6.76698649908906,-0.0135174386012057,
100.302184375019));
#33789=CARTESIAN_POINT('Ctrl Pts',(6.76735806132391,0.17249092444508,100.310933956665));
#33790=CARTESIAN_POINT('Ctrl Pts',(6.76005588896293,0.35851447290079,100.319683538311));
#33791=CARTESIAN_POINT('Ctrl Pts',(6.74510478454589,0.543921359661676,100.328433119957));
#33792=CARTESIAN_POINT('Ctrl Pts',(6.73015393440693,0.729325093149969,100.337182552796));
#33793=CARTESIAN_POINT('Ctrl Pts',(6.70755443556903,0.914111900255936,100.345931985635));
#33794=CARTESIAN_POINT('Ctrl Pts',(6.67738304682325,1.09765415591502,100.354681418474));
#33795=CARTESIAN_POINT('Ctrl Pts',(6.64721213111866,1.28119353391246,100.363430714135));
#33796=CARTESIAN_POINT('Ctrl Pts',(6.60946960955499,1.46348811672634,100.372180009797));
#33797=CARTESIAN_POINT('Ctrl Pts',(6.56428366991186,1.64391876348211,100.380929305458));
#33798=CARTESIAN_POINT('Ctrl Pts',(6.51909837867721,1.82434682109703,100.389678475569));
#33799=CARTESIAN_POINT('Ctrl Pts',(6.46646995271926,2.0029107182043,100.39842764568));
#33800=CARTESIAN_POINT('Ctrl Pts',(6.40657713281555,2.17900400212686,100.40717681579));
#33801=CARTESIAN_POINT('Ctrl Pts',(6.34668509279062,2.35509499309652,100.415925871976));
#33802=CARTESIAN_POINT('Ctrl Pts',(6.27952894037524,2.52871516398128,100.424674928162));
#33803=CARTESIAN_POINT('Ctrl Pts',(6.2053367506144,2.69927486771436,100.433423984348));
#33804=CARTESIAN_POINT('Ctrl Pts',(6.12832117907908,2.87632521635941,100.44250598563));
#33805=CARTESIAN_POINT('Ctrl Pts',(6.0437236662607,3.05007728920016,100.451587986912));
#33806=CARTESIAN_POINT('Ctrl Pts',(5.95185378007857,3.21989527478216,100.460669988195));
#33807=CARTESIAN_POINT('Ctrl Pts',(5.86334450817362,3.38350129286768,100.469419768502));
#33808=CARTESIAN_POINT('Ctrl Pts',(5.76808562057248,3.54345567124974,100.478169548809));
#33809=CARTESIAN_POINT('Ctrl Pts',(5.66640068804479,3.69921508465317,100.486919329116));
#33810=CARTESIAN_POINT('Ctrl Pts',(5.56471941107921,3.85496889852286,100.495668794869));
#33811=CARTESIAN_POINT('Ctrl Pts',(5.45661270815116,4.00652780919634,100.504418260623));
#33812=CARTESIAN_POINT('Ctrl Pts',(5.3424477644912,4.15337704569221,100.513167726376));
#33813=CARTESIAN_POINT('Ctrl Pts',(5.22828631819602,4.30022178356241,100.521916924096));
#33814=CARTESIAN_POINT('Ctrl Pts',(5.10806717844077,4.4423569097267,100.530666121816));
#33815=CARTESIAN_POINT('Ctrl Pts',(4.98219864544728,4.57929969070635,100.539415319535));
#33816=CARTESIAN_POINT('Ctrl Pts',(4.85633329944035,4.7162390042999,100.548164295725));
#33817=CARTESIAN_POINT('Ctrl Pts',(4.7248190403366,4.84798602483605,100.556913271916));
#33818=CARTESIAN_POINT('Ctrl Pts',(4.58810250737212,4.97409332259114,100.565662248106));
#33819=CARTESIAN_POINT('Ctrl Pts',(4.45137708685659,5.1002088182212,100.574411793042));
#33820=CARTESIAN_POINT('Ctrl Pts',(4.30944892636073,5.22068366307915,100.583161337978));
#33821=CARTESIAN_POINT('Ctrl Pts',(4.16280009466687,5.3351086560483,100.591910882914));
#33822=CARTESIAN_POINT('Ctrl Pts',(4.01615988348822,5.44952692272866,100.600659913523));
#33823=CARTESIAN_POINT('Ctrl Pts',(3.86479978232272,5.55789587288597,100.609408944131));
#33824=CARTESIAN_POINT('Ctrl Pts',(3.70923383581116,5.65984746713846,100.618157974739));
#33825=CARTESIAN_POINT('Ctrl Pts',(3.55366577799593,5.7618004450535,100.626907124087));
#33826=CARTESIAN_POINT('Ctrl Pts',(3.39389200026896,5.85733573571026,100.635656273435));
#33827=CARTESIAN_POINT('Ctrl Pts',(3.23045513626101,5.94612887621895,100.644405422783));
#33828=CARTESIAN_POINT('Ctrl Pts',(3.18695122151616,5.96976399206668,100.646734286896));
#33829=CARTESIAN_POINT('Ctrl Pts',(3.14318791262679,5.99292165435326,100.649063151009));
#33830=CARTESIAN_POINT('Ctrl Pts',(3.0991757505325,6.01559628526644,100.651392015122));
#33831=CARTESIAN_POINT('Origin',(0.,0.,-3.69717978381041));
#33832=CARTESIAN_POINT('',(3.09917575053265,6.01559628526636,103.045648009871));
#33833=CARTESIAN_POINT('',(3.09917575053253,6.01559628526642,102.651329234227));
#33834=CARTESIAN_POINT('',(3.09917575053259,6.01559628526639,-3.69717978381041));
#33835=CARTESIAN_POINT('',(-6.76699833621906,-0.00474527222232697,101.69717978384));
#33836=CARTESIAN_POINT('Ctrl Pts',(-6.76699833621906,-0.00474527222232863,
101.69717978384));
#33837=CARTESIAN_POINT('Ctrl Pts',(-6.76685764347592,-0.20538024407743,
101.70658487248));
#33838=CARTESIAN_POINT('Ctrl Pts',(-6.75778988930074,-0.405671385327906,
101.715989961121));
#33839=CARTESIAN_POINT('Ctrl Pts',(-6.73991149079066,-0.604881886245581,
101.725395049761));
#33840=CARTESIAN_POINT('Ctrl Pts',(-6.72212131116182,-0.80310940608071,
101.734753730083));
#33841=CARTESIAN_POINT('Ctrl Pts',(-6.69560740036752,-1.0002668010555,101.744112410406));
#33842=CARTESIAN_POINT('Ctrl Pts',(-6.6605344896149,-1.19564598132158,101.753471090728));
#33843=CARTESIAN_POINT('Ctrl Pts',(-6.62520069676219,-1.39247844646671,
101.762899383527));
#33844=CARTESIAN_POINT('Ctrl Pts',(-6.58118016988564,-1.58750599058811,
101.772327676326));
#33845=CARTESIAN_POINT('Ctrl Pts',(-6.52869054886016,-1.78002492039412,
101.781755969125));
#33846=CARTESIAN_POINT('Ctrl Pts',(-6.47620092783464,-1.97254385020025,
101.791184261924));
#33847=CARTESIAN_POINT('Ctrl Pts',(-6.41524233215604,-2.16255404287778,
101.800612554723));
#33848=CARTESIAN_POINT('Ctrl Pts',(-6.34607992290035,-2.3493740894462,101.810040847522));
#33849=CARTESIAN_POINT('Ctrl Pts',(-6.28574552961825,-2.51234808477026,
101.818265695844));
#33850=CARTESIAN_POINT('Ctrl Pts',(-6.21904440781394,-2.67322514300025,
101.826490544166));
#33851=CARTESIAN_POINT('Ctrl Pts',(-6.1461413664766,-2.83147228545241,101.834715392488));
#33852=CARTESIAN_POINT('Ctrl Pts',(-6.07332043012784,-2.9895412065357,101.842930977807));
#33853=CARTESIAN_POINT('Ctrl Pts',(-5.99431163138863,-3.14498578679159,
101.851146563126));
#33854=CARTESIAN_POINT('Ctrl Pts',(-5.90932902089302,-3.29728972382343,
101.859362148446));
#33855=CARTESIAN_POINT('Ctrl Pts',(-5.82442504496082,-3.44945273374648,
101.867570131869));
#33856=CARTESIAN_POINT('Ctrl Pts',(-5.73355843927315,-3.59848057656376,
101.875778115292));
#33857=CARTESIAN_POINT('Ctrl Pts',(-5.63699069137025,-3.74387832940724,
101.883986098715));
#33858=CARTESIAN_POINT('Ctrl Pts',(-5.54049290165615,-3.88917074932472,
101.892188135892));
#33859=CARTESIAN_POINT('Ctrl Pts',(-5.43830239394184,-4.03083801969773,
101.900390173068));
#33860=CARTESIAN_POINT('Ctrl Pts',(-5.33072583250882,-4.1684111000024,101.908592210245));
#33861=CARTESIAN_POINT('Ctrl Pts',(-5.22320560223558,-4.3059121418345,101.916789952524));
#33862=CARTESIAN_POINT('Ctrl Pts',(-5.11030515729286,-4.43932298258219,
101.924987694804));
#33863=CARTESIAN_POINT('Ctrl Pts',(-4.99237364538065,-4.56820472230708,
101.933185437083));
#33864=CARTESIAN_POINT('Ctrl Pts',(-4.87446455619357,-4.69706195730227,
101.941381620697));
#33865=CARTESIAN_POINT('Ctrl Pts',(-4.75152654276489,-4.82139153791958,
101.949577804312));
#33866=CARTESIAN_POINT('Ctrl Pts',(-4.62394829350515,-4.94078851793829,
101.957773987926));
#33867=CARTESIAN_POINT('Ctrl Pts',(-4.49637943578457,-5.0601767086734,101.965969568187));
#33868=CARTESIAN_POINT('Ctrl Pts',(-4.36417128388756,-5.17463277610796,
101.974165148448));
#33869=CARTESIAN_POINT('Ctrl Pts',(-4.22774851464978,-5.28378950156765,
101.982360728709));
#33870=CARTESIAN_POINT('Ctrl Pts',(-4.09131096752224,-5.39295805134425,
101.990557196749));
#33871=CARTESIAN_POINT('Ctrl Pts',(-3.95065817371479,-5.49682589124071,
101.99875366479));
#33872=CARTESIAN_POINT('Ctrl Pts',(-3.80624696209212,-5.59506685067878,
102.006950132831));
#33873=CARTESIAN_POINT('Ctrl Pts',(-3.66179383321541,-5.69333632584778,
102.015148980004));
#33874=CARTESIAN_POINT('Ctrl Pts',(-3.51358041014197,-5.78597546549938,
102.023347827178));
#33875=CARTESIAN_POINT('Ctrl Pts',(-3.36209152494934,-5.87270206786142,
102.031546674351));
#33876=CARTESIAN_POINT('Ctrl Pts',(-3.21044431914049,-5.95951930795647,
102.039754090117));
#33877=CARTESIAN_POINT('Ctrl Pts',(-3.05551512397921,-6.04041148705646,
102.047961505883));
#33878=CARTESIAN_POINT('Ctrl Pts',(-2.89781323524833,-6.11514247206225,
102.056168921649));
#33879=CARTESIAN_POINT('Ctrl Pts',(-2.74002682385167,-6.18991351024763,
102.064380736301));
#33880=CARTESIAN_POINT('Ctrl Pts',(-2.57946508603522,-6.25851663050186,
102.072592550953));
#33881=CARTESIAN_POINT('Ctrl Pts',(-2.41665610906984,-6.32076437232835,
102.080804365605));
#33882=CARTESIAN_POINT('Ctrl Pts',(-2.25360737113515,-6.38310378341778,
102.089028273403));
#33883=CARTESIAN_POINT('Ctrl Pts',(-2.08830512018977,-6.43906899678869,
102.097252181201));
#33884=CARTESIAN_POINT('Ctrl Pts',(-1.92129261856777,-6.4885224569109,102.105476088998));
#33885=CARTESIAN_POINT('Ctrl Pts',(-1.76697615150164,-6.53421654074378,
102.113074827922));
#33886=CARTESIAN_POINT('Ctrl Pts',(-1.61119992339602,-6.5743517779,102.120673566845));
#33887=CARTESIAN_POINT('Ctrl Pts',(-1.45439827161408,-6.60885880220829,
102.128272305769));
#33888=CARTESIAN_POINT('Ctrl Pts',(-1.28620095868867,-6.64587364675711,
102.136423287943));
#33889=CARTESIAN_POINT('Ctrl Pts',(-1.11632544544517,-6.67652144097375,
102.144574270118));
#33890=CARTESIAN_POINT('Ctrl Pts',(-0.94529939735952,-6.70064907672024,
102.152725252292));
#33891=CARTESIAN_POINT('Ctrl Pts',(-0.774472011879651,-6.72474868598162,
102.160866766345));
#33892=CARTESIAN_POINT('Ctrl Pts',(-0.602497110271949,-6.74234316237416,
102.169008280398));
#33893=CARTESIAN_POINT('Ctrl Pts',(-0.429915582250584,-6.75332966707077,
102.177149794451));
#33894=CARTESIAN_POINT('Ctrl Pts',(-0.257498206185753,-6.76430572188747,
102.185283564654));
#33895=CARTESIAN_POINT('Ctrl Pts',(-0.0844757148706075,-6.76868629486567,
102.193417334857));
#33896=CARTESIAN_POINT('Ctrl Pts',(0.0886027882839978,-6.76641992089674,
102.20155110506));
#33897=CARTESIAN_POINT('Ctrl Pts',(0.261553068752986,-6.76415522593793,
102.209678849478));
#33898=CARTESIAN_POINT('Ctrl Pts',(0.434558914306283,-6.75525339383574,
102.217806593896));
#33899=CARTESIAN_POINT('Ctrl Pts',(0.607068105430911,-6.7397149283459,102.225934338314));
#33900=CARTESIAN_POINT('Ctrl Pts',(0.779485764393722,-6.72418470745641,
102.234057770208));
#33901=CARTESIAN_POINT('Ctrl Pts',(0.951406930313782,-6.70202489875823,
102.242181202102));
#33902=CARTESIAN_POINT('Ctrl Pts',(1.12228140005599,-6.67328805455664,102.250304633996));
#33903=CARTESIAN_POINT('Ctrl Pts',(1.29423983022416,-6.64436891511851,102.258479597747));
#33904=CARTESIAN_POINT('Ctrl Pts',(1.46513786356506,-6.60878901859909,102.266654561498));
#33905=CARTESIAN_POINT('Ctrl Pts',(1.63442152863352,-6.56665480033322,102.274829525249));
#33906=CARTESIAN_POINT('Ctrl Pts',(1.80259993569434,-6.52479567761254,102.282951114422));
#33907=CARTESIAN_POINT('Ctrl Pts',(1.96918463951716,-6.47646768023862,102.291072703595));
#33908=CARTESIAN_POINT('Ctrl Pts',(2.13364451927077,-6.42182606938134,102.299194292768));
#33909=CARTESIAN_POINT('Ctrl Pts',(2.29812611110159,-6.36717724471073,102.307316954157));
#33910=CARTESIAN_POINT('Ctrl Pts',(2.46048197276391,-6.30621326172673,102.315439615547));
#33911=CARTESIAN_POINT('Ctrl Pts',(2.62019808385182,-6.23913864258355,102.323562276936));
#33912=CARTESIAN_POINT('Ctrl Pts',(2.77996569541401,-6.17204239522343,102.331687557478));
#33913=CARTESIAN_POINT('Ctrl Pts',(2.93709152416275,-6.09883172971941,102.339812838021));
#33914=CARTESIAN_POINT('Ctrl Pts',(3.09108343974382,-6.01975848091446,102.347938118563));
#33915=CARTESIAN_POINT('Ctrl Pts',(3.24675306529124,-5.93982374547177,102.356151922351));
#33916=CARTESIAN_POINT('Ctrl Pts',(3.39921974923869,-5.85389811051584,102.364365726138));
#33917=CARTESIAN_POINT('Ctrl Pts',(3.54800332959427,-5.76228785927846,102.372579529926));
#33918=CARTESIAN_POINT('Ctrl Pts',(3.69543809982491,-5.67150810851784,102.380718870781));
#33919=CARTESIAN_POINT('Ctrl Pts',(3.83925600355025,-5.57514664295843,102.388858211636));
#33920=CARTESIAN_POINT('Ctrl Pts',(3.9790218042045,-5.47354313782811,102.396997552492));
#33921=CARTESIAN_POINT('Ctrl Pts',(4.12070558044972,-5.37054534996278,102.405248587746));
#33922=CARTESIAN_POINT('Ctrl Pts',(4.25822492660954,-5.2621608514902,102.413499623));
#33923=CARTESIAN_POINT('Ctrl Pts',(4.39116410387866,-5.14878304192433,102.421750658254));
#33924=CARTESIAN_POINT('Ctrl Pts',(4.52410328114777,-5.03540523235846,102.430001693508));
#33925=CARTESIAN_POINT('Ctrl Pts',(4.65246205279082,-4.917034421242,102.438252728762));
#33926=CARTESIAN_POINT('Ctrl Pts',(4.7758664037268,-4.79409940382484,102.446503764016));
#33927=CARTESIAN_POINT('Ctrl Pts',(4.89898264953621,-4.67145139580793,102.454735536047));
#33928=CARTESIAN_POINT('Ctrl Pts',(5.01755205440472,-4.54387770935175,102.462967308077));
#33929=CARTESIAN_POINT('Ctrl Pts',(5.13115663596937,-4.41174801831967,102.471199080108));
#33930=CARTESIAN_POINT('Ctrl Pts',(5.24462556231068,-4.27977610334292,102.479421022581));
#33931=CARTESIAN_POINT('Ctrl Pts',(5.35314123905025,-4.1432592857504,102.487642965053));
#33932=CARTESIAN_POINT('Ctrl Pts',(5.45632110349104,-4.00260527851527,102.495864907526));
#33933=CARTESIAN_POINT('Ctrl Pts',(5.55939843385556,-3.86209104495386,102.504078679515));
#33934=CARTESIAN_POINT('Ctrl Pts',(5.65715030118557,-3.71744809629668,102.512292451505));
#33935=CARTESIAN_POINT('Ctrl Pts',(5.74923310766844,-3.56911861300366,102.520506223495));
#33936=CARTESIAN_POINT('Ctrl Pts',(5.84124285057581,-3.42090682250058,102.528713478226));
#33937=CARTESIAN_POINT('Ctrl Pts',(5.92759230383383,-3.26901462657528,102.536920732956));
#33938=CARTESIAN_POINT('Ctrl Pts',(6.00798001085715,-3.11391476908745,102.545127987686));
#33939=CARTESIAN_POINT('Ctrl Pts',(6.0883200301798,-2.95890692013986,102.553330373698));
#33940=CARTESIAN_POINT('Ctrl Pts',(6.16270518422332,-2.80069551760968,102.56153275971));
#33941=CARTESIAN_POINT('Ctrl Pts',(6.23087893407393,-2.63977967052438,102.569735145722));
#33942=CARTESIAN_POINT('Ctrl Pts',(6.29903233571379,-2.47891185291634,102.577935083521));
#33943=CARTESIAN_POINT('Ctrl Pts',(6.360977882988,-2.31534152668179,102.586135021319));
#33944=CARTESIAN_POINT('Ctrl Pts',(6.41650624705025,-2.14958986357051,102.594334959118));
#33945=CARTESIAN_POINT('Ctrl Pts',(6.472026846814,-1.98386137681988,102.602533750354));
#33946=CARTESIAN_POINT('Ctrl Pts',(6.52113193584389,-1.81595250013607,102.61073254159));
#33947=CARTESIAN_POINT('Ctrl Pts',(6.56366134678883,-1.64640175068854,102.618931332825));
#33948=CARTESIAN_POINT('Ctrl Pts',(6.60619252608039,-1.47684395142562,102.627130464962));
#33949=CARTESIAN_POINT('Ctrl Pts',(6.64214739529731,-1.30564449104982,102.635329597098));
#33950=CARTESIAN_POINT('Ctrl Pts',(6.67141640530415,-1.13335437840009,102.643528729235));
#33951=CARTESIAN_POINT('Ctrl Pts',(6.70069194182912,-0.961025847828328,
102.651729689645));
#33952=CARTESIAN_POINT('Ctrl Pts',(6.72327858980431,-0.787606533896339,
102.659930650056));
#33953=CARTESIAN_POINT('Ctrl Pts',(6.739118383539,-0.613654962211398,102.668131610467));
#33954=CARTESIAN_POINT('Ctrl Pts',(6.75497302297354,-0.43954035602845,102.676340257152));
#33955=CARTESIAN_POINT('Ctrl Pts',(6.7640681418017,-0.264892852834303,102.684548903837));
#33956=CARTESIAN_POINT('Ctrl Pts',(6.76639782620604,-0.090274345825458,
102.692757550522));
#33957=CARTESIAN_POINT('Ctrl Pts',(6.76872862286714,0.0844275289629238,
102.700970116246));
#33958=CARTESIAN_POINT('Ctrl Pts',(6.76428755412174,0.25910002184057,102.709182681969));
#33959=CARTESIAN_POINT('Ctrl Pts',(6.75312080457621,0.433184024174481,102.717395247693));
#33960=CARTESIAN_POINT('Ctrl Pts',(6.74193873263893,0.60750689488003,102.725619082242));
#33961=CARTESIAN_POINT('Ctrl Pts',(6.72401257287093,0.781239304562182,102.73384291679));
#33962=CARTESIAN_POINT('Ctrl Pts',(6.69944024760741,0.953828794248695,102.742066751339));
#33963=CARTESIAN_POINT('Ctrl Pts',(6.67686290296134,1.11240606966546,102.749622908314));
#33964=CARTESIAN_POINT('Ctrl Pts',(6.64867539778419,1.27001837395876,102.757179065288));
#33965=CARTESIAN_POINT('Ctrl Pts',(6.61499105796768,1.42624763032497,102.764735222263));
#33966=CARTESIAN_POINT('Ctrl Pts',(6.57644960021108,1.60500438546353,102.773380940315));
#33967=CARTESIAN_POINT('Ctrl Pts',(6.53062364198936,1.78235784131071,102.782026658367));
#33968=CARTESIAN_POINT('Ctrl Pts',(6.4776287391073,1.9577065454994,102.79067237642));
#33969=CARTESIAN_POINT('Ctrl Pts',(6.42470187088049,2.13283013768694,102.799306995132));
#33970=CARTESIAN_POINT('Ctrl Pts',(6.36462449798613,2.30595381975003,102.807941613845));
#33971=CARTESIAN_POINT('Ctrl Pts',(6.29756288745097,2.4764875688362,102.816576232557));
#33972=CARTESIAN_POINT('Ctrl Pts',(6.22813292134587,2.65304390746782,102.825515792459));
#33973=CARTESIAN_POINT('Ctrl Pts',(6.15121644127757,2.82682372174258,102.834455352362));
#33974=CARTESIAN_POINT('Ctrl Pts',(6.06705486922959,2.99718771747075,102.843394912264));
#33975=CARTESIAN_POINT('Ctrl Pts',(5.98598979180754,3.1612836363987,102.852005565535));
#33976=CARTESIAN_POINT('Ctrl Pts',(5.89820335204383,3.32221027235961,102.860616218805));
#33977=CARTESIAN_POINT('Ctrl Pts',(5.80396090812787,3.47941471758161,102.869226872076));
#33978=CARTESIAN_POINT('Ctrl Pts',(5.70980767099022,3.63647035827869,102.877829374787));
#33979=CARTESIAN_POINT('Ctrl Pts',(5.60921076977305,3.78981057203066,102.886431877498));
#33980=CARTESIAN_POINT('Ctrl Pts',(5.50248177629145,3.93890635856967,102.895034380209));
#33981=CARTESIAN_POINT('Ctrl Pts',(5.39587290414377,4.08783434080192,102.903627200977));
#33982=CARTESIAN_POINT('Ctrl Pts',(5.28314588526197,4.23252717835655,102.912220021744));
#33983=CARTESIAN_POINT('Ctrl Pts',(5.16465606807672,4.37248404210677,102.920812842512));
#33984=CARTESIAN_POINT('Ctrl Pts',(5.15069150491236,4.38897859421726,102.92182554547));
#33985=CARTESIAN_POINT('Ctrl Pts',(5.13664694788962,4.40540739793204,102.922838248428));
#33986=CARTESIAN_POINT('Ctrl Pts',(5.12252301818374,4.42176966023534,102.923850951386));
#33987=CARTESIAN_POINT('Ctrl Pts',(5.00267607501209,4.56060971121688,102.932444123144));
#33988=CARTESIAN_POINT('Ctrl Pts',(4.87725181832151,4.69449267907582,102.941037294903));
#33989=CARTESIAN_POINT('Ctrl Pts',(4.74668977369564,4.82298923825186,102.949630466662));
#33990=CARTESIAN_POINT('Ctrl Pts',(4.61591887935909,4.9516913431459,102.958237384233));
#33991=CARTESIAN_POINT('Ctrl Pts',(4.47999398472752,5.07498959902972,102.966844301804));
#33992=CARTESIAN_POINT('Ctrl Pts',(4.33938998624165,5.19249299925438,102.975451219376));
#33993=CARTESIAN_POINT('Ctrl Pts',(4.19867056023672,5.31009286278104,102.984065202715));
#33994=CARTESIAN_POINT('Ctrl Pts',(4.05326460314171,5.42188818637733,102.992679186054));
#33995=CARTESIAN_POINT('Ctrl Pts',(3.90367773266319,5.52753011384918,103.001293169392));
#33996=CARTESIAN_POINT('Ctrl Pts',(3.75385609914769,5.63333783675246,103.009920671597));
#33997=CARTESIAN_POINT('Ctrl Pts',(3.59984068853573,5.73297268666424,103.018548173802));
#33998=CARTESIAN_POINT('Ctrl Pts',(3.44216516994388,5.82612975677895,103.027175676007));
#33999=CARTESIAN_POINT('Ctrl Pts',(3.32963221999344,5.89261591774023,103.033333120628));
#34000=CARTESIAN_POINT('Ctrl Pts',(3.21523547777787,5.9558034608754,103.03949056525));
#34001=CARTESIAN_POINT('Ctrl Pts',(3.09917575053265,6.01559628526636,103.045648009871));
#34002=CARTESIAN_POINT('Ctrl Pts',(3.09917575053253,6.01559628526642,101.045648756765));
#34003=CARTESIAN_POINT('Ctrl Pts',(2.94379194180815,6.09564848777267,101.053851475175));
#34004=CARTESIAN_POINT('Ctrl Pts',(2.78535787451797,6.16964896183388,101.062054193584));
#34005=CARTESIAN_POINT('Ctrl Pts',(2.62438968426278,6.23737667494397,101.070256911994));
#34006=CARTESIAN_POINT('Ctrl Pts',(2.45542743074839,6.30846790740621,101.078866996914));
#34007=CARTESIAN_POINT('Ctrl Pts',(2.28367335026463,6.37264727895645,101.087477081833));
#34008=CARTESIAN_POINT('Ctrl Pts',(2.10974435081307,6.42971755011154,101.096087166753));
#34009=CARTESIAN_POINT('Ctrl Pts',(1.94376157595981,6.48418047462568,101.104303886168));
#34010=CARTESIAN_POINT('Ctrl Pts',(1.77579854635092,6.53216938358717,101.112520605583));
#34011=CARTESIAN_POINT('Ctrl Pts',(1.60640334848402,6.57356503595875,101.120737324999));
#34012=CARTESIAN_POINT('Ctrl Pts',(1.43688644648369,6.61499042956304,101.12895994782));
#34013=CARTESIAN_POINT('Ctrl Pts',(1.26593567524199,6.64981305445053,101.137182570642));
#34014=CARTESIAN_POINT('Ctrl Pts',(1.09410655370616,6.67796524767367,101.145405193464));
#34015=CARTESIAN_POINT('Ctrl Pts',(0.922046649230749,6.70615525198407,101.153638860054));
#34016=CARTESIAN_POINT('Ctrl Pts',(0.749106392946738,6.72765689459352,101.161872526645));
#34017=CARTESIAN_POINT('Ctrl Pts',(0.575844420042956,6.74245446435535,101.170106193235));
#34018=CARTESIAN_POINT('Ctrl Pts',(0.551492363644704,6.74453427013938,101.171263439166));
#34019=CARTESIAN_POINT('Ctrl Pts',(0.527133948188128,6.74648172474415,101.172420685098));
#34020=CARTESIAN_POINT('Ctrl Pts',(0.502770719782657,6.74829686686421,101.173577931029));
#34021=CARTESIAN_POINT('Ctrl Pts',(0.331108731698954,6.7610862599527,101.181731823195));
#34022=CARTESIAN_POINT('Ctrl Pts',(0.15867722880418,6.76734226510693,101.189885715362));
#34023=CARTESIAN_POINT('Ctrl Pts',(-0.0139804348075886,6.7669855583888,
101.198039607529));
#34024=CARTESIAN_POINT('Ctrl Pts',(-0.186427407832123,6.76662928695253,
101.206183549669));
#34025=CARTESIAN_POINT('Ctrl Pts',(-0.359099630619685,6.75967636665673,
101.214327491809));
#34026=CARTESIAN_POINT('Ctrl Pts',(-0.531447486644818,6.74609906308371,
101.22247143395));
#34027=CARTESIAN_POINT('Ctrl Pts',(-0.703621305920052,6.73253546986277,
101.230607152342));
#34028=CARTESIAN_POINT('Ctrl Pts',(-0.875471048730543,6.71236083894149,
101.238742870735));
#34029=CARTESIAN_POINT('Ctrl Pts',(-1.04644594997033,6.68559944012433,101.246878589128));
#34030=CARTESIAN_POINT('Ctrl Pts',(-1.21728416548072,6.65885943568313,101.255007803428));
#34031=CARTESIAN_POINT('Ctrl Pts',(-1.38724857241814,6.62554320435573,101.263137017728));
#34032=CARTESIAN_POINT('Ctrl Pts',(-1.5557923882042,6.58572691848105,101.271266232029));
#34033=CARTESIAN_POINT('Ctrl Pts',(-1.72423690021901,6.54593409183165,101.279390656704));
#34034=CARTESIAN_POINT('Ctrl Pts',(-1.89126213295922,6.49964892127365,101.28751508138));
#34035=CARTESIAN_POINT('Ctrl Pts',(-2.05633038219051,6.44699886453226,101.295639506055));
#34036=CARTESIAN_POINT('Ctrl Pts',(-2.22240070136559,6.39402918824172,101.303813251189));
#34037=CARTESIAN_POINT('Ctrl Pts',(-2.38648982816899,6.3346171530717,101.311986996323));
#34038=CARTESIAN_POINT('Ctrl Pts',(-2.54806399910648,6.26894399851024,101.320160741457));
#34039=CARTESIAN_POINT('Ctrl Pts',(-2.70860349633345,6.20369139561318,101.32828214432));
#34040=CARTESIAN_POINT('Ctrl Pts',(-2.86665981931489,6.13225778843294,101.336403547182));
#34041=CARTESIAN_POINT('Ctrl Pts',(-3.02172817996081,6.05486975965881,101.344524950044));
#34042=CARTESIAN_POINT('Ctrl Pts',(-3.17680852967557,5.97747574764993,101.35264698081));
#34043=CARTESIAN_POINT('Ctrl Pts',(-3.32890012940004,5.89412656043081,101.360769011576));
#34044=CARTESIAN_POINT('Ctrl Pts',(-3.47752182676671,5.80509525713068,101.368891042343));
#34045=CARTESIAN_POINT('Ctrl Pts',(-3.62618331578456,5.71604011678235,101.377015247684));
#34046=CARTESIAN_POINT('Ctrl Pts',(-3.77137273875985,5.62130001913802,101.385139453025));
#34047=CARTESIAN_POINT('Ctrl Pts',(-3.91263706047693,5.52119192140451,101.393263658366));
#34048=CARTESIAN_POINT('Ctrl Pts',(-4.05543047072851,5.42000022278301,101.401475802608));
#34049=CARTESIAN_POINT('Ctrl Pts',(-4.19421299676689,5.31332385652425,101.409687946851));
#34050=CARTESIAN_POINT('Ctrl Pts',(-4.32855089063314,5.20153209998737,101.417900091093));
#34051=CARTESIAN_POINT('Ctrl Pts',(-4.46166242758833,5.09076087897687,101.42603726751));
#34052=CARTESIAN_POINT('Ctrl Pts',(-4.59040991419057,4.97496756616058,101.434174443926));
#34053=CARTESIAN_POINT('Ctrl Pts',(-4.71440865088442,4.85454839016629,101.442311620343));
#34054=CARTESIAN_POINT('Ctrl Pts',(-4.84012098856856,4.73246508093375,101.450561248498));
#34055=CARTESIAN_POINT('Ctrl Pts',(-4.96095209377052,4.60562740212507,101.458810876654));
#34056=CARTESIAN_POINT('Ctrl Pts',(-5.07654374176494,4.47448238771226,101.467060504809));
#34057=CARTESIAN_POINT('Ctrl Pts',(-5.19213538975946,4.34333737329935,101.475310132964));
#34058=CARTESIAN_POINT('Ctrl Pts',(-5.30248738655973,4.20788536154887,101.48355976112));
#34059=CARTESIAN_POINT('Ctrl Pts',(-5.40728763516789,4.06860288435238,101.491809389275));
#34060=CARTESIAN_POINT('Ctrl Pts',(-5.51599389035984,3.92412921457607,101.500366489047));
#34061=CARTESIAN_POINT('Ctrl Pts',(-5.61906258002938,3.77508792084405,101.50892358882));
#34062=CARTESIAN_POINT('Ctrl Pts',(-5.71609298988985,3.62195664398846,101.517480688592));
#34063=CARTESIAN_POINT('Ctrl Pts',(-5.80982120828065,3.47403681369791,101.525746568509));
#34064=CARTESIAN_POINT('Ctrl Pts',(-5.89791512808572,3.32230111885043,101.534012448427));
#34065=CARTESIAN_POINT('Ctrl Pts',(-5.9800536091311,3.16721452256051,101.542278328344));
#34066=CARTESIAN_POINT('Ctrl Pts',(-6.06211347227962,3.01227636561197,101.550536296671));
#34067=CARTESIAN_POINT('Ctrl Pts',(-6.13822908460589,2.85399400400668,101.558794264997));
#34068=CARTESIAN_POINT('Ctrl Pts',(-6.2081229015865,2.6928607536962,101.567052233323));
#34069=CARTESIAN_POINT('Ctrl Pts',(-6.27796196947152,2.53185372198564,101.575303733033));
#34070=CARTESIAN_POINT('Ctrl Pts',(-6.34158880976767,2.36800057174501,101.583555232742));
#34071=CARTESIAN_POINT('Ctrl Pts',(-6.39877202886701,2.20181868522118,101.591806732452));
#34072=CARTESIAN_POINT('Ctrl Pts',(-6.45592039237351,2.03573809359239,101.600053202523));
#34073=CARTESIAN_POINT('Ctrl Pts',(-6.50663284512085,1.86733192623631,101.608299672594));
#34074=CARTESIAN_POINT('Ctrl Pts',(-6.55072626635181,1.69713711388575,101.616546142666));
#34075=CARTESIAN_POINT('Ctrl Pts',(-6.59480081166407,1.52701516010118,101.624789082512));
#34076=CARTESIAN_POINT('Ctrl Pts',(-6.63226188359202,1.35510642812366,101.633032022358));
#34077=CARTESIAN_POINT('Ctrl Pts',(-6.66297629917446,1.18196270526588,101.641274962204));
#34078=CARTESIAN_POINT('Ctrl Pts',(-6.6936832034107,1.00886132547147,101.649515886203));
#34079=CARTESIAN_POINT('Ctrl Pts',(-6.71764667896215,0.834525903982359,
101.657756810202));
#34080=CARTESIAN_POINT('Ctrl Pts',(-6.73478467878672,0.659518256289958,
101.665997734201));
#34081=CARTESIAN_POINT('Ctrl Pts',(-6.75192301453384,0.484507178266194,
101.67423881973));
#34082=CARTESIAN_POINT('Ctrl Pts',(-6.76223557122643,0.308824198567568,
101.68247990526));
#34083=CARTESIAN_POINT('Ctrl Pts',(-6.76569215398912,0.133036376416896,
101.690720990789));
#34084=CARTESIAN_POINT('Ctrl Pts',(-6.7665951641789,0.0871129296084177,
101.692873921796));
#34085=CARTESIAN_POINT('Ctrl Pts',(-6.76703054237299,0.0411823393665977,
101.695026852803));
#34086=CARTESIAN_POINT('Ctrl Pts',(-6.76699833621951,-0.00474527158081274,
101.69717978381));
#34087=CARTESIAN_POINT('',(-6.76699858504056,-0.0030292735211277,101.30282021619));
#34088=CARTESIAN_POINT('Ctrl Pts',(3.0991757505325,6.01559628526644,100.651392015122));
#34089=CARTESIAN_POINT('Ctrl Pts',(2.93382384459261,6.10078395293761,100.660141463035));
#34090=CARTESIAN_POINT('Ctrl Pts',(2.76495772122985,6.17915010267049,100.668890910947));
#34091=CARTESIAN_POINT('Ctrl Pts',(2.59315093316717,6.25042856433175,100.67764035886));
#34092=CARTESIAN_POINT('Ctrl Pts',(2.42134553245627,6.32170645041447,100.68638973612));
#34093=CARTESIAN_POINT('Ctrl Pts',(2.24659977927605,6.38589665313452,100.69513911338));
#34094=CARTESIAN_POINT('Ctrl Pts',(2.06950718689938,6.44278115439069,100.70388849064));
#34095=CARTESIAN_POINT('Ctrl Pts',(1.89241596572884,6.49966521519717,100.712637800154));
#34096=CARTESIAN_POINT('Ctrl Pts',(1.71297821457225,6.54924360009539,100.721387109669));
#34097=CARTESIAN_POINT('Ctrl Pts',(1.53180337335876,6.59134792173549,100.730136419183));
#34098=CARTESIAN_POINT('Ctrl Pts',(1.35062987477813,6.63345193135298,100.73888566386));
#34099=CARTESIAN_POINT('Ctrl Pts',(1.16771959102981,6.66808192368233,100.747634908536));
#34100=CARTESIAN_POINT('Ctrl Pts',(0.983693746907121,6.69512028363164,100.756384153212));
#34101=CARTESIAN_POINT('Ctrl Pts',(0.799669205420127,6.72215845218864,100.765133335956));
#34102=CARTESIAN_POINT('Ctrl Pts',(0.61452940287371,6.74160505424577,100.7738825187));
#34103=CARTESIAN_POINT('Ctrl Pts',(0.428903127363461,6.75339404354121,100.782631701444));
#34104=CARTESIAN_POINT('Ctrl Pts',(0.243278104164221,6.76518295330329,100.791380825163));
#34105=CARTESIAN_POINT('Ctrl Pts',(0.0571669005395895,6.76931433552275,
100.800129948882));
#34106=CARTESIAN_POINT('Ctrl Pts',(-0.128798404776912,6.76577415902474,
100.8088790726));
#34107=CARTESIAN_POINT('Ctrl Pts',(-0.31476251725861,6.76223400523444,100.817628140199));
#34108=CARTESIAN_POINT('Ctrl Pts',(-0.500580446819135,6.75102239665092,
100.826377207799));
#34109=CARTESIAN_POINT('Ctrl Pts',(-0.685621118842349,6.732177410125,100.835126275398));
#34110=CARTESIAN_POINT('Ctrl Pts',(-0.870660665414201,6.71333253821775,
100.843875289784));
#34111=CARTESIAN_POINT('Ctrl Pts',(-1.05492267885455,6.68685441030617,100.852624304169));
#34112=CARTESIAN_POINT('Ctrl Pts',(-1.23778137635218,6.65283295028183,100.861373318555));
#34113=CARTESIAN_POINT('Ctrl Pts',(-1.42999922978813,6.61707018861873,100.870570128923));
#34114=CARTESIAN_POINT('Ctrl Pts',(-1.62066601233661,6.57297172934421,100.87976693929));
#34115=CARTESIAN_POINT('Ctrl Pts',(-1.80906628500351,6.52070304311304,100.888963749657));
#34116=CARTESIAN_POINT('Ctrl Pts',(-1.98831342545495,6.47097374915041,100.897713747395));
#34117=CARTESIAN_POINT('Ctrl Pts',(-2.16550875896672,6.41384933989539,100.906463745133));
#34118=CARTESIAN_POINT('Ctrl Pts',(-2.34005036713983,6.34952386240486,100.915213742871));
#34119=CARTESIAN_POINT('Ctrl Pts',(-2.51458843547062,6.28519968948607,100.923963563152));
#34120=CARTESIAN_POINT('Ctrl Pts',(-2.68647261718029,6.2136748397111,100.932713383432));
#34121=CARTESIAN_POINT('Ctrl Pts',(-2.85511905908706,6.13519226743855,100.941463203713));
#34122=CARTESIAN_POINT('Ctrl Pts',(-3.02376230488855,6.05671118252952,100.950212858172));
#34123=CARTESIAN_POINT('Ctrl Pts',(-3.18916767379871,5.97127275992651,100.95896251263));
#34124=CARTESIAN_POINT('Ctrl Pts',(-3.3507733410275,5.87916720438018,100.967712167089));
#34125=CARTESIAN_POINT('Ctrl Pts',(-3.51237616037329,5.78706327195666,100.976461667357));
#34126=CARTESIAN_POINT('Ctrl Pts',(-3.6701791630226,5.68829258362324,100.985211167626));
#34127=CARTESIAN_POINT('Ctrl Pts',(-3.82364636566422,5.58319061741069,100.993960667894));
#34128=CARTESIAN_POINT('Ctrl Pts',(-3.97711106778766,5.47809036367725,101.002710025603));
#34129=CARTESIAN_POINT('Ctrl Pts',(-4.12623987481902,5.36665920043244,101.011459383311));
#34130=CARTESIAN_POINT('Ctrl Pts',(-4.27052628213912,5.24927559512349,101.02020874102));
#34131=CARTESIAN_POINT('Ctrl Pts',(-4.41481053024959,5.13189374643053,101.028957967796));
#34132=CARTESIAN_POINT('Ctrl Pts',(-4.55425230136508,5.00855981477373,101.037707194573));
#34133=CARTESIAN_POINT('Ctrl Pts',(-4.68837800630524,4.87969268192099,101.046456421349));
#34134=CARTESIAN_POINT('Ctrl Pts',(-4.8225018822886,4.75082730631844,101.05520552882));
#34135=CARTESIAN_POINT('Ctrl Pts',(-4.95130963052922,4.61642907903572,101.063954636291));
#34136=CARTESIAN_POINT('Ctrl Pts',(-5.07436379033314,4.47695444731749,101.072703743762));
#34137=CARTESIAN_POINT('Ctrl Pts',(-5.19741643562771,4.33748153220628,101.081452743551));
#34138=CARTESIAN_POINT('Ctrl Pts',(-5.31471544462755,4.19293255254613,101.090201743341));
#34139=CARTESIAN_POINT('Ctrl Pts',(-5.42586245275625,4.04379841779607,101.098950743131));
#34140=CARTESIAN_POINT('Ctrl Pts',(-5.53702160019144,3.89464799484354,101.107700698473));
#34141=CARTESIAN_POINT('Ctrl Pts',(-5.64202723081238,3.7409116444387,101.116450653815));
#34142=CARTESIAN_POINT('Ctrl Pts',(-5.74052265232949,3.58311159163261,101.125200609157));
#34143=CARTESIAN_POINT('Ctrl Pts',(-5.83901427066895,3.42531763191822,101.13395022664));
#34144=CARTESIAN_POINT('Ctrl Pts',(-5.93099603115711,3.26346052695663,101.142699844122));
#34145=CARTESIAN_POINT('Ctrl Pts',(-6.01615550622722,3.09809004467139,101.151449461605));
#34146=CARTESIAN_POINT('Ctrl Pts',(-6.10131214578771,2.93272506863886,101.160198787756));
#34147=CARTESIAN_POINT('Ctrl Pts',(-6.17964682328723,2.76384720416949,101.168948113907));
#34148=CARTESIAN_POINT('Ctrl Pts',(-6.25089348288543,2.59203002791644,101.177697440058));
#34149=CARTESIAN_POINT('Ctrl Pts',(-6.32213814889316,2.42021765937067,101.18644652139));
#34150=CARTESIAN_POINT('Ctrl Pts',(-6.38629508412577,2.24546640831943,101.195195602721));
#34151=CARTESIAN_POINT('Ctrl Pts',(-6.44314639819808,2.06836976660053,101.203944684053));
#34152=CARTESIAN_POINT('Ctrl Pts',(-6.500002852837,1.89125711158277,101.212694556487));
#34153=CARTESIAN_POINT('Ctrl Pts',(-6.54955227673252,1.71179891440246,101.221444428922));
#34154=CARTESIAN_POINT('Ctrl Pts',(-6.59162635926389,1.53060476278412,101.230194301356));
#34155=CARTESIAN_POINT('Ctrl Pts',(-6.63369752055195,1.34942319164699,101.238943566278));
#34156=CARTESIAN_POINT('Ctrl Pts',(-6.66829431424249,1.16650618642729,101.247692831201));
#34157=CARTESIAN_POINT('Ctrl Pts',(-6.6952992374541,0.98247499761903,101.256442096123));
#34158=CARTESIAN_POINT('Ctrl Pts',(-6.72230554731438,0.798434359178225,
101.265191810303));
#34159=CARTESIAN_POINT('Ctrl Pts',(-6.74171916496698,0.613279706240836,
101.273941524483));
#34160=CARTESIAN_POINT('Ctrl Pts',(-6.75347414817272,0.427639953655887,
101.282691238662));
#34161=CARTESIAN_POINT('Ctrl Pts',(-6.76248837758735,0.285283364200229,
101.289400897838));
#34162=CARTESIAN_POINT('Ctrl Pts',(-6.76699999999988,0.142641701107921,
101.296110557014));
#34163=CARTESIAN_POINT('Ctrl Pts',(-6.767,5.52010523486073E-12,101.30282021619));
#34164=CARTESIAN_POINT('Ctrl Pts',(-6.76699704717928,-0.00632166646298646,
101.30282021619));
#34165=CARTESIAN_POINT('Ctrl Pts',(-6.76677605484367,-0.24288183478154,
101.313959647533));
#34166=CARTESIAN_POINT('Ctrl Pts',(-6.75414753504645,-0.478876740857043,
101.325099078876));
#34167=CARTESIAN_POINT('Ctrl Pts',(-6.72930744162487,-0.713239339977983,
101.336238510219));
#34168=CARTESIAN_POINT('Ctrl Pts',(-6.70352641088801,-0.956479543183305,
101.347799900788));
#34169=CARTESIAN_POINT('Ctrl Pts',(-6.66459101458145,-1.19796201672306,
101.359361291358));
#34170=CARTESIAN_POINT('Ctrl Pts',(-6.61276709992077,-1.43652367965356,
101.370922681928));
#34171=CARTESIAN_POINT('Ctrl Pts',(-6.60039721361044,-1.49346612924997,
101.373682278301));
#34172=CARTESIAN_POINT('Ctrl Pts',(-6.58729323537896,-1.55024227680139,
101.376441874675));
#34173=CARTESIAN_POINT('Ctrl Pts',(-6.57345917388123,-1.60683648493453,
101.379201471048));
#34174=CARTESIAN_POINT('Ctrl Pts',(-6.53257525540682,-1.77408982494738,
101.387356929454));
#34175=CARTESIAN_POINT('Ctrl Pts',(-6.48523716147742,-1.94005459146327,
101.395512387861));
#34176=CARTESIAN_POINT('Ctrl Pts',(-6.43153762266074,-2.10418934706445,
101.403667846268));
#34177=CARTESIAN_POINT('Ctrl Pts',(-6.37790344324148,-2.26812432909289,
101.41181337841));
#34178=CARTESIAN_POINT('Ctrl Pts',(-6.31792334356615,-2.43023339030949,
101.419958910552));
#34179=CARTESIAN_POINT('Ctrl Pts',(-6.2517410497252,-2.58998510559055,101.428104442694));
#34180=CARTESIAN_POINT('Ctrl Pts',(-6.18562539162669,-2.74957597461595,
101.436241773494));
#34181=CARTESIAN_POINT('Ctrl Pts',(-6.11332011027605,-2.90681388777158,
101.444379104295));
#34182=CARTESIAN_POINT('Ctrl Pts',(-6.0350187392794,-3.0611824213115,101.452516435095));
#34183=CARTESIAN_POINT('Ctrl Pts',(-5.95677975086082,-3.21542796968561,
101.460647282897));
#34184=CARTESIAN_POINT('Ctrl Pts',(-5.87255434911937,-3.36680836576513,
101.468778130699));
#34185=CARTESIAN_POINT('Ctrl Pts',(-5.78258419121467,-3.51482703294404,
101.476908978501));
#34186=CARTESIAN_POINT('Ctrl Pts',(-5.69266681260293,-3.66275886776898,
101.485035056495));
#34187=CARTESIAN_POINT('Ctrl Pts',(-5.59701157858968,-3.80733258953256,
101.493161134489));
#34188=CARTESIAN_POINT('Ctrl Pts',(-5.49590610710017,-3.94807612159885,
101.501287212483));
#34189=CARTESIAN_POINT('Ctrl Pts',(-5.39444213407503,-4.08931870452396,
101.509442104065));
#34190=CARTESIAN_POINT('Ctrl Pts',(-5.28748937522943,-4.22670355676432,
101.517596995647));
#34191=CARTESIAN_POINT('Ctrl Pts',(-5.17538278403037,-4.35978233846165,
101.525751887229));
#34192=CARTESIAN_POINT('Ctrl Pts',(-5.06371336934004,-4.49234215944,101.533874977585));
#34193=CARTESIAN_POINT('Ctrl Pts',(-4.94693049683313,-4.62062916326516,
101.541998067942));
#34194=CARTESIAN_POINT('Ctrl Pts',(-4.82540576829853,-4.74423314891578,
101.550121158298));
#34195=CARTESIAN_POINT('Ctrl Pts',(-4.70387149708733,-4.86784684051576,
101.558244886516));
#34196=CARTESIAN_POINT('Ctrl Pts',(-4.57759488461345,-4.98677652056343,
101.566368614735));
#34197=CARTESIAN_POINT('Ctrl Pts',(-4.44698442969164,-5.10064882951964,
101.574492342953));
#34198=CARTESIAN_POINT('Ctrl Pts',(-4.31633887015681,-5.21455174432087,
101.582618254614));
#34199=CARTESIAN_POINT('Ctrl Pts',(-4.18135742442363,-5.32339434113196,
101.590744166274));
#34200=CARTESIAN_POINT('Ctrl Pts',(-4.0424816528769,-5.42684356566077,101.598870077934));
#34201=CARTESIAN_POINT('Ctrl Pts',(-3.90271775633498,-5.530954358734,101.607047955644));
#34202=CARTESIAN_POINT('Ctrl Pts',(-3.75900985307031,-5.62960233335927,
101.615225833354));
#34203=CARTESIAN_POINT('Ctrl Pts',(-3.6118368983089,-5.72249274530028,101.623403711064));
#34204=CARTESIAN_POINT('Ctrl Pts',(-3.46536636814058,-5.81493981145188,
101.631542557538));
#34205=CARTESIAN_POINT('Ctrl Pts',(-3.31546413734347,-5.90168402369238,
101.639681404011));
#34206=CARTESIAN_POINT('Ctrl Pts',(-3.16262594594144,-5.98248160265103,
101.647820250485));
#34207=CARTESIAN_POINT('Ctrl Pts',(-3.00868831182946,-6.06386039961777,
101.656017643813));
#34208=CARTESIAN_POINT('Ctrl Pts',(-2.85177265868612,-6.13920652292378,
101.664215037142));
#34209=CARTESIAN_POINT('Ctrl Pts',(-2.69240440419186,-6.20832082968401,
101.67241243047));
#34210=CARTESIAN_POINT('Ctrl Pts',(-2.5330361496976,-6.27743513644424,101.680609823798));
#34211=CARTESIAN_POINT('Ctrl Pts',(-2.37121566294458,-6.34031754879485,
101.688807217127));
#34212=CARTESIAN_POINT('Ctrl Pts',(-2.20748187330029,-6.39682052109098,
101.697004610455));
#34213=CARTESIAN_POINT('Ctrl Pts',(-2.04317251602129,-6.45352211629927,
101.705230819792));
#34214=CARTESIAN_POINT('Ctrl Pts',(-1.87644740536304,-6.50396820714166,
101.713457029129));
#34215=CARTESIAN_POINT('Ctrl Pts',(-1.70782342178583,-6.54794839319918,
101.721683238466));
#34216=CARTESIAN_POINT('Ctrl Pts',(-1.5393888800303,-6.59187916940179,101.729900206009));
#34217=CARTESIAN_POINT('Ctrl Pts',(-1.36906005721576,-6.62935841606095,
101.738117173552));
#34218=CARTESIAN_POINT('Ctrl Pts',(-1.19737214157202,-6.66022439220986,
101.746334141096));
#34219=CARTESIAN_POINT('Ctrl Pts',(-1.02584265080669,-6.69106188680549,
101.754543526439));
#34220=CARTESIAN_POINT('Ctrl Pts',(-0.852956915561639,-6.71529820096794,
101.762752911782));
#34221=CARTESIAN_POINT('Ctrl Pts',(-0.679263651728511,-6.73282183719727,
101.770962297126));
#34222=CARTESIAN_POINT('Ctrl Pts',(-0.505695812766533,-6.75033281951149,
101.779165754426));
#34223=CARTESIAN_POINT('Ctrl Pts',(-0.331321962072286,-6.76114074295263,
101.787369211727));
#34224=CARTESIAN_POINT('Ctrl Pts',(-0.156699429616982,-6.7651854585634,
101.795572669028));
#34225=CARTESIAN_POINT('Ctrl Pts',(0.017832035788296,-6.76922806482257,
101.803771848159));
#34226=CARTESIAN_POINT('Ctrl Pts',(0.192611566902767,-6.76651448151195,
101.811971027291));
#34227=CARTESIAN_POINT('Ctrl Pts',(0.367078218529337,-6.75703652361605,
101.820170206423));
#34228=CARTESIAN_POINT('Ctrl Pts',(0.541511996878627,-6.7475603515717,101.828367840653));
#34229=CARTESIAN_POINT('Ctrl Pts',(0.71563265509255,-6.73132235694608,101.836565474883));
#34230=CARTESIAN_POINT('Ctrl Pts',(0.888880445623995,-6.70836645938393,
101.844763109113));
#34231=CARTESIAN_POINT('Ctrl Pts',(1.06211573094008,-6.68541221880362,101.852960151628));
#34232=CARTESIAN_POINT('Ctrl Pts',(1.234477918364,-6.65574108724116,101.861157194144));
#34233=CARTESIAN_POINT('Ctrl Pts',(1.40541362672095,-6.6194487336807,101.869354236659));
#34234=CARTESIAN_POINT('Ctrl Pts',(1.57636806403,-6.58315240366759,101.877552177302));
#34235=CARTESIAN_POINT('Ctrl Pts',(1.74589535995426,-6.54023348082067,101.885750117945));
#34236=CARTESIAN_POINT('Ctrl Pts',(1.91345349777141,-6.4908385214752,101.893948058588));
#34237=CARTESIAN_POINT('Ctrl Pts',(2.08106044799347,-6.44142917257642,101.902148387424));
#34238=CARTESIAN_POINT('Ctrl Pts',(2.24669675351575,-6.38554013074687,101.91034871626));
#34239=CARTESIAN_POINT('Ctrl Pts',(2.40983664903004,-6.32336748299446,101.918549045096));
#34240=CARTESIAN_POINT('Ctrl Pts',(2.57314654054857,-6.26113004972985,101.926757918887));
#34241=CARTESIAN_POINT('Ctrl Pts',(2.73395448939905,-6.19259605716673,101.934966792679));
#34242=CARTESIAN_POINT('Ctrl Pts',(2.89175485330826,-6.11800971463499,101.94317566647));
#34243=CARTESIAN_POINT('Ctrl Pts',(3.04963990693204,-6.043383342436,101.951388945874));
#34244=CARTESIAN_POINT('Ctrl Pts',(3.20451383998295,-5.96269831037021,101.959602225277));
#34245=CARTESIAN_POINT('Ctrl Pts',(3.35589673515166,-5.87624421744012,101.96781550468));
#34246=CARTESIAN_POINT('Ctrl Pts',(3.5075010515976,-5.78966367181101,101.976040797296));
#34247=CARTESIAN_POINT('Ctrl Pts',(3.65560382144678,-5.69729739200272,101.984266089911));
#34248=CARTESIAN_POINT('Ctrl Pts',(3.7997541101936,-5.5994783419589,101.992491382527));
#34249=CARTESIAN_POINT('Ctrl Pts',(3.93012073039307,-5.51101276165242,101.999930171639));
#34250=CARTESIAN_POINT('Ctrl Pts',(4.05725485954066,-5.41808800326091,102.007368960751));
#34251=CARTESIAN_POINT('Ctrl Pts',(4.18084761357551,-5.32097756357419,102.014807749863));
#34252=CARTESIAN_POINT('Ctrl Pts',(4.31752292777657,-5.2135877739378,102.023033950882));
#34253=CARTESIAN_POINT('Ctrl Pts',(4.45024897394864,-5.10077851177387,102.031260151901));
#34254=CARTESIAN_POINT('Ctrl Pts',(4.5785688837601,-4.98287025484949,102.039486352919));
#34255=CARTESIAN_POINT('Ctrl Pts',(4.70674465319765,-4.86509444300137,102.047703313535));
#34256=CARTESIAN_POINT('Ctrl Pts',(4.83052388012345,-4.74223128214391,102.055920274151));
#34257=CARTESIAN_POINT('Ctrl Pts',(4.94948067859382,-4.61464299943414,102.064137234767));
#34258=CARTESIAN_POINT('Ctrl Pts',(5.06832772974694,-4.48717242728752,102.072346614568));
#34259=CARTESIAN_POINT('Ctrl Pts',(5.18236096992875,-4.35498567567921,102.08055599437));
#34260=CARTESIAN_POINT('Ctrl Pts',(5.29118941659963,-4.21848356138365,102.088765374171));
#34261=CARTESIAN_POINT('Ctrl Pts',(5.39993929590646,-4.08207999311752,102.096968827312));
#34262=CARTESIAN_POINT('Ctrl Pts',(5.50349164340634,-3.94136754683849,102.105172280452));
#34263=CARTESIAN_POINT('Ctrl Pts',(5.60149397071873,-3.79678209751385,102.113375733593));
#34264=CARTESIAN_POINT('Ctrl Pts',(5.6994452054739,-3.65227202640264,102.121574909943));
#34265=CARTESIAN_POINT('Ctrl Pts',(5.79185198356465,-3.50389327091828,102.129774086293));
#34266=CARTESIAN_POINT('Ctrl Pts',(5.87840353612408,-3.35211289584404,102.137973262643));
#34267=CARTESIAN_POINT('Ctrl Pts',(5.9649388027028,-3.2003610805378,102.146170896194));
#34268=CARTESIAN_POINT('Ctrl Pts',(6.04562085544122,-3.045209228725,102.154368529746));
#34269=CARTESIAN_POINT('Ctrl Pts',(6.1201833705286,-2.88715162592914,102.162566163297));
#34270=CARTESIAN_POINT('Ctrl Pts',(6.19474051528497,-2.72910540715973,102.170763206418));
#34271=CARTESIAN_POINT('Ctrl Pts',(6.26317884635147,-2.56815417822818,102.178960249538));
#34272=CARTESIAN_POINT('Ctrl Pts',(6.32527898651211,-2.40481490821818,102.187157292659));
#34273=CARTESIAN_POINT('Ctrl Pts',(6.38738594053535,-2.24145771600476,102.19535523519));
#34274=CARTESIAN_POINT('Ctrl Pts',(6.44315319062226,-2.07571229602015,102.203553177721));
#34275=CARTESIAN_POINT('Ctrl Pts',(6.49241028927303,-1.90811363281691,102.211751120252));
#34276=CARTESIAN_POINT('Ctrl Pts',(6.54168174502811,-1.74046611916255,102.219951452261));
#34277=CARTESIAN_POINT('Ctrl Pts',(6.58443916857949,-1.57096463037527,102.228151784269));
#34278=CARTESIAN_POINT('Ctrl Pts',(6.62056254925754,-1.40015732379206,102.236352116278));
#34279=CARTESIAN_POINT('Ctrl Pts',(6.65672358026163,-1.22917198982982,102.244560995248));
#34280=CARTESIAN_POINT('Ctrl Pts',(6.68623668002341,-1.05687847035063,102.252769874219));
#34281=CARTESIAN_POINT('Ctrl Pts',(6.70903318831306,-0.883834078384577,
102.26097875319));
#34282=CARTESIAN_POINT('Ctrl Pts',(6.73184193429711,-0.710696792175269,
102.269192038877));
#34283=CARTESIAN_POINT('Ctrl Pts',(6.74792686787206,-0.536808186722328,
102.277405324565));
#34284=CARTESIAN_POINT('Ctrl Pts',(6.75727141716096,-0.362728541501153,
102.285618610252));
#34285=CARTESIAN_POINT('Ctrl Pts',(6.76662963637377,-0.188394239213868,
102.293843910964));
#34286=CARTESIAN_POINT('Ctrl Pts',(6.76922776069267,-0.0138686972772417,
102.302069211676));
#34287=CARTESIAN_POINT('Ctrl Pts',(6.76510136961379,0.160288673491626,102.310294512388));
#34288=CARTESIAN_POINT('Ctrl Pts',(6.76136954664049,0.317793007128361,102.317733304682));
#34289=CARTESIAN_POINT('Ctrl Pts',(6.75213842063547,0.474996070190415,102.325172096976));
#34290=CARTESIAN_POINT('Ctrl Pts',(6.7374705412114,0.631490068258035,102.33261088927));
#34291=CARTESIAN_POINT('Ctrl Pts',(6.72139525549191,0.802999913654975,102.340763445483));
#34292=CARTESIAN_POINT('Ctrl Pts',(6.69874158818251,0.97416380000485,102.348916001697));
#34293=CARTESIAN_POINT('Ctrl Pts',(6.66952499726471,1.14443230942732,102.35706855791));
#34294=CARTESIAN_POINT('Ctrl Pts',(6.64034225447185,1.31450355867679,102.36521166919));
#34295=CARTESIAN_POINT('Ctrl Pts',(6.60461178436809,1.48368113926133,102.373354780471));
#34296=CARTESIAN_POINT('Ctrl Pts',(6.56240095140022,1.65141840641962,102.381497891751));
#34297=CARTESIAN_POINT('Ctrl Pts',(6.52023014639807,1.81899661058134,102.389633281028));
#34298=CARTESIAN_POINT('Ctrl Pts',(6.47159130151889,1.98513686843841,102.397768670306));
#34299=CARTESIAN_POINT('Ctrl Pts',(6.41660320791154,2.14930041460457,102.405904059583));
#34300=CARTESIAN_POINT('Ctrl Pts',(6.36165570444918,2.31334278140798,102.414033443622));
#34301=CARTESIAN_POINT('Ctrl Pts',(6.30036840007265,2.47541099674163,102.42216282766));
#34302=CARTESIAN_POINT('Ctrl Pts',(6.23291052180081,2.63497920812001,102.430292211699));
#34303=CARTESIAN_POINT('Ctrl Pts',(6.16548826901972,2.79446314919543,102.438417302491));
#34304=CARTESIAN_POINT('Ctrl Pts',(6.0919020743481,2.95144937976762,102.446542393283));
#34305=CARTESIAN_POINT('Ctrl Pts',(6.01237010880785,3.10542986955332,102.454667484075));
#34306=CARTESIAN_POINT('Ctrl Pts',(5.93253455251368,3.25999813624939,102.4628235901));
#34307=CARTESIAN_POINT('Ctrl Pts',(5.84670786880475,3.41153731929982,102.470979696125));
#34308=CARTESIAN_POINT('Ctrl Pts',(5.7551585947507,3.55955594832659,102.479135802151));
#34309=CARTESIAN_POINT('Ctrl Pts',(5.66397778996784,3.70697882914099,102.487259081324));
#34310=CARTESIAN_POINT('Ctrl Pts',(5.56712058616963,3.85090914058018,102.495382360497));
#34311=CARTESIAN_POINT('Ctrl Pts',(5.46489701561949,3.9908883232525,102.503505639671));
#34312=CARTESIAN_POINT('Ctrl Pts',(5.3626598331371,4.13088614533589,102.511630000528));
#34313=CARTESIAN_POINT('Ctrl Pts',(5.25505507636806,4.26693149524327,102.519754361384));
#34314=CARTESIAN_POINT('Ctrl Pts',(5.14243446978351,4.39859713135704,102.527878722241));
#34315=CARTESIAN_POINT('Ctrl Pts',(5.02977744016367,4.53030534992758,102.536005710626));
#34316=CARTESIAN_POINT('Ctrl Pts',(4.9121015680922,4.65763075622964,102.544132699012));
#34317=CARTESIAN_POINT('Ctrl Pts',(4.78979695461393,4.7801813912833,102.552259687397));
#34318=CARTESIAN_POINT('Ctrl Pts',(4.66670165573424,4.90352430223986,102.560439215837));
#34319=CARTESIAN_POINT('Ctrl Pts',(4.53891782486309,5.02203022519002,102.568618744277));
#34320=CARTESIAN_POINT('Ctrl Pts',(4.40687795864314,5.13533987751787,102.576798272717));
#34321=CARTESIAN_POINT('Ctrl Pts',(4.27545991072082,5.24811591816364,102.584939281121));
#34322=CARTESIAN_POINT('Ctrl Pts',(4.13982615344022,5.35574434796051,102.593080289525));
#34323=CARTESIAN_POINT('Ctrl Pts',(4.00043295278129,5.45791399623533,102.601221297929));
#34324=CARTESIAN_POINT('Ctrl Pts',(3.86005042176651,5.560808784144,102.609420086387));
#34325=CARTESIAN_POINT('Ctrl Pts',(3.71585519949623,5.65816680806154,102.617618874845));
#34326=CARTESIAN_POINT('Ctrl Pts',(3.56833894735471,5.74971705015051,102.625817663303));
#34327=CARTESIAN_POINT('Ctrl Pts',(3.4208226952133,5.84126729223942,102.634016451762));
#34328=CARTESIAN_POINT('Ctrl Pts',(3.26998576806624,5.92700962529715,102.64221524022));
#34329=CARTESIAN_POINT('Ctrl Pts',(3.11634032552883,6.00672223225636,102.650414028678));
#34330=CARTESIAN_POINT('Ctrl Pts',(3.1106233360721,6.00968825666964,102.650719097194));
#34331=CARTESIAN_POINT('Ctrl Pts',(3.10490180318934,6.01264627953154,102.65102416571));
#34332=CARTESIAN_POINT('Ctrl Pts',(3.09917575053253,6.01559628526642,102.651329234227));
#34333=CARTESIAN_POINT('Origin',(0.,0.,-3.69717978381041));
#34334=CARTESIAN_POINT('',(3.09917575053258,6.0155962852664,105.045751582742));
#34335=CARTESIAN_POINT('',(3.09917575053253,6.01559628526642,104.651558856765));
#34336=CARTESIAN_POINT('',(3.09917575053259,6.01559628526639,-3.69717978381041));
#34337=CARTESIAN_POINT('',(-6.767,5.83999903015602E-12,103.69717978381));
#34338=CARTESIAN_POINT('Ctrl Pts',(-6.767,5.83999902796969E-12,103.69717978381));
#34339=CARTESIAN_POINT('Ctrl Pts',(-6.76700000000016,-0.186007249409826,
103.705929295616));
#34340=CARTESIAN_POINT('Ctrl Pts',(-6.7593263729547,-0.372014355521671,
103.714678807422));
#34341=CARTESIAN_POINT('Ctrl Pts',(-6.74400518266976,-0.557389537149187,
103.723428319228));
#34342=CARTESIAN_POINT('Ctrl Pts',(-6.7286840570971,-0.742763935805548,
103.732177794078));
#34343=CARTESIAN_POINT('Ctrl Pts',(-6.70571545653072,-0.927506129689208,
103.740927268929));
#34344=CARTESIAN_POINT('Ctrl Pts',(-6.67517739415747,-1.11098863924396,
103.749676743779));
#34345=CARTESIAN_POINT('Ctrl Pts',(-6.64463945823177,-1.29447038906111,
103.758426182401));
#34346=CARTESIAN_POINT('Ctrl Pts',(-6.6065321702724,-1.4766921822785,103.767175621023));
#34347=CARTESIAN_POINT('Ctrl Pts',(-6.56098496116798,-1.65703510503779,
103.775925059645));
#34348=CARTESIAN_POINT('Ctrl Pts',(-6.51543793687612,-1.83737729603683,
103.784674462766));
#34349=CARTESIAN_POINT('Ctrl Pts',(-6.46245112202743,-2.01584035396719,
103.793423865886));
#34350=CARTESIAN_POINT('Ctrl Pts',(-6.40220448416355,-2.19181813637813,
103.802173269006));
#34351=CARTESIAN_POINT('Ctrl Pts',(-6.34195808575307,-2.36779521935624,
103.810922637351));
#34352=CARTESIAN_POINT('Ctrl Pts',(-6.2744520148936,-2.54128677544517,103.819672005697));
#34353=CARTESIAN_POINT('Ctrl Pts',(-6.19991555136315,-2.71170355237541,
103.828421374042));
#34354=CARTESIAN_POINT('Ctrl Pts',(-6.12537937789178,-2.88211966612775,
103.837170708339));
#34355=CARTESIAN_POINT('Ctrl Pts',(-6.04381298133765,-3.04946076210151,
103.845920042636));
#34356=CARTESIAN_POINT('Ctrl Pts',(-5.95549339426463,-3.21315848206564,
103.854669376933));
#34357=CARTESIAN_POINT('Ctrl Pts',(-5.86717414355331,-3.37685557859339,
103.863418677909));
#34358=CARTESIAN_POINT('Ctrl Pts',(-5.77210188986423,-3.53690907467009,
103.872167978884));
#34359=CARTESIAN_POINT('Ctrl Pts',(-5.67059953467268,-3.69277536784598,
103.88091727986));
#34360=CARTESIAN_POINT('Ctrl Pts',(-5.56909755761982,-3.84864108035479,
103.889666548241));
#34361=CARTESIAN_POINT('Ctrl Pts',(-5.46116568338304,-4.00031938103959,
103.898415816621));
#34362=CARTESIAN_POINT('Ctrl Pts',(-5.34717048686366,-4.14729511662894,
103.907165085002));
#34363=CARTESIAN_POINT('Ctrl Pts',(-5.23317570555772,-4.2942703168773,103.915914321515));
#34364=CARTESIAN_POINT('Ctrl Pts',(-5.11311782179062,-4.43654275986834,
103.924663558027));
#34365=CARTESIAN_POINT('Ctrl Pts',(-4.98740459172272,-4.57362924147368,
103.93341279454));
#34366=CARTESIAN_POINT('Ctrl Pts',(-4.86169180911094,-4.71071523514164,
103.942161999911));
#34367=CARTESIAN_POINT('Ctrl Pts',(-4.73032391415701,-4.84261509316261,
103.950911205282));
#34368=CARTESIAN_POINT('Ctrl Pts',(-4.59374707237567,-4.9688808433127,103.959660410653));
#34369=CARTESIAN_POINT('Ctrl Pts',(-4.45717070537701,-5.09514615452462,
103.96840958561));
#34370=CARTESIAN_POINT('Ctrl Pts',(-4.31538563819835,-5.21577720253362,
103.977158760566));
#34371=CARTESIAN_POINT('Ctrl Pts',(-4.16887341291001,-5.33036429028374,
103.985907935522));
#34372=CARTESIAN_POINT('Ctrl Pts',(-4.02236168477712,-5.444950989209,103.99465708079));
#34373=CARTESIAN_POINT('Ctrl Pts',(-3.87112305634832,-5.55349359238484,
104.003406226058));
#34374=CARTESIAN_POINT('Ctrl Pts',(-3.71567117317147,-5.65562346102201,
104.012155371326));
#34375=CARTESIAN_POINT('Ctrl Pts',(-3.56021980457718,-5.75775299158512,
104.020904487632));
#34376=CARTESIAN_POINT('Ctrl Pts',(-3.40055544862807,-5.8534696727511,104.029653603938));
#34377=CARTESIAN_POINT('Ctrl Pts',(-3.23722036323823,-5.94244842803333,
104.038402720244));
#34378=CARTESIAN_POINT('Ctrl Pts',(-3.073885804965,-6.03142689616243,104.047151808315));
#34379=CARTESIAN_POINT('Ctrl Pts',(-2.90688079258194,-6.1136673448459,104.055900896386));
#34380=CARTESIAN_POINT('Ctrl Pts',(-2.73677251095136,-6.18889046787072,
104.064649984457));
#34381=CARTESIAN_POINT('Ctrl Pts',(-2.56666476417183,-6.26411335438049,
104.073399045019));
#34382=CARTESIAN_POINT('Ctrl Pts',(-2.39345402972648,-6.3323188435008,104.082148105581));
#34383=CARTESIAN_POINT('Ctrl Pts',(-2.2177285647461,-6.39327529620845,104.090897166144));
#34384=CARTESIAN_POINT('Ctrl Pts',(-2.04200363768856,-6.45423156231896,
104.099646199924));
#34385=CARTESIAN_POINT('Ctrl Pts',(-1.86376426620693,-6.50793874251884,
104.108395233704));
#34386=CARTESIAN_POINT('Ctrl Pts',(-1.68361578195302,-6.55421443795965,
104.117144267484));
#34387=CARTESIAN_POINT('Ctrl Pts',(-1.50346783420474,-6.60048999558542,
104.125893275208));
#34388=CARTESIAN_POINT('Ctrl Pts',(-1.32141106257844,-6.63933404145377,
104.134642282932));
#34389=CARTESIAN_POINT('Ctrl Pts',(-1.13806375959632,-6.6706146552693,104.143391290656));
#34390=CARTESIAN_POINT('Ctrl Pts',(-0.954716987425001,-6.70189517852397,
104.152140273051));
#34391=CARTESIAN_POINT('Ctrl Pts',(-0.770079973815685,-6.72561226535761,
104.160889255446));
#34392=CARTESIAN_POINT('Ctrl Pts',(-0.584779770558221,-6.74168536939732,
104.169638237841));
#34393=CARTESIAN_POINT('Ctrl Pts',(-0.391490647559682,-6.7584514394236,
104.178764418517));
#34394=CARTESIAN_POINT('Ctrl Pts',(-0.197480213110104,-6.7668997592401,
104.187890599193));
#34395=CARTESIAN_POINT('Ctrl Pts',(-0.00346532630355763,-6.76699911271707,
104.197016779869));
#34396=CARTESIAN_POINT('Ctrl Pts',(0.184486595290381,-6.76709536139789,
104.205857767399));
#34397=CARTESIAN_POINT('Ctrl Pts',(0.372442378179646,-6.75935659726801,
104.214698754929));
#34398=CARTESIAN_POINT('Ctrl Pts',(0.559750217716602,-6.74380965729062,
104.223539742459));
#34399=CARTESIAN_POINT('Ctrl Pts',(0.745129914452278,-6.72842275717314,
104.232289721057));
#34400=CARTESIAN_POINT('Ctrl Pts',(0.929874656308724,-6.70538772273549,
104.241039699655));
#34401=CARTESIAN_POINT('Ctrl Pts',(1.11335688289233,-6.67478280180833,104.249789678252));
#34402=CARTESIAN_POINT('Ctrl Pts',(1.29683723118314,-6.64417819418129,104.258539567277));
#34403=CARTESIAN_POINT('Ctrl Pts',(1.47905480729695,-6.60600390230196,104.267289456302));
#34404=CARTESIAN_POINT('Ctrl Pts',(1.65939064804271,-6.5603895979727,104.276039345327));
#34405=CARTESIAN_POINT('Ctrl Pts',(1.83972470263724,-6.51477574543409,104.284789147688));
#34406=CARTESIAN_POINT('Ctrl Pts',(2.01817678125304,-6.46172209820269,104.293538950049));
#34407=CARTESIAN_POINT('Ctrl Pts',(2.19414072347134,-6.40140886724201,104.30228875241));
#34408=CARTESIAN_POINT('Ctrl Pts',(2.37010298131563,-6.34109621361574,104.311038471015));
#34409=CARTESIAN_POINT('Ctrl Pts',(2.54357687926391,-6.27352420826183,104.319788189621));
#34410=CARTESIAN_POINT('Ctrl Pts',(2.71397317789462,-6.19892237325719,104.328537908226));
#34411=CARTESIAN_POINT('Ctrl Pts',(2.88436790206691,-6.12432122757204,104.337287545985));
#34412=CARTESIAN_POINT('Ctrl Pts',(3.05168482125746,-6.04269049717674,104.346037183743));
#34413=CARTESIAN_POINT('Ctrl Pts',(3.21535561996879,-5.95430745235205,104.354786821501));
#34414=CARTESIAN_POINT('Ctrl Pts',(3.37902496074777,-5.86592519481807,104.36353638132));
#34415=CARTESIAN_POINT('Ctrl Pts',(3.53904799384378,-5.77079087940536,104.372285941139));
#34416=CARTESIAN_POINT('Ctrl Pts',(3.69488118814495,-5.66922763747343,104.381035500958));
#34417=CARTESIAN_POINT('Ctrl Pts',(3.85071304610354,-5.56766526649383,104.389784985746));
#34418=CARTESIAN_POINT('Ctrl Pts',(4.002354897055,-5.45967423581057,104.398534470533));
#34419=CARTESIAN_POINT('Ctrl Pts',(4.14929168607198,-5.34562133936683,104.407283955321));
#34420=CARTESIAN_POINT('Ctrl Pts',(4.296227263853,-5.23156938308905,104.416033367984));
#34421=CARTESIAN_POINT('Ctrl Pts',(4.43845763091611,-5.11145583677598,104.424782780647));
#34422=CARTESIAN_POINT('Ctrl Pts',(4.57549970660508,-4.98568866204628,104.43353219331));
#34423=CARTESIAN_POINT('Ctrl Pts',(4.71254069814855,-4.85992248226588,104.442281536757));
#34424=CARTESIAN_POINT('Ctrl Pts',(4.84439326930888,-4.72850295734439,104.451030880203));
#34425=CARTESIAN_POINT('Ctrl Pts',(4.97060959434287,-4.59187644222127,104.459780223649));
#34426=CARTESIAN_POINT('Ctrl Pts',(5.09682496280121,-4.45525096257115,104.468529500786));
#34427=CARTESIAN_POINT('Ctrl Pts',(5.21740397615462,-4.31341878218783,104.477278777922));
#34428=CARTESIAN_POINT('Ctrl Pts',(5.33193710451573,-4.16686161439139,104.486028055058));
#34429=CARTESIAN_POINT('Ctrl Pts',(5.44646940289039,-4.0203055086498,104.494777268791));
#34430=CARTESIAN_POINT('Ctrl Pts',(5.55495572749338,-3.86902470980603,104.503526482524));
#34431=CARTESIAN_POINT('Ctrl Pts',(5.65702762491146,-3.71353301466254,104.512275696257));
#34432=CARTESIAN_POINT('Ctrl Pts',(5.75909881654858,-3.55804239467372,104.521024849493));
#34433=CARTESIAN_POINT('Ctrl Pts',(5.85475551250501,-3.39834117620037,104.529774002729));
#34434=CARTESIAN_POINT('Ctrl Pts',(5.94367283727829,-3.23497174692459,104.538523155966));
#34435=CARTESIAN_POINT('Ctrl Pts',(6.03258957676073,-3.07160339301437,104.547272251611));
#34436=CARTESIAN_POINT('Ctrl Pts',(6.11476689685071,-2.90456712829955,104.556021347257));
#34437=CARTESIAN_POINT('Ctrl Pts',(6.18992570525071,-2.73443024476334,104.564770442902));
#34438=CARTESIAN_POINT('Ctrl Pts',(6.26508404388517,-2.5642944246347,104.573519483863));
#34439=CARTESIAN_POINT('Ctrl Pts',(6.33322384283144,-2.39105828656444,104.582268524824));
#34440=CARTESIAN_POINT('Ctrl Pts',(6.39411368719873,-2.21531017132543,104.591017565785));
#34441=CARTESIAN_POINT('Ctrl Pts',(6.45500317120733,-2.03956309620009,104.599766554968));
#34442=CARTESIAN_POINT('Ctrl Pts',(6.50864269269922,-1.86130434439159,104.60851554415));
#34443=CARTESIAN_POINT('Ctrl Pts',(6.5548500844619,-1.68113930720503,104.617264533332));
#34444=CARTESIAN_POINT('Ctrl Pts',(6.60199664749281,-1.49731239212385,104.626191346862));
#34445=CARTESIAN_POINT('Ctrl Pts',(6.64140563640802,-1.31150116500202,104.635118160391));
#34446=CARTESIAN_POINT('Ctrl Pts',(6.67293772282085,-1.12436255156176,104.644044973921));
#34447=CARTESIAN_POINT('Ctrl Pts',(6.70384494949799,-0.940932395056459,
104.652794888076));
#34448=CARTESIAN_POINT('Ctrl Pts',(6.72718449348873,-0.756227260511783,
104.661544802232));
#34449=CARTESIAN_POINT('Ctrl Pts',(6.7428770737389,-0.570874564546707,104.670294716387));
#34450=CARTESIAN_POINT('Ctrl Pts',(6.75856934538641,-0.385525513637585,
104.679044458471));
#34451=CARTESIAN_POINT('Ctrl Pts',(6.76661493004087,-0.19952921242343,104.687794200555));
#34452=CARTESIAN_POINT('Ctrl Pts',(6.76698649908906,-0.0135174386057119,
104.696543942639));
#34453=CARTESIAN_POINT('Ctrl Pts',(6.76735806132403,0.172490924440569,104.705293524285));
#34454=CARTESIAN_POINT('Ctrl Pts',(6.76005588896317,0.35851447289628,104.714043105931));
#34455=CARTESIAN_POINT('Ctrl Pts',(6.74510478454625,0.543921359657171,104.722792687577));
#34456=CARTESIAN_POINT('Ctrl Pts',(6.73015393440742,0.729325093145469,104.731542120416));
#34457=CARTESIAN_POINT('Ctrl Pts',(6.70755443556964,0.914111900251446,104.740291553255));
#34458=CARTESIAN_POINT('Ctrl Pts',(6.67738304682398,1.09765415591055,104.749040986094));
#34459=CARTESIAN_POINT('Ctrl Pts',(6.64721213111954,1.28119353390787,104.757790281755));
#34460=CARTESIAN_POINT('Ctrl Pts',(6.60946960955602,1.46348811672165,104.766539577417));
#34461=CARTESIAN_POINT('Ctrl Pts',(6.56428366991306,1.64391876347732,104.775288873078));
#34462=CARTESIAN_POINT('Ctrl Pts',(6.51909837867851,1.82434682109239,104.784038043189));
#34463=CARTESIAN_POINT('Ctrl Pts',(6.46646995272065,2.00291071819982,104.7927872133));
#34464=CARTESIAN_POINT('Ctrl Pts',(6.40657713281702,2.17900400212254,104.80153638341));
#34465=CARTESIAN_POINT('Ctrl Pts',(6.34668509279221,2.35509499309224,104.810285439596));
#34466=CARTESIAN_POINT('Ctrl Pts',(6.27952894037695,2.52871516397704,104.819034495782));
#34467=CARTESIAN_POINT('Ctrl Pts',(6.20533675061622,2.69927486771016,104.827783551968));
#34468=CARTESIAN_POINT('Ctrl Pts',(6.12832117908098,2.87632521635538,104.83686555325));
#34469=CARTESIAN_POINT('Ctrl Pts',(6.04372366626265,3.05007728919629,104.845947554532));
#34470=CARTESIAN_POINT('Ctrl Pts',(5.95185378008057,3.21989527477846,104.855029555815));
#34471=CARTESIAN_POINT('Ctrl Pts',(5.86334450817573,3.38350129286403,104.863779336122));
#34472=CARTESIAN_POINT('Ctrl Pts',(5.76808562057469,3.54345567124614,104.872529116429));
#34473=CARTESIAN_POINT('Ctrl Pts',(5.6664006880471,3.69921508464963,104.881278896736));
#34474=CARTESIAN_POINT('Ctrl Pts',(5.56471941108155,3.85496889851948,104.890028362489));
#34475=CARTESIAN_POINT('Ctrl Pts',(5.45661270815352,4.00652780919313,104.898777828243));
#34476=CARTESIAN_POINT('Ctrl Pts',(5.34244776449357,4.15337704568917,104.907527293996));
#34477=CARTESIAN_POINT('Ctrl Pts',(5.22828631819855,4.30022178355933,104.916276491716));
#34478=CARTESIAN_POINT('Ctrl Pts',(5.10806717844347,4.44235690972358,104.925025689436));
#34479=CARTESIAN_POINT('Ctrl Pts',(4.98219864545016,4.57929969070322,104.933774887155));
#34480=CARTESIAN_POINT('Ctrl Pts',(4.85633329944323,4.71623900429694,104.942523863345));
#34481=CARTESIAN_POINT('Ctrl Pts',(4.72481904033947,4.84798602483326,104.951272839536));
#34482=CARTESIAN_POINT('Ctrl Pts',(4.58810250737497,4.9740933225885,104.960021815726));
#34483=CARTESIAN_POINT('Ctrl Pts',(4.45137708685943,5.10020881821873,104.968771360662));
#34484=CARTESIAN_POINT('Ctrl Pts',(4.30944892636354,5.22068366307683,104.977520905598));
#34485=CARTESIAN_POINT('Ctrl Pts',(4.16280009466965,5.33510865604614,104.986270450534));
#34486=CARTESIAN_POINT('Ctrl Pts',(4.01615988349106,5.44952692272657,104.995019481143));
#34487=CARTESIAN_POINT('Ctrl Pts',(3.86479978232562,5.55789587288396,105.003768511751));
#34488=CARTESIAN_POINT('Ctrl Pts',(3.70923383581412,5.65984746713652,105.012517542359));
#34489=CARTESIAN_POINT('Ctrl Pts',(3.55366577799894,5.76180044505164,105.021266691707));
#34490=CARTESIAN_POINT('Ctrl Pts',(3.39389200027203,5.85733573570849,105.030015841055));
#34491=CARTESIAN_POINT('Ctrl Pts',(3.23045513626413,5.94612887621726,105.038764990403));
#34492=CARTESIAN_POINT('Ctrl Pts',(3.18695122151827,5.96976399206556,105.041093854516));
#34493=CARTESIAN_POINT('Ctrl Pts',(3.14318791262789,5.99292165435268,105.043422718629));
#34494=CARTESIAN_POINT('Ctrl Pts',(3.09917575053258,6.0155962852664,105.045751582742));
#34495=CARTESIAN_POINT('Ctrl Pts',(3.09917575053265,6.01559628526636,103.045648009871));
#34496=CARTESIAN_POINT('Ctrl Pts',(2.93620633558397,6.09955651712641,103.054294205853));
#34497=CARTESIAN_POINT('Ctrl Pts',(2.76995739107423,6.1768211836711,103.062940401836));
#34498=CARTESIAN_POINT('Ctrl Pts',(2.60100041795294,6.24716622364161,103.071586597819));
#34499=CARTESIAN_POINT('Ctrl Pts',(2.52687362550646,6.27802882777806,103.075379958716));
#34500=CARTESIAN_POINT('Ctrl Pts',(2.45222578995234,6.30756014579373,103.079173319613));
#34501=CARTESIAN_POINT('Ctrl Pts',(2.37710607410156,6.3357442903316,103.08296668051));
#34502=CARTESIAN_POINT('Ctrl Pts',(2.21423320088169,6.39685251668918,103.091191360028));
#34503=CARTESIAN_POINT('Ctrl Pts',(2.04878781355926,6.45175678425539,103.099416039547));
#34504=CARTESIAN_POINT('Ctrl Pts',(1.88128287079002,6.50023566957938,103.107640719066));
#34505=CARTESIAN_POINT('Ctrl Pts',(1.71395399466591,6.54866359811035,103.115856753516));
#34506=CARTESIAN_POINT('Ctrl Pts',(1.54457021548309,6.59067949479075,103.124072787966));
#34507=CARTESIAN_POINT('Ctrl Pts',(1.3736637611641,6.62611023687838,103.132288822416));
#34508=CARTESIAN_POINT('Ctrl Pts',(1.20290271599981,6.66151083408776,103.140497866571));
#34509=CARTESIAN_POINT('Ctrl Pts',(1.0306219248412,6.69033736284446,103.148706910725));
#34510=CARTESIAN_POINT('Ctrl Pts',(0.857368139471158,6.71246667577723,103.15691595488));
#34511=CARTESIAN_POINT('Ctrl Pts',(0.684227067155946,6.73458159212722,103.165119658508));
#34512=CARTESIAN_POINT('Ctrl Pts',(0.51011461576297,6.75000792612537,103.173323362136));
#34513=CARTESIAN_POINT('Ctrl Pts',(0.335587173082654,6.75867370489672,103.181527065764));
#34514=CARTESIAN_POINT('Ctrl Pts',(0.161138330881639,6.76733558093305,103.189727074758));
#34515=CARTESIAN_POINT('Ctrl Pts',(-0.0137247730234298,6.76924294987574,
103.197927083752));
#34516=CARTESIAN_POINT('Ctrl Pts',(-0.188441097279942,6.76437572528729,
103.206127092746));
#34517=CARTESIAN_POINT('Ctrl Pts',(-0.363143450850669,6.75950888989239,
103.21432644605));
#34518=CARTESIAN_POINT('Ctrl Pts',(-0.537698689905782,6.74786854120877,
103.222525799354));
#34519=CARTESIAN_POINT('Ctrl Pts',(-0.711545861680575,6.72948671792472,
103.230725152658));
#34520=CARTESIAN_POINT('Ctrl Pts',(-0.885391900023208,6.71110501448473,
103.238924452504));
#34521=CARTESIAN_POINT('Ctrl Pts',(-1.05852952363827,6.68598196060847,103.247123752351));
#34522=CARTESIAN_POINT('Ctrl Pts',(-1.23040311181431,6.65420146842863,103.255323052198));
#34523=CARTESIAN_POINT('Ctrl Pts',(-1.40230675898107,6.62241541815501,103.263523786021));
#34524=CARTESIAN_POINT('Ctrl Pts',(-1.57294557772301,6.58396967505265,103.271724519844));
#34525=CARTESIAN_POINT('Ctrl Pts',(-1.74177429048402,6.53899925990277,103.279925253667));
#34526=CARTESIAN_POINT('Ctrl Pts',(-1.91066315723398,6.4940128217091,103.288128909427));
#34527=CARTESIAN_POINT('Ctrl Pts',(-2.07774028702214,6.44249717266287,103.296332565187));
#34528=CARTESIAN_POINT('Ctrl Pts',(-2.2424756550531,6.38463718127304,103.304536220946));
#34529=CARTESIAN_POINT('Ctrl Pts',(-2.40739973803829,6.3267109075435,103.312749274521));
#34530=CARTESIAN_POINT('Ctrl Pts',(-2.56997636116366,6.26242589036879,103.320962328097));
#34531=CARTESIAN_POINT('Ctrl Pts',(-2.72969458793926,6.19201554072461,103.329175381672));
#34532=CARTESIAN_POINT('Ctrl Pts',(-2.88950732357304,6.12156352769684,103.337393295095));
#34533=CARTESIAN_POINT('Ctrl Pts',(-3.04645796963835,6.04497911418334,103.345611208518));
#34534=CARTESIAN_POINT('Ctrl Pts',(-3.20006040701181,5.96254160501002,103.353829121941));
#34535=CARTESIAN_POINT('Ctrl Pts',(-3.35390241237484,5.87997552112997,103.362059852537));
#34536=CARTESIAN_POINT('Ctrl Pts',(-3.50438546420654,5.7915382797772,103.370290583133));
#34537=CARTESIAN_POINT('Ctrl Pts',(-3.6510514950988,5.69755315728926,103.378521313729));
#34538=CARTESIAN_POINT('Ctrl Pts',(-3.78574670354945,5.61123906269109,103.386080255405));
#34539=CARTESIAN_POINT('Ctrl Pts',(-3.91722273601703,5.52024637806843,103.39363919708));
#34540=CARTESIAN_POINT('Ctrl Pts',(-4.04515029016871,5.42485466440789,103.401198138756));
#34541=CARTESIAN_POINT('Ctrl Pts',(-4.18180096016709,5.32295838670253,103.409272509061));
#34542=CARTESIAN_POINT('Ctrl Pts',(-4.31484209244109,5.21571408620643,103.417346879367));
#34543=CARTESIAN_POINT('Ctrl Pts',(-4.44381626277234,5.10340925487268,103.425421249672));
#34544=CARTESIAN_POINT('Ctrl Pts',(-4.57263330685397,4.99124124191827,103.433485783159));
#34545=CARTESIAN_POINT('Ctrl Pts',(-4.69739297015287,4.87402520797903,103.441550316645));
#34546=CARTESIAN_POINT('Ctrl Pts',(-4.8176665367021,4.75209197524004,103.449614850132));
#34547=CARTESIAN_POINT('Ctrl Pts',(-4.93781994293716,4.63028056091864,103.457671326679));
#34548=CARTESIAN_POINT('Ctrl Pts',(-5.05349591220563,4.5037615904889,103.465727803226));
#34549=CARTESIAN_POINT('Ctrl Pts',(-5.16429867510254,4.37290614972859,103.473784279773));
#34550=CARTESIAN_POINT('Ctrl Pts',(-5.27501499522651,4.2421527958374,103.481834471059));
#34551=CARTESIAN_POINT('Ctrl Pts',(-5.38086543664533,4.10706998908007,103.489884662346));
#34552=CARTESIAN_POINT('Ctrl Pts',(-5.48149107981123,3.96806559194148,103.497934853633));
#34553=CARTESIAN_POINT('Ctrl Pts',(-5.58517308236886,3.82483913587916,103.506229557919));
#34554=CARTESIAN_POINT('Ctrl Pts',(-5.68330758303456,3.67744937432671,103.514524262204));
#34555=CARTESIAN_POINT('Ctrl Pts',(-5.77554624560037,3.52637981007881,103.52281896649));
#34556=CARTESIAN_POINT('Ctrl Pts',(-5.86499462276928,3.37988020800635,103.530862750049));
#34557=CARTESIAN_POINT('Ctrl Pts',(-5.94889847941986,3.22992054412356,103.538906533607));
#34558=CARTESIAN_POINT('Ctrl Pts',(-6.02698405823563,3.07697126437242,103.546950317166));
#34559=CARTESIAN_POINT('Ctrl Pts',(-6.10506417863741,2.92403267623042,103.554993538441));
#34560=CARTESIAN_POINT('Ctrl Pts',(-6.17732666058445,2.76810522044496,103.563036759715));
#34561=CARTESIAN_POINT('Ctrl Pts',(-6.2435439618279,2.60968346676804,103.57107998099));
#34562=CARTESIAN_POINT('Ctrl Pts',(-6.30976974087697,2.4512414303431,103.579124232038));
#34563=CARTESIAN_POINT('Ctrl Pts',(-6.36994865513251,2.2903048050044,103.587168483087));
#34564=CARTESIAN_POINT('Ctrl Pts',(-6.42390157633086,2.12738749117643,103.595212734135));
#34565=CARTESIAN_POINT('Ctrl Pts',(-6.47787208641834,1.96441706558902,103.603259607645));
#34566=CARTESIAN_POINT('Ctrl Pts',(-6.52561244701796,1.7994650206104,103.611306481155));
#34567=CARTESIAN_POINT('Ctrl Pts',(-6.56699363240196,1.63305959229667,103.619353354665));
#34568=CARTESIAN_POINT('Ctrl Pts',(-6.60841604447854,1.4664883798138,103.627408245006));
#34569=CARTESIAN_POINT('Ctrl Pts',(-6.64346654456829,1.29846125577211,103.635463135347));
#34570=CARTESIAN_POINT('Ctrl Pts',(-6.67206727133515,1.12951641279722,103.643518025688));
#34571=CARTESIAN_POINT('Ctrl Pts',(-6.70068510948697,0.960470492662015,
103.651577735149));
#34572=CARTESIAN_POINT('Ctrl Pts',(-6.72284544161039,0.790506128862421,
103.659637444609));
#34573=CARTESIAN_POINT('Ctrl Pts',(-6.73852239184888,0.620165280027229,
103.66769715407));
#34574=CARTESIAN_POINT('Ctrl Pts',(-6.75421881387219,0.449612856854959,
103.675766874211));
#34575=CARTESIAN_POINT('Ctrl Pts',(-6.7634157636552,0.278683385992217,103.683836594351));
#34576=CARTESIAN_POINT('Ctrl Pts',(-6.76613942338065,0.107918040077253,
103.691906314492));
#34577=CARTESIAN_POINT('Ctrl Pts',(-6.76671336282573,0.0719337477086487,
103.693606795156));
#34578=CARTESIAN_POINT('Ctrl Pts',(-6.76700004258492,0.0359567218966393,
103.695307275821));
#34579=CARTESIAN_POINT('Ctrl Pts',(-6.76699999999526,-8.01352280423633E-6,
103.697007756485));
#34580=CARTESIAN_POINT('',(-6.76699950316282,0.00259310511624294,103.30282021622));
#34581=CARTESIAN_POINT('Ctrl Pts',(3.09917575053253,6.01559628526642,102.651329234227));
#34582=CARTESIAN_POINT('Ctrl Pts',(2.94465102080322,6.09520589876518,102.659561891668));
#34583=CARTESIAN_POINT('Ctrl Pts',(2.78683225452528,6.16897342073497,102.667794549109));
#34584=CARTESIAN_POINT('Ctrl Pts',(2.6261999455191,6.23661469437992,102.67602720655));
#34585=CARTESIAN_POINT('Ctrl Pts',(2.46575773407981,6.30417591911303,102.684250121193));
#34586=CARTESIAN_POINT('Ctrl Pts',(2.30250893698856,6.36562519448207,102.692473035836));
#34587=CARTESIAN_POINT('Ctrl Pts',(2.13695934262842,6.42072377290545,102.700695950479));
#34588=CARTESIAN_POINT('Ctrl Pts',(1.97157253052235,6.47576817378265,102.708910779662));
#34589=CARTESIAN_POINT('Ctrl Pts',(1.80388976419275,6.52447420150795,102.717125608845));
#34590=CARTESIAN_POINT('Ctrl Pts',(1.63443763868945,6.56665079056556,102.725340438028));
#34591=CARTESIAN_POINT('Ctrl Pts',(1.46511822916006,6.60879434665249,102.733548833305));
#34592=CARTESIAN_POINT('Ctrl Pts',(1.29403256669579,6.64441856386078,102.741757228583));
#34593=CARTESIAN_POINT('Ctrl Pts',(1.12172336251686,6.67338187862675,102.74996562386));
#34594=CARTESIAN_POINT('Ctrl Pts',(0.949514645628381,6.70232830256534,102.758169232165));
#34595=CARTESIAN_POINT('Ctrl Pts',(0.776084160813869,6.72462150336137,102.766372840469));
#34596=CARTESIAN_POINT('Ctrl Pts',(0.601985888318103,6.74017076862789,102.774576448774));
#34597=CARTESIAN_POINT('Ctrl Pts',(0.42793743962812,6.75571558397333,102.782777709353));
#34598=CARTESIAN_POINT('Ctrl Pts',(0.253221939909041,6.76452027247827,102.790978969932));
#34599=CARTESIAN_POINT('Ctrl Pts',(0.0783998453697731,6.76654582961248,
102.799180230511));
#34600=CARTESIAN_POINT('Ctrl Pts',(-0.0963993126394692,6.76857112099508,
102.807380415091));
#34601=CARTESIAN_POINT('Ctrl Pts',(-0.27130467947958,6.76381904749359,102.815580599671));
#34602=CARTESIAN_POINT('Ctrl Pts',(-0.445754415818094,6.75230271839013,
102.823780784251));
#34603=CARTESIAN_POINT('Ctrl Pts',(-0.620212878314131,6.74078581322788,
102.831981379012));
#34604=CARTESIAN_POINT('Ctrl Pts',(-0.794215307374695,6.72250400195956,
102.840181973774));
#34605=CARTESIAN_POINT('Ctrl Pts',(-0.967203545148345,6.69752240028001,
102.848382568535));
#34606=CARTESIAN_POINT('Ctrl Pts',(-1.14023178482971,6.67253502183935,102.856585059608));
#34607=CARTESIAN_POINT('Ctrl Pts',(-1.31224501159702,6.64084481848889,102.86478755068));
#34608=CARTESIAN_POINT('Ctrl Pts',(-1.48269377772703,6.60256830040323,102.872990041752));
#34609=CARTESIAN_POINT('Ctrl Pts',(-1.65330245823249,6.56425587143582,102.88120022837));
#34610=CARTESIAN_POINT('Ctrl Pts',(-1.82234339568558,6.51934486103658,102.889410414987));
#34611=CARTESIAN_POINT('Ctrl Pts',(-1.98927995375338,6.4680023396405,102.897620601605));
#34612=CARTESIAN_POINT('Ctrl Pts',(-2.15629740973563,6.41663493751757,102.905834766902));
#34613=CARTESIAN_POINT('Ctrl Pts',(-2.32120811518539,6.35882992870066,102.914048932198));
#34614=CARTESIAN_POINT('Ctrl Pts',(-2.48349410094345,6.29480309863455,102.922263097495));
#34615=CARTESIAN_POINT('Ctrl Pts',(-2.6459998187415,6.23068957749699,102.93048838461));
#34616=CARTESIAN_POINT('Ctrl Pts',(-2.80587338684529,6.16033754424743,102.938713671725));
#34617=CARTESIAN_POINT('Ctrl Pts',(-2.96261910462237,6.08400994747104,102.946938958841));
#34618=CARTESIAN_POINT('Ctrl Pts',(-3.09778229647575,6.01819199880167,102.954031695256));
#34619=CARTESIAN_POINT('Ctrl Pts',(-3.230619975244,5.94793158111742,102.961124431671));
#34620=CARTESIAN_POINT('Ctrl Pts',(-3.36083145644398,5.87342327108958,102.968217168086));
#34621=CARTESIAN_POINT('Ctrl Pts',(-3.51955779805292,5.782598473144,102.976863134577));
#34622=CARTESIAN_POINT('Ctrl Pts',(-3.67474162686808,5.68525477980905,102.985509101068));
#34623=CARTESIAN_POINT('Ctrl Pts',(-3.82584466453705,5.58168447718369,102.994155067559));
#34624=CARTESIAN_POINT('Ctrl Pts',(-3.97675442087866,5.47824665505559,103.002789974683));
#34625=CARTESIAN_POINT('Ctrl Pts',(-4.12359354450498,5.36859827726257,103.011424881808));
#34626=CARTESIAN_POINT('Ctrl Pts',(-4.26585000875932,5.25307649884981,103.020059788932));
#34627=CARTESIAN_POINT('Ctrl Pts',(-4.41282927280917,5.13371949063343,103.028981368004));
#34628=CARTESIAN_POINT('Ctrl Pts',(-4.55491607446304,5.00809252951917,103.037902947075));
#34629=CARTESIAN_POINT('Ctrl Pts',(-4.69157743729695,4.87661667038185,103.046824526147));
#34630=CARTESIAN_POINT('Ctrl Pts',(-4.82348223191121,4.74971689537142,103.055435585122));
#34631=CARTESIAN_POINT('Ctrl Pts',(-4.95033261604947,4.61736871822652,103.064046644098));
#34632=CARTESIAN_POINT('Ctrl Pts',(-5.0716818674175,4.47999241469319,103.072657703074));
#34633=CARTESIAN_POINT('Ctrl Pts',(-5.19291668083943,4.34274566335603,103.081260641423));
#34634=CARTESIAN_POINT('Ctrl Pts',(-5.3086605034215,4.20048046725272,103.089863579773));
#34635=CARTESIAN_POINT('Ctrl Pts',(-5.4185033873348,4.05365391239081,103.098466518122));
#34636=CARTESIAN_POINT('Ctrl Pts',(-5.52822327262892,3.90699176930382,103.107059823171));
#34637=CARTESIAN_POINT('Ctrl Pts',(-5.63205521911334,3.75577870077789,103.11565312822));
#34638=CARTESIAN_POINT('Ctrl Pts',(-5.72962937647881,3.6005049934962,103.124246433269));
#34639=CARTESIAN_POINT('Ctrl Pts',(-5.74050073473508,3.58320496093413,103.125203868109));
#34640=CARTESIAN_POINT('Ctrl Pts',(-5.75129445271447,3.56585455464649,103.12616130295));
#34641=CARTESIAN_POINT('Ctrl Pts',(-5.76201005039754,3.54845447753213,103.12711873779));
#34642=CARTESIAN_POINT('Ctrl Pts',(-5.85821365169512,3.39223826535554,103.135714495338));
#34643=CARTESIAN_POINT('Ctrl Pts',(-5.94800424912497,3.23219914504976,103.144310252885));
#34644=CARTESIAN_POINT('Ctrl Pts',(-6.03110494216396,3.06888614591767,103.152906010433));
#34645=CARTESIAN_POINT('Ctrl Pts',(-6.11428317097482,2.90542077020509,103.161509788114));
#34646=CARTESIAN_POINT('Ctrl Pts',(-6.1907588978608,2.73867569059632,103.170113565796));
#34647=CARTESIAN_POINT('Ctrl Pts',(-6.26030291329682,2.56922097799457,103.178717343477));
#34648=CARTESIAN_POINT('Ctrl Pts',(-6.33258006935235,2.39310654700761,103.187659257145));
#34649=CARTESIAN_POINT('Ctrl Pts',(-6.39736952032273,2.21406554749393,103.196601170813));
#34650=CARTESIAN_POINT('Ctrl Pts',(-6.45447096379186,2.03275516911598,103.205543084481));
#34651=CARTESIAN_POINT('Ctrl Pts',(-6.50956271757872,1.85782602341062,103.214170286812));
#34652=CARTESIAN_POINT('Ctrl Pts',(-6.55749837040686,1.68078481732085,103.222797489143));
#34653=CARTESIAN_POINT('Ctrl Pts',(-6.59815021984394,1.50223256401043,103.231424691473));
#34654=CARTESIAN_POINT('Ctrl Pts',(-6.63884078394521,1.32351026700897,103.240060109894));
#34655=CARTESIAN_POINT('Ctrl Pts',(-6.67223363982516,1.14327434944384,103.248695528314));
#34656=CARTESIAN_POINT('Ctrl Pts',(-6.69825261285262,0.962133532527059,
103.257330946734));
#34657=CARTESIAN_POINT('Ctrl Pts',(-6.72431002520673,0.78072510585407,103.265979122755));
#34658=CARTESIAN_POINT('Ctrl Pts',(-6.74297174975277,0.598409411195861,
103.274627298777));
#34659=CARTESIAN_POINT('Ctrl Pts',(-6.75421349743395,0.415799267773559,
103.283275474798));
#34660=CARTESIAN_POINT('Ctrl Pts',(-6.75540283171353,0.396479806998448,
103.284190419029));
#34661=CARTESIAN_POINT('Ctrl Pts',(-6.7565091634507,0.377157049266722,103.285105363261));
#34662=CARTESIAN_POINT('Ctrl Pts',(-6.7575324979539,0.357831718964357,103.286020307493));
#34663=CARTESIAN_POINT('Ctrl Pts',(-6.76379587649999,0.239549907070366,
103.291620277059));
#34664=CARTESIAN_POINT('Ctrl Pts',(-6.76695409214459,0.121098237013267,
103.297220246624));
#34665=CARTESIAN_POINT('Ctrl Pts',(-6.76699950316258,0.00259310574074797,
103.30282021619));
#34666=CARTESIAN_POINT('Ctrl Pts',(-6.76699950316282,0.00259310511624744,
103.30282021622));
#34667=CARTESIAN_POINT('Ctrl Pts',(-6.76706574277703,-0.170266619558,103.310988716493));
#34668=CARTESIAN_POINT('Ctrl Pts',(-6.7605043375378,-0.343364296386368,
103.319157216767));
#34669=CARTESIAN_POINT('Ctrl Pts',(-6.74728687381096,-0.516148081947727,
103.327325717041));
#34670=CARTESIAN_POINT('Ctrl Pts',(-6.73408283282203,-0.68875640030021,
103.335485921953));
#34671=CARTESIAN_POINT('Ctrl Pts',(-6.71423621859555,-0.861051102120788,
103.343646126866));
#34672=CARTESIAN_POINT('Ctrl Pts',(-6.68777061728648,-1.03247913807475,
103.351806331778));
#34673=CARTESIAN_POINT('Ctrl Pts',(-6.66132639162829,-1.20376871558966,
103.359959945883));
#34674=CARTESIAN_POINT('Ctrl Pts',(-6.62827387931158,-1.37419266334526,
103.368113559988));
#34675=CARTESIAN_POINT('Ctrl Pts',(-6.58868857281771,-1.54320183074715,
103.376267174092));
#34676=CARTESIAN_POINT('Ctrl Pts',(-6.54912701333018,-1.71210961048463,
103.384415896889));
#34677=CARTESIAN_POINT('Ctrl Pts',(-6.50304054736499,-1.87960394697185,
103.392564619686));
#34678=CARTESIAN_POINT('Ctrl Pts',(-6.45055597016453,-2.04514465888718,
103.400713342482));
#34679=CARTESIAN_POINT('Ctrl Pts',(-6.39604769413584,-2.21706828484309,
103.4091762635));
#34680=CARTESIAN_POINT('Ctrl Pts',(-6.33463814294162,-2.3868842279124,103.417639184517));
#34681=CARTESIAN_POINT('Ctrl Pts',(-6.26652689360036,-2.55400268045738,
103.426102105535));
#34682=CARTESIAN_POINT('Ctrl Pts',(-6.20097048049423,-2.71485256089052,
103.434247584463));
#34683=CARTESIAN_POINT('Ctrl Pts',(-6.12920615613764,-2.87320328257457,
103.442393063392));
#34684=CARTESIAN_POINT('Ctrl Pts',(-6.05146148877742,-3.02854797714082,
103.45053854232));
#34685=CARTESIAN_POINT('Ctrl Pts',(-5.9737115727459,-3.18390315928478,103.458684571164));
#34686=CARTESIAN_POINT('Ctrl Pts',(-5.88998067207161,-3.33625158434668,
103.466830600007));
#34687=CARTESIAN_POINT('Ctrl Pts',(-5.80054284650386,-3.48510999623726,
103.47497662885));
#34688=CARTESIAN_POINT('Ctrl Pts',(-5.71108215100214,-3.63400647235883,
103.483124740695));
#34689=CARTESIAN_POINT('Ctrl Pts',(-5.61591181184105,-3.77941084611467,
103.49127285254));
#34690=CARTESIAN_POINT('Ctrl Pts',(-5.51534982011552,-3.92086793475013,
103.499420964385));
#34691=CARTESIAN_POINT('Ctrl Pts',(-5.41474318760003,-4.0623878180466,103.507572693284));
#34692=CARTESIAN_POINT('Ctrl Pts',(-5.30874034676697,-4.19995663042744,
103.515724422183));
#34693=CARTESIAN_POINT('Ctrl Pts',(-5.19770022153839,-4.33315144058222,
103.523876151082));
#34694=CARTESIAN_POINT('Ctrl Pts',(-5.08653198099771,-4.46649992756902,
103.532037285241));
#34695=CARTESIAN_POINT('Ctrl Pts',(-4.97031508416509,-4.59546405607798,
103.540198419401));
#34696=CARTESIAN_POINT('Ctrl Pts',(-4.84944661176212,-4.7196564027129,103.54835955356));
#34697=CARTESIAN_POINT('Ctrl Pts',(-4.72849558309742,-4.84393357590077,
103.556526261983));
#34698=CARTESIAN_POINT('Ctrl Pts',(-4.60288691110054,-4.96343222345064,
103.564692970406));
#34699=CARTESIAN_POINT('Ctrl Pts',(-4.47305131585109,-5.07780473489902,
103.572859678829));
#34700=CARTESIAN_POINT('Ctrl Pts',(-4.34303828673217,-5.19233354830163,
103.58103754791));
#34701=CARTESIAN_POINT('Ctrl Pts',(-4.20878708258286,-5.30172201124552,
103.589215416991));
#34702=CARTESIAN_POINT('Ctrl Pts',(-4.07075860683747,-5.40566493272185,
103.597393286072));
#34703=CARTESIAN_POINT('Ctrl Pts',(-4.03458189261365,-5.43290795881143,
103.599536673015));
#34704=CARTESIAN_POINT('Ctrl Pts',(-3.99814583848349,-5.45977714901582,
103.601680059958));
#34705=CARTESIAN_POINT('Ctrl Pts',(-3.96145902307961,-5.48626752979301,
103.603823446901));
#34706=CARTESIAN_POINT('Ctrl Pts',(-3.82186789696318,-5.58706183541023,
103.611978905308));
#34707=CARTESIAN_POINT('Ctrl Pts',(-3.67819970009139,-5.68268948867638,
103.620134363715));
#34708=CARTESIAN_POINT('Ctrl Pts',(-3.53087616309073,-5.77279849994071,
103.628289822122));
#34709=CARTESIAN_POINT('Ctrl Pts',(-3.38373193819997,-5.86279783669369,
103.636435354264));
#34710=CARTESIAN_POINT('Ctrl Pts',(-3.23294153755421,-5.94729171315061,
103.644580886406));
#34711=CARTESIAN_POINT('Ctrl Pts',(-3.07895901496569,-6.02596883365335,
103.652726418548));
#34712=CARTESIAN_POINT('Ctrl Pts',(-2.92513152991245,-6.10456673797856,
103.660863749348));
#34713=CARTESIAN_POINT('Ctrl Pts',(-2.76811864444988,-6.17735938076264,
103.669001080149));
#34714=CARTESIAN_POINT('Ctrl Pts',(-2.60840259564971,-6.24407918743892,
103.677138410949));
#34715=CARTESIAN_POINT('Ctrl Pts',(-2.44881379237286,-6.3107458385508,103.685269258751));
#34716=CARTESIAN_POINT('Ctrl Pts',(-2.28652644954427,-6.37134914681978,
103.693400106553));
#34717=CARTESIAN_POINT('Ctrl Pts',(-2.12204656300972,-6.42566785512749,
103.701530954355));
#34718=CARTESIAN_POINT('Ctrl Pts',(-1.95766316549192,-6.47995469839159,
103.709657032349));
#34719=CARTESIAN_POINT('Ctrl Pts',(-1.79109013193453,-6.52796416943831,
103.717783110343));
#34720=CARTESIAN_POINT('Ctrl Pts',(-1.62285255312617,-6.56952346755926,
103.725909188337));
#34721=CARTESIAN_POINT('Ctrl Pts',(-1.45401843459086,-6.61123012736082,
103.734064079919));
#34722=CARTESIAN_POINT('Ctrl Pts',(-1.28350829025956,-6.64644065036041,
103.742218971501));
#34723=CARTESIAN_POINT('Ctrl Pts',(-1.11186784727553,-6.67503100293886,
103.750373863083));
#34724=CARTESIAN_POINT('Ctrl Pts',(-0.940896742006795,-6.70350986313857,
103.758496953439));
#34725=CARTESIAN_POINT('Ctrl Pts',(-0.768804503938351,-6.72542004930831,
103.766620043796));
#34726=CARTESIAN_POINT('Ctrl Pts',(-0.596140021328421,-6.7406903262923,
103.774743134152));
#34727=CARTESIAN_POINT('Ctrl Pts',(-0.423461980314886,-6.75596180236816,
103.78286686237));
#34728=CARTESIAN_POINT('Ctrl Pts',(-0.250211969660003,-6.76459229842574,
103.790990590589));
#34729=CARTESIAN_POINT('Ctrl Pts',(-0.0769430694369275,-6.76656255155198,
103.799114318807));
#34730=CARTESIAN_POINT('Ctrl Pts',(0.0963724008534442,-6.76853333422981,
103.807240230468));
#34731=CARTESIAN_POINT('Ctrl Pts',(0.269706405172214,-6.7638403054025,103.815366142128));
#34732=CARTESIAN_POINT('Ctrl Pts',(0.442506837496675,-6.75251632347296,
103.823492053788));
#34733=CARTESIAN_POINT('Ctrl Pts',(0.616412346548741,-6.74111992350183,
103.831669931498));
#34734=CARTESIAN_POINT('Ctrl Pts',(0.789777060626473,-6.72300748934226,
103.839847809208));
#34735=CARTESIAN_POINT('Ctrl Pts',(0.962045255402203,-6.69826529233936,
103.848025686919));
#34736=CARTESIAN_POINT('Ctrl Pts',(1.13349125144722,-6.67364118447647,103.856164533392));
#34737=CARTESIAN_POINT('Ctrl Pts',(1.30385082336201,-6.64245058633746,103.864303379865));
#34738=CARTESIAN_POINT('Ctrl Pts',(1.47258852360663,-6.60482944822514,103.872442226339));
#34739=CARTESIAN_POINT('Ctrl Pts',(1.64254003980044,-6.56693768216541,103.880639619667));
#34740=CARTESIAN_POINT('Ctrl Pts',(1.81084589720142,-6.52252260743711,103.888837012996));
#34741=CARTESIAN_POINT('Ctrl Pts',(1.97697700707738,-6.47177339787846,103.897034406324));
#34742=CARTESIAN_POINT('Ctrl Pts',(2.14310811695347,-6.42102418831978,103.905231799652));
#34743=CARTESIAN_POINT('Ctrl Pts',(2.30706414786201,-6.36394102403529,103.913429192981));
#34744=CARTESIAN_POINT('Ctrl Pts',(2.46833918939741,-6.30076111641165,103.921626586309));
#34745=CARTESIAN_POINT('Ctrl Pts',(2.63018115541685,-6.23735911467977,103.929852795646));
#34746=CARTESIAN_POINT('Ctrl Pts',(2.78980496348707,-6.16762884505108,103.938079004983));
#34747=CARTESIAN_POINT('Ctrl Pts',(2.94668072219698,-6.0917453756237,103.94630521432));
#34748=CARTESIAN_POINT('Ctrl Pts',(3.1033802377122,-6.01594715802353,103.954522181863));
#34749=CARTESIAN_POINT('Ctrl Pts',(3.2573375316345,-5.93400966074938,103.962739149406));
#34750=CARTESIAN_POINT('Ctrl Pts',(3.40804033492672,-5.84615686374498,103.97095611695));
#34751=CARTESIAN_POINT('Ctrl Pts',(3.55860407733491,-5.75838513283458,103.979165502293));
#34752=CARTESIAN_POINT('Ctrl Pts',(3.70591900196913,-5.66470915216056,103.987374887636));
#34753=CARTESIAN_POINT('Ctrl Pts',(3.84949512797683,-5.56539991911477,103.99558427298));
#34754=CARTESIAN_POINT('Ctrl Pts',(3.99296757686672,-5.46616239781758,104.00378773028));
#34755=CARTESIAN_POINT('Ctrl Pts',(4.13270631092355,-5.36129992970159,104.011991187581));
#34756=CARTESIAN_POINT('Ctrl Pts',(4.26824809427468,-5.25112818408773,104.020194644882));
#34757=CARTESIAN_POINT('Ctrl Pts',(4.40371919149893,-5.14101389392265,104.028393824013));
#34758=CARTESIAN_POINT('Ctrl Pts',(4.53499742074772,-5.02559606793333,104.036593003145));
#34759=CARTESIAN_POINT('Ctrl Pts',(4.6616504952531,-4.90523227381808,104.044792182277));
#34760=CARTESIAN_POINT('Ctrl Pts',(4.78827970558998,-4.78489115883538,104.052989816507));
#34761=CARTESIAN_POINT('Ctrl Pts',(4.91028523309642,-4.65960617432333,104.061187450737));
#34762=CARTESIAN_POINT('Ctrl Pts',(5.02726949482033,-4.52977377210484,104.069385084966));
#34763=CARTESIAN_POINT('Ctrl Pts',(5.14424531249196,-4.39995074133151,104.077582127482));
#34764=CARTESIAN_POINT('Ctrl Pts',(5.25620034544828,-4.26558121242906,104.085779169998));
#34765=CARTESIAN_POINT('Ctrl Pts',(5.36277541842275,-4.12709689873653,104.093976212513));
#34766=CARTESIAN_POINT('Ctrl Pts',(5.46936216853308,-3.98859741170093,104.102174153156));
#34767=CARTESIAN_POINT('Ctrl Pts',(5.57056756547256,-3.84598252596951,104.110372093799));
#34768=CARTESIAN_POINT('Ctrl Pts',(5.66607408704463,-3.69971531879432,104.118570034442));
#34769=CARTESIAN_POINT('Ctrl Pts',(5.76160843121589,-3.55340550160872,104.126770363278));
#34770=CARTESIAN_POINT('Ctrl Pts',(5.85144039710096,-3.40344154390989,104.134970692114));
#34771=CARTESIAN_POINT('Ctrl Pts',(5.93529695554827,-3.25031368477867,104.14317102095));
#34772=CARTESIAN_POINT('Ctrl Pts',(6.01924089470567,-3.09702626244435,104.151379894741));
#34773=CARTESIAN_POINT('Ctrl Pts',(6.09719681425231,-2.94056866704617,104.159588768533));
#34774=CARTESIAN_POINT('Ctrl Pts',(6.16893821169109,-2.78145471657144,104.167797642324));
#34775=CARTESIAN_POINT('Ctrl Pts',(6.24071811194648,-2.62225537139473,104.176010921727));
#34776=CARTESIAN_POINT('Ctrl Pts',(6.30627670660361,-2.46039716120847,104.184224201131));
#34777=CARTESIAN_POINT('Ctrl Pts',(6.36543651163292,-2.29641176977704,104.192437480534));
#34778=CARTESIAN_POINT('Ctrl Pts',(6.42468284717531,-2.13218652393684,104.20066277315));
#34779=CARTESIAN_POINT('Ctrl Pts',(6.47751158071383,-1.96582822088184,104.208888065765));
#34780=CARTESIAN_POINT('Ctrl Pts',(6.52379541334976,-1.79788275612082,104.217113358381));
#34781=CARTESIAN_POINT('Ctrl Pts',(6.56565358015001,-1.64599625759747,104.224552147493));
#34782=CARTESIAN_POINT('Ctrl Pts',(6.60215927446537,-1.49281195096278,104.231990936605));
#34783=CARTESIAN_POINT('Ctrl Pts',(6.63325475579004,-1.33873834067336,104.239429725717));
#34784=CARTESIAN_POINT('Ctrl Pts',(6.66764176102705,-1.16835570569849,104.247655926736));
#34785=CARTESIAN_POINT('Ctrl Pts',(6.69550790612459,-0.996409170636312,
104.255882127755));
#34786=CARTESIAN_POINT('Ctrl Pts',(6.71671327765216,-0.823438975159202,
104.264108328773));
#34787=CARTESIAN_POINT('Ctrl Pts',(6.73789482941407,-0.65066307524144,104.272325289389));
#34788=CARTESIAN_POINT('Ctrl Pts',(6.75243046300857,-0.47686615734503,104.280542250005));
#34789=CARTESIAN_POINT('Ctrl Pts',(6.76023092441601,-0.30260014634741,104.288759210621));
#34790=CARTESIAN_POINT('Ctrl Pts',(6.76802418926368,-0.128494909911465,
104.296968590422));
#34791=CARTESIAN_POINT('Ctrl Pts',(6.76909464089102,0.0460782017084419,
104.305177970224));
#34792=CARTESIAN_POINT('Ctrl Pts',(6.76340462002218,0.220560526528714,104.313387350026));
#34793=CARTESIAN_POINT('Ctrl Pts',(6.75771870699421,0.394916885971801,104.321590803166));
#34794=CARTESIAN_POINT('Ctrl Pts',(6.74528205451015,0.569182232170582,104.329794256306));
#34795=CARTESIAN_POINT('Ctrl Pts',(6.7261090409509,0.742796182837956,104.337997709447));
#34796=CARTESIAN_POINT('Ctrl Pts',(6.70694602305525,0.916319621565553,104.346196885797));
#34797=CARTESIAN_POINT('Ctrl Pts',(6.68105367976009,1.08919198568131,104.354396062147));
#34798=CARTESIAN_POINT('Ctrl Pts',(6.64849837335323,1.26085620889911,104.362595238497));
#34799=CARTESIAN_POINT('Ctrl Pts',(6.6159491927186,1.43248813090258,104.370792872049));
#34800=CARTESIAN_POINT('Ctrl Pts',(6.57673960692468,1.60291201167313,104.3789905056));
#34801=CARTESIAN_POINT('Ctrl Pts',(6.53098746266332,1.7715788897293,104.387188139151));
#34802=CARTESIAN_POINT('Ctrl Pts',(6.48523861367921,1.94023361963083,104.395385182272));
#34803=CARTESIAN_POINT('Ctrl Pts',(6.43294823774539,2.10713125244343,104.403582225392));
#34804=CARTESIAN_POINT('Ctrl Pts',(6.37428462750736,2.27173600744526,104.411779268513));
#34805=CARTESIAN_POINT('Ctrl Pts',(6.31561458047564,2.43635882350479,104.419977211044));
#34806=CARTESIAN_POINT('Ctrl Pts',(6.25057002637754,2.59868792259207,104.428175153575));
#34807=CARTESIAN_POINT('Ctrl Pts',(6.17936818585291,2.7582055441299,104.436373096107));
#34808=CARTESIAN_POINT('Ctrl Pts',(6.10814559192847,2.91776966071552,104.444573428115));
#34809=CARTESIAN_POINT('Ctrl Pts',(6.03076228294856,3.07452034001717,104.452773760124));
#34810=CARTESIAN_POINT('Ctrl Pts',(5.94748241403092,3.22796250517148,104.460974092132));
#34811=CARTESIAN_POINT('Ctrl Pts',(5.86411574498172,3.38156459853289,104.469182971103));
#34812=CARTESIAN_POINT('Ctrl Pts',(5.77484040891931,3.53185097277528,104.477391850074));
#34813=CARTESIAN_POINT('Ctrl Pts',(5.67996558559512,3.67835288498196,104.485600729044));
#34814=CARTESIAN_POINT('Ctrl Pts',(5.58503983126507,3.82493344281334,104.493814014732));
#34815=CARTESIAN_POINT('Ctrl Pts',(5.4845088035225,3.96772519557063,104.502027300419));
#34816=CARTESIAN_POINT('Ctrl Pts',(5.37872325443189,4.10629092396456,104.510240586106));
#34817=CARTESIAN_POINT('Ctrl Pts',(5.27278295412074,4.24505935694127,104.518465886818));
#34818=CARTESIAN_POINT('Ctrl Pts',(5.16157299957407,4.37958913449246,104.526691187531));
#34819=CARTESIAN_POINT('Ctrl Pts',(5.04548327590348,4.50947752101929,104.534916488243));
#34820=CARTESIAN_POINT('Ctrl Pts',(4.94049412449559,4.62694589847781,104.542355280536));
#34821=CARTESIAN_POINT('Ctrl Pts',(4.83151441907065,4.74061841286867,104.54979407283));
#34822=CARTESIAN_POINT('Ctrl Pts',(4.71885624377911,4.85022522678555,104.557232865124));
#34823=CARTESIAN_POINT('Ctrl Pts',(4.59540267829461,4.9703350363437,104.565384474443));
#34824=CARTESIAN_POINT('Ctrl Pts',(4.46716728355509,5.0859161893053,104.573536083762));
#34825=CARTESIAN_POINT('Ctrl Pts',(4.33451801718587,5.19656064707139,104.581687693081));
#34826=CARTESIAN_POINT('Ctrl Pts',(4.20200393016589,5.3070923500051,104.589830995312));
#34827=CARTESIAN_POINT('Ctrl Pts',(4.06508519780222,5.41269713461875,104.597974297542));
#34828=CARTESIAN_POINT('Ctrl Pts',(3.92416764446704,5.51300256648933,104.606117599772));
#34829=CARTESIAN_POINT('Ctrl Pts',(3.78339917756085,5.61320187830396,104.614252286639));
#34830=CARTESIAN_POINT('Ctrl Pts',(3.63864061179269,5.70811279368045,104.622386973507));
#34831=CARTESIAN_POINT('Ctrl Pts',(3.49033166315081,5.79740233908317,104.630521660374));
#34832=CARTESIAN_POINT('Ctrl Pts',(3.36248390330737,5.87437320605857,104.637534059171));
#34833=CARTESIAN_POINT('Ctrl Pts',(3.2319984966419,5.94716731923532,104.644546457968));
#34834=CARTESIAN_POINT('Ctrl Pts',(3.09917575053253,6.01559628526642,104.651558856765));
#34835=CARTESIAN_POINT('Origin',(0.,0.,-3.69717978381041));
#34836=CARTESIAN_POINT('',(3.0991757505325,6.01559628526643,107.045813349661));
#34837=CARTESIAN_POINT('',(3.09917575053261,6.01559628526638,106.651392015122));
#34838=CARTESIAN_POINT('',(3.09917575053259,6.01559628526639,-3.69717978381041));
#34839=CARTESIAN_POINT('',(-6.76699999997695,1.76623100267976E-5,105.69756051241));
#34840=CARTESIAN_POINT('Ctrl Pts',(-6.76699999997695,1.76623100267975E-5,
105.69756051241));
#34841=CARTESIAN_POINT('Ctrl Pts',(-6.76700044466366,-0.170356143476382,
105.705581476401));
#34842=CARTESIAN_POINT('Ctrl Pts',(-6.76056227767791,-0.340943091970037,
105.713602440391));
#34843=CARTESIAN_POINT('Ctrl Pts',(-6.747663184599,-0.511204995287844,105.721623404382));
#34844=CARTESIAN_POINT('Ctrl Pts',(-6.73477403793164,-0.681335610696416,
105.729638183456));
#34845=CARTESIAN_POINT('Ctrl Pts',(-6.71543390845697,-0.85114130644225,
105.737652962531));
#34846=CARTESIAN_POINT('Ctrl Pts',(-6.68967254174539,-1.02008346924053,
105.745667741605));
#34847=CARTESIAN_POINT('Ctrl Pts',(-6.66270217275019,-1.19695422771114,
105.754058660902));
#34848=CARTESIAN_POINT('Ctrl Pts',(-6.62869328459728,-1.37287802099367,
105.762449580199));
#34849=CARTESIAN_POINT('Ctrl Pts',(-6.5877410844805,-1.54724154670424,105.770840499496));
#34850=CARTESIAN_POINT('Ctrl Pts',(-6.54865406306637,-1.71366363987277,
105.778849252171));
#34851=CARTESIAN_POINT('Ctrl Pts',(-6.50324228412838,-1.87866403626064,
105.786858004846));
#34852=CARTESIAN_POINT('Ctrl Pts',(-6.45164093027403,-2.04171944860524,
105.794866757521));
#34853=CARTESIAN_POINT('Ctrl Pts',(-6.40004205710617,-2.20476702221444,
105.802875125183));
#34854=CARTESIAN_POINT('Ctrl Pts',(-6.34225431417973,-2.36586943871361,
105.810883492845));
#34855=CARTESIAN_POINT('Ctrl Pts',(-6.27846270017658,-2.52451879028288,
105.818891860507));
#34856=CARTESIAN_POINT('Ctrl Pts',(-6.21466134671133,-2.68319236383449,
105.826901450857));
#34857=CARTESIAN_POINT('Ctrl Pts',(-6.14485443867364,-2.83941177790795,
105.834911041206));
#34858=CARTESIAN_POINT('Ctrl Pts',(-6.06927496196964,-2.99268949876335,
105.842920631555));
#34859=CARTESIAN_POINT('Ctrl Pts',(-5.99366876803175,-3.14602140306771,
105.850933053283));
#34860=CARTESIAN_POINT('Ctrl Pts',(-5.91228611141086,-3.2964092076703,105.85894547501));
#34861=CARTESIAN_POINT('Ctrl Pts',(-5.82540562324274,-3.44339052747315,
105.866957896738));
#34862=CARTESIAN_POINT('Ctrl Pts',(-5.73843226888166,-3.59052895499829,
105.87497888291));
#34863=CARTESIAN_POINT('Ctrl Pts',(-5.6459495436579,-3.73425330528655,105.882999869082));
#34864=CARTESIAN_POINT('Ctrl Pts',(-5.54827940201112,-3.87413018330814,
105.891020855254));
#34865=CARTESIAN_POINT('Ctrl Pts',(-5.45054816258855,-4.01409456162396,
105.899046858972));
#34866=CARTESIAN_POINT('Ctrl Pts',(-5.34762327212463,-4.15020637693373,
105.90707286269));
#34867=CARTESIAN_POINT('Ctrl Pts',(-5.23986615537025,-4.28206628554549,
105.915098866407));
#34868=CARTESIAN_POINT('Ctrl Pts',(-5.13196415113807,-4.41410348963581,
105.923135661686));
#34869=CARTESIAN_POINT('Ctrl Pts',(-5.01921720128658,-4.54187709697175,
105.931172456964));
#34870=CARTESIAN_POINT('Ctrl Pts',(-4.90202308582014,-4.66502504452938,
105.939209252242));
#34871=CARTESIAN_POINT('Ctrl Pts',(-4.86391226420427,-4.70507201653861,
105.941822769738));
#34872=CARTESIAN_POINT('Ctrl Pts',(-4.8253314061741,-4.74463014141675,105.944436287234));
#34873=CARTESIAN_POINT('Ctrl Pts',(-4.78629490478964,-4.78368791670033,
105.94704980473));
#34874=CARTESIAN_POINT('Ctrl Pts',(-4.66344512132277,-4.9066046501706,105.955274672408));
#34875=CARTESIAN_POINT('Ctrl Pts',(-4.53568489280584,-5.02495855146323,
105.963499540086));
#34876=CARTESIAN_POINT('Ctrl Pts',(-4.40338642834206,-5.13833406491764,
105.971724407763));
#34877=CARTESIAN_POINT('Ctrl Pts',(-4.27123701290651,-5.25158184816615,
105.979940009207));
#34878=CARTESIAN_POINT('Ctrl Pts',(-4.13455981241164,-5.35986218062053,
105.98815561065));
#34879=CARTESIAN_POINT('Ctrl Pts',(-3.9937648242292,-5.46279521204571,105.996371212094));
#34880=CARTESIAN_POINT('Ctrl Pts',(-3.85310016882183,-5.56563295920115,
106.004579208422));
#34881=CARTESIAN_POINT('Ctrl Pts',(-3.70832560480854,-5.66313305285339,
106.01278720475));
#34882=CARTESIAN_POINT('Ctrl Pts',(-3.55988531489514,-5.75495486904927,
106.020995201078));
#34883=CARTESIAN_POINT('Ctrl Pts',(-3.41155261994671,-5.84671012942597,
106.02919724795));
#34884=CARTESIAN_POINT('Ctrl Pts',(-3.25955979532231,-5.93279512231752,
106.037399294821));
#34885=CARTESIAN_POINT('Ctrl Pts',(-3.10438127590678,-6.01291159870153,
106.045601341693));
#34886=CARTESIAN_POINT('Ctrl Pts',(-2.94928407433597,-6.09298609183161,
106.053799090464));
#34887=CARTESIAN_POINT('Ctrl Pts',(-2.79100482170631,-6.16709813507121,
106.061996839236));
#34888=CARTESIAN_POINT('Ctrl Pts',(-2.63004398036768,-6.23499459994407,
106.070194588007));
#34889=CARTESIAN_POINT('Ctrl Pts',(-2.46911383907699,-6.30287811492981,
106.078390773223));
#34890=CARTESIAN_POINT('Ctrl Pts',(-2.30550345565305,-6.36454826788074,
106.086586958439));
#34891=CARTESIAN_POINT('Ctrl Pts',(-2.13973505400837,-6.41979928803446,
106.094783143654));
#34892=CARTESIAN_POINT('Ctrl Pts',(-1.97397891553591,-6.47504622084242,
106.102978722534));
#34893=CARTESIAN_POINT('Ctrl Pts',(-1.80606541691134,-6.52387485226607,
106.111174301415));
#34894=CARTESIAN_POINT('Ctrl Pts',(-1.63653374083831,-6.56612871600137,
106.119369880295));
#34895=CARTESIAN_POINT('Ctrl Pts',(-1.46698376205527,-6.60838714148131,
106.127566343974));
#34896=CARTESIAN_POINT('Ctrl Pts',(-1.29581560601942,-6.6440692983082,106.135762807652));
#34897=CARTESIAN_POINT('Ctrl Pts',(-1.12358054209639,-6.673069441076,106.14395927133));
#34898=CARTESIAN_POINT('Ctrl Pts',(-0.951295547343085,-6.70207799096587,
106.152158111158));
#34899=CARTESIAN_POINT('Ctrl Pts',(-0.777943382385791,-6.7244006087548,
106.160356950986));
#34900=CARTESIAN_POINT('Ctrl Pts',(-0.604082414082601,-6.73998319263454,
106.168555790814));
#34901=CARTESIAN_POINT('Ctrl Pts',(-0.430039843051825,-6.75558205296647,
106.176763194563));
#34902=CARTESIAN_POINT('Ctrl Pts',(-0.255487764764599,-6.76442678199833,
106.184970598312));
#34903=CARTESIAN_POINT('Ctrl Pts',(-0.0809875503417063,-6.76651535257917,
106.193178002062));
#34904=CARTESIAN_POINT('Ctrl Pts',(0.0936061356304104,-6.76860504190894,
106.201389802131));
#34905=CARTESIAN_POINT('Ctrl Pts',(0.268147543993728,-6.76393136790142,
106.2096016022));
#34906=CARTESIAN_POINT('Ctrl Pts',(0.4420785402835,-6.75254437706416,106.217813402269));
#34907=CARTESIAN_POINT('Ctrl Pts',(0.616265587303113,-6.74114062298529,
106.226037291255));
#34908=CARTESIAN_POINT('Ctrl Pts',(0.789840069506157,-6.7230038385874,106.234261180241));
#34909=CARTESIAN_POINT('Ctrl Pts',(0.962250890148902,-6.69823575461536,
106.242485069227));
#34910=CARTESIAN_POINT('Ctrl Pts',(1.12155550781551,-6.67535047321139,106.250083800477));
#34911=CARTESIAN_POINT('Ctrl Pts',(1.27986654957716,-6.64680436916413,106.257682531727));
#34912=CARTESIAN_POINT('Ctrl Pts',(1.43676036062567,-6.61271568012226,106.265281262977));
#34913=CARTESIAN_POINT('Ctrl Pts',(1.6065818421427,-6.57581816557165,106.273506111299));
#34914=CARTESIAN_POINT('Ctrl Pts',(1.77521940266211,-6.53232287046059,106.281730959621));
#34915=CARTESIAN_POINT('Ctrl Pts',(1.94212222556167,-6.48231827828435,106.289955807943));
#34916=CARTESIAN_POINT('Ctrl Pts',(2.10883707887704,-6.43237000236589,106.298171393263));
#34917=CARTESIAN_POINT('Ctrl Pts',(2.27382074434021,-6.37592712912642,106.306386978582));
#34918=CARTESIAN_POINT('Ctrl Pts',(2.43653201563181,-6.31312923491997,106.314602563901));
#34919=CARTESIAN_POINT('Ctrl Pts',(2.59909272988927,-6.25038944771882,106.322810547324));
#34920=CARTESIAN_POINT('Ctrl Pts',(2.75938490484714,-6.18130647867979,106.331018530747));
#34921=CARTESIAN_POINT('Ctrl Pts',(2.91688185424882,-6.10606986926566,106.339226514171));
#34922=CARTESIAN_POINT('Ctrl Pts',(3.07426470550153,-6.03088776476672,106.347428551347));
#34923=CARTESIAN_POINT('Ctrl Pts',(3.22885604218162,-5.9495610533771,106.355630588524));
#34924=CARTESIAN_POINT('Ctrl Pts',(3.38014847323695,-5.86232763489673,106.3638326257));
#34925=CARTESIAN_POINT('Ctrl Pts',(3.53136168184899,-5.77513989513605,106.37203036798));
#34926=CARTESIAN_POINT('Ctrl Pts',(3.67927911608528,-5.68205178877099,106.380228110259));
#34927=CARTESIAN_POINT('Ctrl Pts',(3.8234172737882,-5.58334750400672,106.388425852539));
#34928=CARTESIAN_POINT('Ctrl Pts',(3.96752802600509,-5.48466198622921,106.396622036153));
#34929=CARTESIAN_POINT('Ctrl Pts',(4.10786063374422,-5.38036261438356,106.404818219767));
#34930=CARTESIAN_POINT('Ctrl Pts',(4.24395967166901,-5.27077748584088,106.413014403382));
#34931=CARTESIAN_POINT('Ctrl Pts',(4.3800486908057,-5.16120042429263,106.421209983642));
#34932=CARTESIAN_POINT('Ctrl Pts',(4.51190448073893,-5.04633860530262,106.429405563903));
#34933=CARTESIAN_POINT('Ctrl Pts',(4.63910392739835,-4.92656104709941,106.437601144164));
#34934=CARTESIAN_POINT('Ctrl Pts',(4.76631715283842,-4.80677051408582,106.445797612205));
#34935=CARTESIAN_POINT('Ctrl Pts',(4.88887276880498,-4.68206342701493,106.453994080246));
#34936=CARTESIAN_POINT('Ctrl Pts',(5.00638379795321,-4.55284639182914,106.462190548286));
#34937=CARTESIAN_POINT('Ctrl Pts',(5.12392893622362,-4.42359184969891,106.47038939546));
#34938=CARTESIAN_POINT('Ctrl Pts',(5.23642632970017,-4.2898250173541,106.478588242633));
#34939=CARTESIAN_POINT('Ctrl Pts',(5.34352861111647,-4.1519863899319,106.486787089807));
#34940=CARTESIAN_POINT('Ctrl Pts',(5.4507428248317,-4.01400370774033,106.494994505573));
#34941=CARTESIAN_POINT('Ctrl Pts',(5.55255044120691,-3.87194101242286,106.503201921339));
#34942=CARTESIAN_POINT('Ctrl Pts',(5.64864627826914,-3.72626947804318,106.511409337105));
#34943=CARTESIAN_POINT('Ctrl Pts',(5.74479361932023,-3.58051986884452,106.519621151757));
#34944=CARTESIAN_POINT('Ctrl Pts',(5.83522289259002,-3.43115787135136,106.527832966409));
#34945=CARTESIAN_POINT('Ctrl Pts',(5.91967447460793,-3.27868008727222,106.536044781061));
#34946=CARTESIAN_POINT('Ctrl Pts',(6.004250424419,-3.12597775647578,106.544268688859));
#34947=CARTESIAN_POINT('Ctrl Pts',(6.08283092874094,-2.97015078956756,106.552492596656));
#34948=CARTESIAN_POINT('Ctrl Pts',(6.15520364966004,-2.81171780789105,106.560716504454));
#34949=CARTESIAN_POINT('Ctrl Pts',(6.22207470718817,-2.66532865880982,106.568315243377));
#34950=CARTESIAN_POINT('Ctrl Pts',(6.28364637551961,-2.5167150653473,106.575913982301));
#34951=CARTESIAN_POINT('Ctrl Pts',(6.33978909926604,-2.36629735596088,106.583512721224));
#34952=CARTESIAN_POINT('Ctrl Pts',(6.40001203166125,-2.20494794255636,106.591663703398));
#34953=CARTESIAN_POINT('Ctrl Pts',(6.45416596335491,-2.04104452900994,106.599814685573));
#34954=CARTESIAN_POINT('Ctrl Pts',(6.50202534328628,-1.87508811399969,106.607965667747));
#34955=CARTESIAN_POINT('Ctrl Pts',(6.54982913011222,-1.70932447274641,106.6161071818));
#34956=CARTESIAN_POINT('Ctrl Pts',(6.59135281938823,-1.54151292483798,106.624248695853));
#34957=CARTESIAN_POINT('Ctrl Pts',(6.6264187797736,-1.37217460808156,106.632390209906));
#34958=CARTESIAN_POINT('Ctrl Pts',(6.66145138696019,-1.20299735848194,106.640523980109));
#34959=CARTESIAN_POINT('Ctrl Pts',(6.69003842004142,-1.03229658677865,106.648657750312));
#34960=CARTESIAN_POINT('Ctrl Pts',(6.71205196314816,-0.860608763608052,
106.656791520515));
#34961=CARTESIAN_POINT('Ctrl Pts',(6.73404919784243,-0.689048132858079,
106.664919264933));
#34962=CARTESIAN_POINT('Ctrl Pts',(6.74948259292692,-0.516502267864114,
106.673047009351));
#34963=CARTESIAN_POINT('Ctrl Pts',(6.75827525172114,-0.343518008223105,
106.681174753769));
#34964=CARTESIAN_POINT('Ctrl Pts',(6.7670632451925,-0.170625532812691,106.689298185663));
#34965=CARTESIAN_POINT('Ctrl Pts',(6.76921750103009,0.00270450957563728,
106.697421617557));
#34966=CARTESIAN_POINT('Ctrl Pts',(6.76471293997549,0.175919981037493,106.705545049451));
#34967=CARTESIAN_POINT('Ctrl Pts',(6.76017980375731,0.350234263320476,106.713720013202));
#34968=CARTESIAN_POINT('Ctrl Pts',(6.74890303522488,0.524432143122847,106.721894976953));
#34969=CARTESIAN_POINT('Ctrl Pts',(6.73091037817121,0.697950199532255,106.730069940704));
#34970=CARTESIAN_POINT('Ctrl Pts',(6.71303519570248,0.870335351468791,106.738191529877));
#34971=CARTESIAN_POINT('Ctrl Pts',(6.68853162470116,1.04204916537469,106.74631311905));
#34972=CARTESIAN_POINT('Ctrl Pts',(6.65747895546655,1.2125440023026,106.754434708223));
#34973=CARTESIAN_POINT('Ctrl Pts',(6.62642218664269,1.38306134804596,106.762557369612));
#34974=CARTESIAN_POINT('Ctrl Pts',(6.58881466301032,1.55235903616866,106.770680031002));
#34975=CARTESIAN_POINT('Ctrl Pts',(6.54478684632054,1.71989945526758,106.778802692391));
#34976=CARTESIAN_POINT('Ctrl Pts',(6.50074483285733,1.88749389778959,106.786927972933));
#34977=CARTESIAN_POINT('Ctrl Pts',(6.45027849685564,2.05332958916554,106.795053253476));
#34978=CARTESIAN_POINT('Ctrl Pts',(6.39356821373546,2.2168839609487,106.803178534018));
#34979=CARTESIAN_POINT('Ctrl Pts',(6.33624008384824,2.38222022367442,106.811392337806));
#34980=CARTESIAN_POINT('Ctrl Pts',(6.27253128256514,2.54522480365822,106.819606141593));
#34981=CARTESIAN_POINT('Ctrl Pts',(6.20267777368547,2.7053793515565,106.827819945381));
#34982=CARTESIAN_POINT('Ctrl Pts',(6.13345752769562,2.86408200486213,106.835959286236));
#34983=CARTESIAN_POINT('Ctrl Pts',(6.05820374328877,3.01998578739856,106.844098627091));
#34984=CARTESIAN_POINT('Ctrl Pts',(5.97719174312741,3.17261215182214,106.852237967947));
#34985=CARTESIAN_POINT('Ctrl Pts',(5.8950680329613,3.32733297454797,106.860489003201));
#34986=CARTESIAN_POINT('Ctrl Pts',(5.80702712091954,3.47868543698048,106.868740038455));
#34987=CARTESIAN_POINT('Ctrl Pts',(5.71340025635927,3.62620276744611,106.876991073709));
#34988=CARTESIAN_POINT('Ctrl Pts',(5.61977339179908,3.77372009791163,106.885242108963));
#34989=CARTESIAN_POINT('Ctrl Pts',(5.52056084802858,3.91740201862809,106.893493144217));
#34990=CARTESIAN_POINT('Ctrl Pts',(5.41613476850117,4.05681810899045,106.901744179471));
#34991=CARTESIAN_POINT('Ctrl Pts',(5.31194522147646,4.19591841198514,106.909976525543));
#34992=CARTESIAN_POINT('Ctrl Pts',(5.20224058843683,4.33120657113159,106.918208871615));
#34993=CARTESIAN_POINT('Ctrl Pts',(5.08732837871471,4.46221682206545,106.926441217687));
#34994=CARTESIAN_POINT('Ctrl Pts',(4.97254920912488,4.59307539528678,106.934664032723));
#34995=CARTESIAN_POINT('Ctrl Pts',(4.85257470073578,4.71966565437131,106.942886847759));
#34996=CARTESIAN_POINT('Ctrl Pts',(4.72775504148645,4.84155153516923,106.951109662795));
#34997=CARTESIAN_POINT('Ctrl Pts',(4.60308733443707,4.96328903527262,106.95932246759));
#34998=CARTESIAN_POINT('Ctrl Pts',(4.47358648596615,5.08033332166435,106.967535272385));
#34999=CARTESIAN_POINT('Ctrl Pts',(4.33964202266184,5.19228236088404,106.97574807718));
#35000=CARTESIAN_POINT('Ctrl Pts',(4.20579201884946,5.30415245208969,106.983955090192));
#35001=CARTESIAN_POINT('Ctrl Pts',(4.06750491228971,5.41093422083757,106.992162103203));
#35002=CARTESIAN_POINT('Ctrl Pts',(3.92520649450804,5.5122629632005,107.000369116215));
#35003=CARTESIAN_POINT('Ctrl Pts',(3.78299019264822,5.61353323194707,107.008571393218));
#35004=CARTESIAN_POINT('Ctrl Pts',(3.63676748146777,5.70935653508362,107.016773670221));
#35005=CARTESIAN_POINT('Ctrl Pts',(3.48699657130324,5.79940892778906,107.024975947225));
#35006=CARTESIAN_POINT('Ctrl Pts',(3.36016850770618,5.87566653066111,107.031921748037));
#35007=CARTESIAN_POINT('Ctrl Pts',(3.23079671185624,5.94778646687896,107.038867548849));
#35008=CARTESIAN_POINT('Ctrl Pts',(3.0991757505325,6.01559628526643,107.045813349661));
#35009=CARTESIAN_POINT('Ctrl Pts',(3.09917575053258,6.0155962852664,105.045751582742));
#35010=CARTESIAN_POINT('Ctrl Pts',(2.93382384459258,6.10078395293763,105.054501030655));
#35011=CARTESIAN_POINT('Ctrl Pts',(2.76495772122971,6.17915010267055,105.063250478567));
#35012=CARTESIAN_POINT('Ctrl Pts',(2.59315093316692,6.25042856433186,105.07199992648));
#35013=CARTESIAN_POINT('Ctrl Pts',(2.42134553245602,6.32170645041457,105.08074930374));
#35014=CARTESIAN_POINT('Ctrl Pts',(2.24659977927579,6.38589665313461,105.089498681));
#35015=CARTESIAN_POINT('Ctrl Pts',(2.06950718689912,6.44278115439077,105.09824805826));
#35016=CARTESIAN_POINT('Ctrl Pts',(1.89241596572847,6.49966521519728,105.106997367774));
#35017=CARTESIAN_POINT('Ctrl Pts',(1.71297821457175,6.54924360009552,105.115746677289));
#35018=CARTESIAN_POINT('Ctrl Pts',(1.53180337335814,6.59134792173563,105.124495986804));
#35019=CARTESIAN_POINT('Ctrl Pts',(1.35062987477751,6.63345193135311,105.13324523148));
#35020=CARTESIAN_POINT('Ctrl Pts',(1.16771959102919,6.66808192368244,105.141994476156));
#35021=CARTESIAN_POINT('Ctrl Pts',(0.983693746906509,6.69512028363173,105.150743720832));
#35022=CARTESIAN_POINT('Ctrl Pts',(0.799669205419644,6.72215845218869,105.159492903576));
#35023=CARTESIAN_POINT('Ctrl Pts',(0.614529402873359,6.7416050542458,105.16824208632));
#35024=CARTESIAN_POINT('Ctrl Pts',(0.428903127363242,6.75339404354122,105.176991269065));
#35025=CARTESIAN_POINT('Ctrl Pts',(0.243278104163879,6.7651829533033,105.185740392783));
#35026=CARTESIAN_POINT('Ctrl Pts',(0.0571669005391235,6.76931433552276,
105.194489516502));
#35027=CARTESIAN_POINT('Ctrl Pts',(-0.128798404777501,6.76577415902473,
105.20323864022));
#35028=CARTESIAN_POINT('Ctrl Pts',(-0.314762517259193,6.76223400523441,
105.21198770782));
#35029=CARTESIAN_POINT('Ctrl Pts',(-0.500580446819713,6.75102239665088,
105.220736775419));
#35030=CARTESIAN_POINT('Ctrl Pts',(-0.68562111884292,6.73217741012494,105.229485843018));
#35031=CARTESIAN_POINT('Ctrl Pts',(-0.870660665414765,6.71333253821768,
105.238234857404));
#35032=CARTESIAN_POINT('Ctrl Pts',(-1.05492267885511,6.68685441030608,105.24698387179));
#35033=CARTESIAN_POINT('Ctrl Pts',(-1.23778137635273,6.65283295028173,105.255732886175));
#35034=CARTESIAN_POINT('Ctrl Pts',(-1.42999922978854,6.61707018861863,105.264929696543));
#35035=CARTESIAN_POINT('Ctrl Pts',(-1.62066601233689,6.57297172934414,105.27412650691));
#35036=CARTESIAN_POINT('Ctrl Pts',(-1.80906628500366,6.520703043113,105.283323317277));
#35037=CARTESIAN_POINT('Ctrl Pts',(-1.9883134254551,6.47097374915036,105.292073315015));
#35038=CARTESIAN_POINT('Ctrl Pts',(-2.16550875896686,6.41384933989534,105.300823312753));
#35039=CARTESIAN_POINT('Ctrl Pts',(-2.34005036713997,6.34952386240481,105.309573310491));
#35040=CARTESIAN_POINT('Ctrl Pts',(-2.51458843547075,6.28519968948602,105.318323130772));
#35041=CARTESIAN_POINT('Ctrl Pts',(-2.68647261718042,6.21367483971105,105.327072951053));
#35042=CARTESIAN_POINT('Ctrl Pts',(-2.85511905908718,6.1351922674385,105.335822771333));
#35043=CARTESIAN_POINT('Ctrl Pts',(-3.02376230488877,6.05671118252941,105.344572425792));
#35044=CARTESIAN_POINT('Ctrl Pts',(-3.18916767379903,5.97127275992634,105.35332208025));
#35045=CARTESIAN_POINT('Ctrl Pts',(-3.35077334102792,5.87916720437994,105.362071734709));
#35046=CARTESIAN_POINT('Ctrl Pts',(-3.5123761603736,5.78706327195647,105.370821234977));
#35047=CARTESIAN_POINT('Ctrl Pts',(-3.67017916302279,5.68829258362311,105.379570735246));
#35048=CARTESIAN_POINT('Ctrl Pts',(-3.8236463656643,5.58319061741064,105.388320235514));
#35049=CARTESIAN_POINT('Ctrl Pts',(-3.97711106778763,5.47809036367727,105.397069593223));
#35050=CARTESIAN_POINT('Ctrl Pts',(-4.12623987481889,5.36665920043254,105.405818950931));
#35051=CARTESIAN_POINT('Ctrl Pts',(-4.27052628213889,5.24927559512368,105.41456830864));
#35052=CARTESIAN_POINT('Ctrl Pts',(-4.41481053024935,5.13189374643073,105.423317535416));
#35053=CARTESIAN_POINT('Ctrl Pts',(-4.55425230136485,5.00855981477394,105.432066762193));
#35054=CARTESIAN_POINT('Ctrl Pts',(-4.68837800630502,4.87969268192121,105.440815988969));
#35055=CARTESIAN_POINT('Ctrl Pts',(-4.82250188228837,4.75082730631867,105.44956509644));
#35056=CARTESIAN_POINT('Ctrl Pts',(-4.95130963052899,4.61642907903597,105.458314203911));
#35057=CARTESIAN_POINT('Ctrl Pts',(-5.07436379033292,4.47695444731775,105.467063311382));
#35058=CARTESIAN_POINT('Ctrl Pts',(-5.19741643562715,4.33748153220693,105.475812311171));
#35059=CARTESIAN_POINT('Ctrl Pts',(-5.31471544462669,4.19293255254719,105.484561310961));
#35060=CARTESIAN_POINT('Ctrl Pts',(-5.42586245275512,4.04379841779758,105.493310310751));
#35061=CARTESIAN_POINT('Ctrl Pts',(-5.53702160019036,3.89464799484509,105.502060266093));
#35062=CARTESIAN_POINT('Ctrl Pts',(-5.64202723081133,3.74091164444028,105.510810221435));
#35063=CARTESIAN_POINT('Ctrl Pts',(-5.74052265232849,3.58311159163422,105.519560176777));
#35064=CARTESIAN_POINT('Ctrl Pts',(-5.83901427066812,3.42531763191965,105.52830979426));
#35065=CARTESIAN_POINT('Ctrl Pts',(-5.93099603115644,3.26346052695786,105.537059411742));
#35066=CARTESIAN_POINT('Ctrl Pts',(-6.01615550622669,3.09809004467241,105.545809029225));
#35067=CARTESIAN_POINT('Ctrl Pts',(-6.10131214578715,2.93272506864002,105.554558355376));
#35068=CARTESIAN_POINT('Ctrl Pts',(-6.17964682328665,2.76384720417078,105.563307681527));
#35069=CARTESIAN_POINT('Ctrl Pts',(-6.25089348288484,2.59203002791787,105.572057007678));
#35070=CARTESIAN_POINT('Ctrl Pts',(-6.32213814889256,2.42021765937224,105.58080608901));
#35071=CARTESIAN_POINT('Ctrl Pts',(-6.38629508412516,2.24546640832114,105.589555170341));
#35072=CARTESIAN_POINT('Ctrl Pts',(-6.44314639819748,2.06836976660239,105.598304251673));
#35073=CARTESIAN_POINT('Ctrl Pts',(-6.50000285283646,1.89125711158465,105.607054124107));
#35074=CARTESIAN_POINT('Ctrl Pts',(-6.54955227673202,1.71179891440436,105.615803996541));
#35075=CARTESIAN_POINT('Ctrl Pts',(-6.59162635926345,1.53060476278603,105.624553868976));
#35076=CARTESIAN_POINT('Ctrl Pts',(-6.63369752055156,1.34942319164891,105.633303133898));
#35077=CARTESIAN_POINT('Ctrl Pts',(-6.66829431424215,1.16650618642923,105.642052398821));
#35078=CARTESIAN_POINT('Ctrl Pts',(-6.69529923745382,0.982474997620986,
105.650801663743));
#35079=CARTESIAN_POINT('Ctrl Pts',(-6.72230554731414,0.798434359180195,
105.659551377923));
#35080=CARTESIAN_POINT('Ctrl Pts',(-6.7417191649668,0.613279706242812,105.668301092103));
#35081=CARTESIAN_POINT('Ctrl Pts',(-6.75347414817259,0.427639953657873,
105.677050806282));
#35082=CARTESIAN_POINT('Ctrl Pts',(-6.76248837758729,0.285283364201837,
105.683760465458));
#35083=CARTESIAN_POINT('Ctrl Pts',(-6.76699999999987,0.142641701109152,
105.690470124634));
#35084=CARTESIAN_POINT('Ctrl Pts',(-6.767,6.37056316116541E-12,105.69717978381));
#35085=CARTESIAN_POINT('',(-6.767,5.80994670776325E-12,105.30282021619));
#35086=CARTESIAN_POINT('Ctrl Pts',(3.09917575053253,6.01559628526642,104.651558856765));
#35087=CARTESIAN_POINT('Ctrl Pts',(2.94526809315026,6.09488798919087,104.659684436931));
#35088=CARTESIAN_POINT('Ctrl Pts',(2.78822179244347,6.16831755058199,104.667810017098));
#35089=CARTESIAN_POINT('Ctrl Pts',(2.62852912535888,6.23563337898726,104.675935597265));
#35090=CARTESIAN_POINT('Ctrl Pts',(2.46549012587466,6.30435979901025,104.684231447567));
#35091=CARTESIAN_POINT('Ctrl Pts',(2.29969296126507,6.36671323073493,104.69252729787));
#35092=CARTESIAN_POINT('Ctrl Pts',(2.13168545729376,6.4224766337576,104.700823148173));
#35093=CARTESIAN_POINT('Ctrl Pts',(1.9671733892681,6.47707986596187,104.708946401344));
#35094=CARTESIAN_POINT('Ctrl Pts',(1.80054241571459,6.52536448150152,104.717069654515));
#35095=CARTESIAN_POINT('Ctrl Pts',(1.63232420764034,6.56717646185568,104.725192907685));
#35096=CARTESIAN_POINT('Ctrl Pts',(1.46408745371886,6.60899305192844,104.733317056435));
#35097=CARTESIAN_POINT('Ctrl Pts',(1.29426347175619,6.6443354970468,104.741441205184));
#35098=CARTESIAN_POINT('Ctrl Pts',(1.12339596380903,6.6731005168885,104.749565353933));
#35099=CARTESIAN_POINT('Ctrl Pts',(0.952477109807773,6.70187418068061,104.757691944007));
#35100=CARTESIAN_POINT('Ctrl Pts',(0.780514465980827,6.72406642256315,104.76581853408));
#35101=CARTESIAN_POINT('Ctrl Pts',(0.608058681233473,6.73962563056559,104.773945124154));
#35102=CARTESIAN_POINT('Ctrl Pts',(0.429286414833262,6.7557547205933,104.782369364185));
#35103=CARTESIAN_POINT('Ctrl Pts',(0.249984630161608,6.76475564082305,104.790793604217));
#35104=CARTESIAN_POINT('Ctrl Pts',(0.0707677718090432,6.76662995312092,
104.799217844248));
#35105=CARTESIAN_POINT('Ctrl Pts',(-0.102413384704881,6.76844114194766,
104.807358371009));
#35106=CARTESIAN_POINT('Ctrl Pts',(-0.275514882274292,6.76359801666385,
104.81549889777));
#35107=CARTESIAN_POINT('Ctrl Pts',(-0.44798701878902,6.75215496201002,104.823639424531));
#35108=CARTESIAN_POINT('Ctrl Pts',(-0.6294756419622,6.74011368812088,104.832205521198));
#35109=CARTESIAN_POINT('Ctrl Pts',(-0.81026685441072,6.72076398380431,104.840771617864));
#35110=CARTESIAN_POINT('Ctrl Pts',(-0.9897323476931,6.69423026791953,104.849337714531));
#35111=CARTESIAN_POINT('Ctrl Pts',(-1.16919784097561,6.66769655203473,104.857903811198));
#35112=CARTESIAN_POINT('Ctrl Pts',(-1.34733717515646,6.63397898833411,104.866469907865));
#35113=CARTESIAN_POINT('Ctrl Pts',(-1.52354118781109,6.5932625648493,104.875036004532));
#35114=CARTESIAN_POINT('Ctrl Pts',(-1.69289445640747,6.55412918020714,104.883269054664));
#35115=CARTESIAN_POINT('Ctrl Pts',(-1.86098657619945,6.50840943586728,104.891502104796));
#35116=CARTESIAN_POINT('Ctrl Pts',(-2.02726723581267,6.45619675618707,104.899735154928));
#35117=CARTESIAN_POINT('Ctrl Pts',(-2.19334988072036,6.40404625378242,104.907958400763));
#35118=CARTESIAN_POINT('Ctrl Pts',(-2.35762502253053,6.34541831878858,104.916181646598));
#35119=CARTESIAN_POINT('Ctrl Pts',(-2.51955236299189,6.28045737905624,104.924404892433));
#35120=CARTESIAN_POINT('Ctrl Pts',(-2.68131928298852,6.21556079574519,104.932619991546));
#35121=CARTESIAN_POINT('Ctrl Pts',(-2.84074270365649,6.14434383502938,104.94083509066));
#35122=CARTESIAN_POINT('Ctrl Pts',(-2.99729723425014,6.06700076558067,104.949050189773));
#35123=CARTESIAN_POINT('Ctrl Pts',(-3.15372799059706,5.98971884466675,104.957258793912));
#35124=CARTESIAN_POINT('Ctrl Pts',(-3.30729405495557,5.90632062001654,104.965467398051));
#35125=CARTESIAN_POINT('Ctrl Pts',(-3.4574897006659,5.81704856175271,104.97367600219));
#35126=CARTESIAN_POINT('Ctrl Pts',(-3.60759664286986,5.72782922635278,104.981879758439));
#35127=CARTESIAN_POINT('Ctrl Pts',(-3.75433682474402,5.63274315058797,104.990083514688));
#35128=CARTESIAN_POINT('Ctrl Pts',(-3.89722875597661,5.53207890612462,104.998287270937));
#35129=CARTESIAN_POINT('Ctrl Pts',(-4.04007840908963,5.43144444567306,105.006488599901));
#35130=CARTESIAN_POINT('Ctrl Pts',(-4.17908178494357,5.32523530700372,105.014689928865));
#35131=CARTESIAN_POINT('Ctrl Pts',(-4.31378584557687,5.21378371995815,105.02289125783));
#35132=CARTESIAN_POINT('Ctrl Pts',(-4.44847132923409,5.10234750315055,105.031091455752));
#35133=CARTESIAN_POINT('Ctrl Pts',(-4.57885840209157,4.98567050559777,105.039291653675));
#35134=CARTESIAN_POINT('Ctrl Pts',(-4.70452662502886,4.8641256392485,105.047491851598));
#35135=CARTESIAN_POINT('Ctrl Pts',(-4.83020029075708,4.74257550869415,105.055692404678));
#35136=CARTESIAN_POINT('Ctrl Pts',(-4.95115444180458,4.61615733837194,105.063892957758));
#35137=CARTESIAN_POINT('Ctrl Pts',(-5.06700503571259,4.48528136999936,105.072093510837));
#35138=CARTESIAN_POINT('Ctrl Pts',(-5.18288164159939,4.35437601599482,105.080295905191));
#35139=CARTESIAN_POINT('Ctrl Pts',(-5.29365217060191,4.21901113862904,105.088498299544));
#35140=CARTESIAN_POINT('Ctrl Pts',(-5.3989724215177,4.07963059500383,105.096700693897));
#35141=CARTESIAN_POINT('Ctrl Pts',(-5.50439116538272,3.94011970606813,105.104910758931));
#35142=CARTESIAN_POINT('Ctrl Pts',(-5.60434923156479,3.79658593421217,105.113120823965));
#35143=CARTESIAN_POINT('Ctrl Pts',(-5.69854484998727,3.64950347207446,105.121330888998));
#35144=CARTESIAN_POINT('Ctrl Pts',(-5.79278554876156,3.50235061887985,105.129544883224));
#35145=CARTESIAN_POINT('Ctrl Pts',(-5.88125811987639,3.35164599799604,105.137758877449));
#35146=CARTESIAN_POINT('Ctrl Pts',(-5.96370650742258,3.19788894324452,105.145972871674));
#35147=CARTESIAN_POINT('Ctrl Pts',(-6.04626729958135,3.04392226641688,105.15419806431));
#35148=CARTESIAN_POINT('Ctrl Pts',(-6.12278733745084,2.88689516110816,105.162423256945));
#35149=CARTESIAN_POINT('Ctrl Pts',(-6.1930580184258,2.72732861613922,105.17064844958));
#35150=CARTESIAN_POINT('Ctrl Pts',(-6.25625229131923,2.58383076401195,105.1780453477));
#35151=CARTESIAN_POINT('Ctrl Pts',(-6.31439306651561,2.43827960410804,105.18544224582));
#35152=CARTESIAN_POINT('Ctrl Pts',(-6.36736319722621,2.29106414458636,105.19283914394));
#35153=CARTESIAN_POINT('Ctrl Pts',(-6.43416671896371,2.10540269693046,105.202167775712));
#35154=CARTESIAN_POINT('Ctrl Pts',(-6.49288172649907,1.91671821912665,105.211496407485));
#35155=CARTESIAN_POINT('Ctrl Pts',(-6.54326425484908,1.72568302165095,105.220825039257));
#35156=CARTESIAN_POINT('Ctrl Pts',(-6.59352975588623,1.53509155609093,105.230132002711));
#35157=CARTESIAN_POINT('Ctrl Pts',(-6.63550135685087,1.34216043581957,105.239438966164));
#35158=CARTESIAN_POINT('Ctrl Pts',(-6.66898465358551,1.14757687770405,105.248745929617));
#35159=CARTESIAN_POINT('Ctrl Pts',(-6.70230957459399,0.95391369826447,105.258008871208));
#35160=CARTESIAN_POINT('Ctrl Pts',(-6.72722623341481,0.758613842922332,
105.267271812798));
#35161=CARTESIAN_POINT('Ctrl Pts',(-6.74359154643889,0.562371811880692,
105.276534754389));
#35162=CARTESIAN_POINT('Ctrl Pts',(-6.75907150336007,0.37674638680155,105.285296574989));
#35163=CARTESIAN_POINT('Ctrl Pts',(-6.76690063763709,0.190278218662405,
105.29405839559));
#35164=CARTESIAN_POINT('Ctrl Pts',(-6.7669990598182,0.00356713044430194,
105.30282021619));
#35165=CARTESIAN_POINT('Ctrl Pts',(-6.767,6.19460692657023E-12,105.30282021619));
#35166=CARTESIAN_POINT('Ctrl Pts',(-6.76700000000017,-0.186007249409504,
105.311569727996));
#35167=CARTESIAN_POINT('Ctrl Pts',(-6.75932637295472,-0.372014355521384,
105.320319239802));
#35168=CARTESIAN_POINT('Ctrl Pts',(-6.74400518266978,-0.557389537148933,
105.329068751608));
#35169=CARTESIAN_POINT('Ctrl Pts',(-6.72868405709711,-0.742763935805453,
105.337818226458));
#35170=CARTESIAN_POINT('Ctrl Pts',(-6.70571545653072,-0.927506129689267,
105.346567701309));
#35171=CARTESIAN_POINT('Ctrl Pts',(-6.67517739415743,-1.11098863924417,
105.35531717616));
#35172=CARTESIAN_POINT('Ctrl Pts',(-6.64463945823174,-1.29447038906123,
105.364066614782));
#35173=CARTESIAN_POINT('Ctrl Pts',(-6.60653217027239,-1.47669218227853,
105.372816053403));
#35174=CARTESIAN_POINT('Ctrl Pts',(-6.560984961168,-1.65703510503773,105.381565492025));
#35175=CARTESIAN_POINT('Ctrl Pts',(-6.51543793687604,-1.83737729603717,
105.390314895146));
#35176=CARTESIAN_POINT('Ctrl Pts',(-6.46245112202722,-2.01584035396792,
105.399064298266));
#35177=CARTESIAN_POINT('Ctrl Pts',(-6.40220448416317,-2.19181813637925,
105.407813701386));
#35178=CARTESIAN_POINT('Ctrl Pts',(-6.34195808575264,-2.36779521935737,
105.416563069732));
#35179=CARTESIAN_POINT('Ctrl Pts',(-6.27445201489314,-2.54128677544633,
105.425312438077));
#35180=CARTESIAN_POINT('Ctrl Pts',(-6.19991555136263,-2.71170355237658,
105.434061806422));
#35181=CARTESIAN_POINT('Ctrl Pts',(-6.12537937789112,-2.88211966612918,
105.442811140719));
#35182=CARTESIAN_POINT('Ctrl Pts',(-6.04381298133682,-3.04946076210317,
105.451560475016));
#35183=CARTESIAN_POINT('Ctrl Pts',(-5.95549339426361,-3.21315848206753,
105.460309809313));
#35184=CARTESIAN_POINT('Ctrl Pts',(-5.86717414355217,-3.37685557859539,
105.469059110289));
#35185=CARTESIAN_POINT('Ctrl Pts',(-5.77210188986295,-3.53690907467219,
105.477808411264));
#35186=CARTESIAN_POINT('Ctrl Pts',(-5.67059953467125,-3.69277536784817,
105.48655771224));
#35187=CARTESIAN_POINT('Ctrl Pts',(-5.56909755761831,-3.84864108035697,
105.495306980621));
#35188=CARTESIAN_POINT('Ctrl Pts',(-5.46116568338145,-4.00031938104177,
105.504056249001));
#35189=CARTESIAN_POINT('Ctrl Pts',(-5.347170486862,-4.14729511663109,105.512805517382));
#35190=CARTESIAN_POINT('Ctrl Pts',(-5.23317570555606,-4.29427031687933,
105.521554753895));
#35191=CARTESIAN_POINT('Ctrl Pts',(-5.11311782178896,-4.43654275987025,
105.530303990407));
#35192=CARTESIAN_POINT('Ctrl Pts',(-4.98740459172108,-4.57362924147547,
105.53905322692));
#35193=CARTESIAN_POINT('Ctrl Pts',(-4.86169180910923,-4.71071523514341,
105.547802432291));
#35194=CARTESIAN_POINT('Ctrl Pts',(-4.73032391415522,-4.84261509316435,
105.556551637662));
#35195=CARTESIAN_POINT('Ctrl Pts',(-4.59374707237382,-4.96888084331442,
105.565300843033));
#35196=CARTESIAN_POINT('Ctrl Pts',(-4.45717070537499,-5.09514615452639,
105.57405001799));
#35197=CARTESIAN_POINT('Ctrl Pts',(-4.31538563819616,-5.21577720253544,
105.582799192946));
#35198=CARTESIAN_POINT('Ctrl Pts',(-4.16887341290764,-5.33036429028559,
105.591548367902));
#35199=CARTESIAN_POINT('Ctrl Pts',(-4.02236168477457,-5.44495098921089,
105.60029751317));
#35200=CARTESIAN_POINT('Ctrl Pts',(-3.8711230563456,-5.55349359238675,105.609046658438));
#35201=CARTESIAN_POINT('Ctrl Pts',(-3.71567117316855,-5.65562346102392,
105.617795803706));
#35202=CARTESIAN_POINT('Ctrl Pts',(-3.5602198045744,-5.75775299158683,105.626544920012));
#35203=CARTESIAN_POINT('Ctrl Pts',(-3.40055544862543,-5.85346967275262,
105.635294036318));
#35204=CARTESIAN_POINT('Ctrl Pts',(-3.23722036323576,-5.94244842803467,
105.644043152624));
#35205=CARTESIAN_POINT('Ctrl Pts',(-3.07388580496235,-6.03142689616379,
105.652792240695));
#35206=CARTESIAN_POINT('Ctrl Pts',(-2.90688079257911,-6.11366734484725,
105.661541328766));
#35207=CARTESIAN_POINT('Ctrl Pts',(-2.73677251094835,-6.18889046787205,
105.670290416837));
#35208=CARTESIAN_POINT('Ctrl Pts',(-2.56666476416852,-6.26411335438186,
105.679039477399));
#35209=CARTESIAN_POINT('Ctrl Pts',(-2.39345402972286,-6.33231884350218,
105.687788537962));
#35210=CARTESIAN_POINT('Ctrl Pts',(-2.21772856474217,-6.39327529620981,
105.696537598524));
#35211=CARTESIAN_POINT('Ctrl Pts',(-2.04200363768468,-6.45423156232019,
105.705286632304));
#35212=CARTESIAN_POINT('Ctrl Pts',(-1.86376426620312,-6.50793874251993,
105.714035666084));
#35213=CARTESIAN_POINT('Ctrl Pts',(-1.68361578194927,-6.55421443796061,
105.722784699864));
#35214=CARTESIAN_POINT('Ctrl Pts',(-1.50346783420131,-6.60048999558619,
105.731533707588));
#35215=CARTESIAN_POINT('Ctrl Pts',(-1.32141106257533,-6.63933404145438,
105.740282715312));
#35216=CARTESIAN_POINT('Ctrl Pts',(-1.13806375959355,-6.67061465526977,
105.749031723037));
#35217=CARTESIAN_POINT('Ctrl Pts',(-0.954716987422054,-6.7018951785244,
105.757780705431));
#35218=CARTESIAN_POINT('Ctrl Pts',(-0.770079973812569,-6.72561226535797,
105.766529687826));
#35219=CARTESIAN_POINT('Ctrl Pts',(-0.584779770554938,-6.74168536939761,
105.775278670221));
#35220=CARTESIAN_POINT('Ctrl Pts',(-0.391490647556358,-6.7584514394238,
105.784404850897));
#35221=CARTESIAN_POINT('Ctrl Pts',(-0.197480213106745,-6.7668997592402,
105.793531031573));
#35222=CARTESIAN_POINT('Ctrl Pts',(-0.00346532630016481,-6.76699911271707,
105.802657212249));
#35223=CARTESIAN_POINT('Ctrl Pts',(0.184486595293678,-6.7670953613978,105.811498199779));
#35224=CARTESIAN_POINT('Ctrl Pts',(0.372442378182846,-6.75935659726783,
105.820339187309));
#35225=CARTESIAN_POINT('Ctrl Pts',(0.559750217719698,-6.74380965729036,
105.829180174839));
#35226=CARTESIAN_POINT('Ctrl Pts',(0.7451299144554,-6.72842275717279,105.837930153437));
#35227=CARTESIAN_POINT('Ctrl Pts',(0.929874656311867,-6.70538772273505,
105.846680132035));
#35228=CARTESIAN_POINT('Ctrl Pts',(1.11335688289549,-6.6747828018078,105.855430110632));
#35229=CARTESIAN_POINT('Ctrl Pts',(1.29683723118632,-6.64417819418067,105.864179999657));
#35230=CARTESIAN_POINT('Ctrl Pts',(1.47905480730014,-6.60600390230125,105.872929888682));
#35231=CARTESIAN_POINT('Ctrl Pts',(1.65939064804591,-6.56038959797189,105.881679777707));
#35232=CARTESIAN_POINT('Ctrl Pts',(1.83972470264045,-6.51477574543318,105.890429580068));
#35233=CARTESIAN_POINT('Ctrl Pts',(2.01817678125625,-6.46172209820169,105.899179382429));
#35234=CARTESIAN_POINT('Ctrl Pts',(2.19414072347455,-6.40140886724091,105.90792918479));
#35235=CARTESIAN_POINT('Ctrl Pts',(2.37010298131872,-6.34109621361458,105.916678903396));
#35236=CARTESIAN_POINT('Ctrl Pts',(2.54357687926688,-6.27352420826062,105.925428622001));
#35237=CARTESIAN_POINT('Ctrl Pts',(2.71397317789747,-6.19892237325595,105.934178340607));
#35238=CARTESIAN_POINT('Ctrl Pts',(2.88436790206987,-6.12432122757065,105.942927978365));
#35239=CARTESIAN_POINT('Ctrl Pts',(3.05168482126052,-6.0426904971752,105.951677616123));
#35240=CARTESIAN_POINT('Ctrl Pts',(3.21535561997194,-5.95430745235034,105.960427253881));
#35241=CARTESIAN_POINT('Ctrl Pts',(3.3790249607508,-5.86592519481632,105.9691768137));
#35242=CARTESIAN_POINT('Ctrl Pts',(3.53904799384668,-5.77079087940359,105.977926373519));
#35243=CARTESIAN_POINT('Ctrl Pts',(3.69488118814771,-5.66922763747163,105.986675933338));
#35244=CARTESIAN_POINT('Ctrl Pts',(3.85071304610628,-5.56766526649194,105.995425418126));
#35245=CARTESIAN_POINT('Ctrl Pts',(4.00235489705771,-5.45967423580858,106.004174902913));
#35246=CARTESIAN_POINT('Ctrl Pts',(4.14929168607466,-5.34562133936475,106.012924387701));
#35247=CARTESIAN_POINT('Ctrl Pts',(4.29622726385565,-5.23156938308688,106.021673800364));
#35248=CARTESIAN_POINT('Ctrl Pts',(4.43845763091873,-5.11145583677371,106.030423213027));
#35249=CARTESIAN_POINT('Ctrl Pts',(4.57549970660766,-4.98568866204392,106.039172625691));
#35250=CARTESIAN_POINT('Ctrl Pts',(4.71254069815118,-4.85992248226334,106.047921969137));
#35251=CARTESIAN_POINT('Ctrl Pts',(4.84439326931155,-4.72850295734166,106.056671312583));
#35252=CARTESIAN_POINT('Ctrl Pts',(4.97060959434556,-4.59187644221835,106.06542065603));
#35253=CARTESIAN_POINT('Ctrl Pts',(5.09682496280384,-4.45525096256814,106.074169933166));
#35254=CARTESIAN_POINT('Ctrl Pts',(5.21740397615719,-4.31341878218472,106.082919210302));
#35255=CARTESIAN_POINT('Ctrl Pts',(5.33193710451824,-4.16686161438818,106.091668487439));
#35256=CARTESIAN_POINT('Ctrl Pts',(5.44646940289275,-4.0203055086466,106.100417701171));
#35257=CARTESIAN_POINT('Ctrl Pts',(5.55495572749559,-3.86902470980285,106.109166914904));
#35258=CARTESIAN_POINT('Ctrl Pts',(5.65702762491353,-3.71353301465938,106.117916128637));
#35259=CARTESIAN_POINT('Ctrl Pts',(5.75909881655058,-3.55804239467048,106.126665281874));
#35260=CARTESIAN_POINT('Ctrl Pts',(5.85475551250694,-3.39834117619705,106.13541443511));
#35261=CARTESIAN_POINT('Ctrl Pts',(5.94367283728014,-3.23497174692119,106.144163588346));
#35262=CARTESIAN_POINT('Ctrl Pts',(6.03258957676244,-3.071603393011,106.152912683991));
#35263=CARTESIAN_POINT('Ctrl Pts',(6.11476689685229,-2.90456712829622,106.161661779637));
#35264=CARTESIAN_POINT('Ctrl Pts',(6.18992570525216,-2.73443024476006,106.170410875282));
#35265=CARTESIAN_POINT('Ctrl Pts',(6.2650840438867,-2.564294424631,106.179159916243));
#35266=CARTESIAN_POINT('Ctrl Pts',(6.33322384283302,-2.3910582865603,106.187908957204));
#35267=CARTESIAN_POINT('Ctrl Pts',(6.39411368720031,-2.21531017132086,106.196657998166));
#35268=CARTESIAN_POINT('Ctrl Pts',(6.45500317120888,-2.0395630961952,106.205406987348));
#35269=CARTESIAN_POINT('Ctrl Pts',(6.50864269270072,-1.86130434438639,106.21415597653));
#35270=CARTESIAN_POINT('Ctrl Pts',(6.55485008446332,-1.68113930719951,106.222904965713));
#35271=CARTESIAN_POINT('Ctrl Pts',(6.60199664749401,-1.49731239211851,106.231831779242));
#35272=CARTESIAN_POINT('Ctrl Pts',(6.64140563640903,-1.31150116499686,106.240758592771));
#35273=CARTESIAN_POINT('Ctrl Pts',(6.67293772282169,-1.1243625515568,106.249685406301));
#35274=CARTESIAN_POINT('Ctrl Pts',(6.70384494949868,-0.940932395051574,
106.258435320456));
#35275=CARTESIAN_POINT('Ctrl Pts',(6.72718449348927,-0.756227260506975,
106.267185234612));
#35276=CARTESIAN_POINT('Ctrl Pts',(6.7428770737393,-0.570874564541984,106.275935148767));
#35277=CARTESIAN_POINT('Ctrl Pts',(6.75856934538668,-0.38552551363282,106.284684890851));
#35278=CARTESIAN_POINT('Ctrl Pts',(6.76661493004102,-0.199529212418625,
106.293434632935));
#35279=CARTESIAN_POINT('Ctrl Pts',(6.76698649908907,-0.0135174386008752,
106.302184375019));
#35280=CARTESIAN_POINT('Ctrl Pts',(6.7673580613239,0.172490924445438,106.310933956665));
#35281=CARTESIAN_POINT('Ctrl Pts',(6.76005588896291,0.358514472901174,106.319683538311));
#35282=CARTESIAN_POINT('Ctrl Pts',(6.74510478454585,0.543921359662087,106.328433119957));
#35283=CARTESIAN_POINT('Ctrl Pts',(6.73015393440688,0.729325093150405,106.337182552796));
#35284=CARTESIAN_POINT('Ctrl Pts',(6.70755443556897,0.914111900256396,106.345931985635));
#35285=CARTESIAN_POINT('Ctrl Pts',(6.67738304682317,1.09765415591551,106.354681418474));
#35286=CARTESIAN_POINT('Ctrl Pts',(6.6472121311186,1.28119353391271,106.363430714135));
#35287=CARTESIAN_POINT('Ctrl Pts',(6.60946960955497,1.46348811672637,106.372180009797));
#35288=CARTESIAN_POINT('Ctrl Pts',(6.5642836699119,1.64391876348192,106.380929305458));
#35289=CARTESIAN_POINT('Ctrl Pts',(6.51909837867726,1.82434682109686,106.389678475569));
#35290=CARTESIAN_POINT('Ctrl Pts',(6.4664699527193,2.00291071820416,106.39842764568));
#35291=CARTESIAN_POINT('Ctrl Pts',(6.40657713281559,2.17900400212675,106.407176815791));
#35292=CARTESIAN_POINT('Ctrl Pts',(6.3466850927907,2.35509499309632,106.415925871976));
#35293=CARTESIAN_POINT('Ctrl Pts',(6.27952894037536,2.52871516398098,106.424674928162));
#35294=CARTESIAN_POINT('Ctrl Pts',(6.20533675061456,2.69927486771398,106.433423984348));
#35295=CARTESIAN_POINT('Ctrl Pts',(6.1283211790793,2.87632521635894,106.44250598563));
#35296=CARTESIAN_POINT('Ctrl Pts',(6.04372366626097,3.05007728919961,106.451587986912));
#35297=CARTESIAN_POINT('Ctrl Pts',(5.95185378007891,3.21989527478153,106.460669988195));
#35298=CARTESIAN_POINT('Ctrl Pts',(5.86334450817396,3.38350129286708,106.469419768502));
#35299=CARTESIAN_POINT('Ctrl Pts',(5.76808562057283,3.54345567124917,106.478169548809));
#35300=CARTESIAN_POINT('Ctrl Pts',(5.66640068804514,3.69921508465264,106.486919329116));
#35301=CARTESIAN_POINT('Ctrl Pts',(5.56471941107956,3.85496889852235,106.49566879487));
#35302=CARTESIAN_POINT('Ctrl Pts',(5.4566127081515,4.00652780919587,106.504418260623));
#35303=CARTESIAN_POINT('Ctrl Pts',(5.34244776449154,4.15337704569177,106.513167726377));
#35304=CARTESIAN_POINT('Ctrl Pts',(5.22828631819636,4.300221783562,106.521916924096));
#35305=CARTESIAN_POINT('Ctrl Pts',(5.1080671784411,4.44235690972632,106.530666121816));
#35306=CARTESIAN_POINT('Ctrl Pts',(4.9821986454476,4.579299690706,106.539415319535));
#35307=CARTESIAN_POINT('Ctrl Pts',(4.85633329944058,4.71623900429968,106.548164295726));
#35308=CARTESIAN_POINT('Ctrl Pts',(4.72481904033672,4.84798602483594,106.556913271916));
#35309=CARTESIAN_POINT('Ctrl Pts',(4.58810250737212,4.97409332259113,106.565662248106));
#35310=CARTESIAN_POINT('Ctrl Pts',(4.45137708685649,5.1002088182213,106.574411793042));
#35311=CARTESIAN_POINT('Ctrl Pts',(4.3094489263605,5.22068366307934,106.583161337978));
#35312=CARTESIAN_POINT('Ctrl Pts',(4.16280009466652,5.33510865604858,106.591910882915));
#35313=CARTESIAN_POINT('Ctrl Pts',(4.01615988348784,5.44952692272895,106.600659913523));
#35314=CARTESIAN_POINT('Ctrl Pts',(3.8647997823223,5.55789587288626,106.609408944131));
#35315=CARTESIAN_POINT('Ctrl Pts',(3.70923383581072,5.65984746713875,106.618157974739));
#35316=CARTESIAN_POINT('Ctrl Pts',(3.55366577799534,5.76180044505387,106.626907124087));
#35317=CARTESIAN_POINT('Ctrl Pts',(3.39389200026823,5.85733573571069,106.635656273435));
#35318=CARTESIAN_POINT('Ctrl Pts',(3.23045513626013,5.94612887621943,106.644405422784));
#35319=CARTESIAN_POINT('Ctrl Pts',(3.18695122151561,5.96976399206697,106.646734286896));
#35320=CARTESIAN_POINT('Ctrl Pts',(3.14318791262657,5.99292165435336,106.649063151009));
#35321=CARTESIAN_POINT('Ctrl Pts',(3.09917575053261,6.01559628526638,106.651392015122));
#35322=CARTESIAN_POINT('Origin',(0.,0.,-3.69717978381041));
#35323=CARTESIAN_POINT('',(3.09917575053271,6.01559628526633,109.0454843164));
#35324=CARTESIAN_POINT('',(3.09917575053272,6.01559628526632,108.651236765584));
#35325=CARTESIAN_POINT('',(3.09917575053259,6.01559628526639,-3.69717978381041));
#35326=CARTESIAN_POINT('',(-6.76699985827658,-0.00138494936151985,107.697179783846));
#35327=CARTESIAN_POINT('Ctrl Pts',(-6.76699985827658,-0.00138494936171985,
107.697179783846));
#35328=CARTESIAN_POINT('Ctrl Pts',(-6.76696181981259,-0.187244654813968,
107.70587655106));
#35329=CARTESIAN_POINT('Ctrl Pts',(-6.75926240779375,-0.372917032884847,
107.714573318273));
#35330=CARTESIAN_POINT('Ctrl Pts',(-6.74397327179888,-0.557775500772766,
107.723270085487));
#35331=CARTESIAN_POINT('Ctrl Pts',(-6.72865813208867,-0.742948375372715,
107.731981644135));
#35332=CARTESIAN_POINT('Ctrl Pts',(-6.70572750687344,-0.927304289991112,
107.740693202783));
#35333=CARTESIAN_POINT('Ctrl Pts',(-6.6753044046526,-1.11022524976944,107.749404761432));
#35334=CARTESIAN_POINT('Ctrl Pts',(-6.64415517569663,-1.29751209565452,
107.758324244163));
#35335=CARTESIAN_POINT('Ctrl Pts',(-6.60515146150567,-1.48329431660274,
107.767243726895));
#35336=CARTESIAN_POINT('Ctrl Pts',(-6.55847902962916,-1.66692585855356,
107.776163209626));
#35337=CARTESIAN_POINT('Ctrl Pts',(-6.51269760225618,-1.84705176507271,
107.784912414124));
#35338=CARTESIAN_POINT('Ctrl Pts',(-6.45953776308255,-2.0251081253126,107.793661618621));
#35339=CARTESIAN_POINT('Ctrl Pts',(-6.39922373482964,-2.20050553091626,
107.802410823119));
#35340=CARTESIAN_POINT('Ctrl Pts',(-6.33714894657369,-2.38102334955431,
107.811415444968));
#35341=CARTESIAN_POINT('Ctrl Pts',(-6.26749609692,-2.55872430725835,107.820420066816));
#35342=CARTESIAN_POINT('Ctrl Pts',(-6.19056070292071,-2.73299234968812,
107.829424688665));
#35343=CARTESIAN_POINT('Ctrl Pts',(-6.11362530892143,-2.9072603921179,107.838429310514));
#35344=CARTESIAN_POINT('Ctrl Pts',(-6.02940757291204,-3.07809525843261,
107.847433932363));
#35345=CARTESIAN_POINT('Ctrl Pts',(-5.93825196960901,-3.24491179316706,
107.856438554211));
#35346=CARTESIAN_POINT('Ctrl Pts',(-5.85570847447816,-3.3959680017122,107.864592446378));
#35347=CARTESIAN_POINT('Ctrl Pts',(-5.76726219193837,-3.54412000438498,
107.872746338545));
#35348=CARTESIAN_POINT('Ctrl Pts',(-5.67314178603937,-3.68886856305481,
107.880900230712));
#35349=CARTESIAN_POINT('Ctrl Pts',(-5.57913623333142,-3.83344048804244,
107.889044172852));
#35350=CARTESIAN_POINT('Ctrl Pts',(-5.47947053682363,-3.97461693282893,
107.897188114992));
#35351=CARTESIAN_POINT('Ctrl Pts',(-5.37442007181827,-4.11192143548937,
107.905332057132));
#35352=CARTESIAN_POINT('Ctrl Pts',(-5.26947568670199,-4.24908728815513,
107.913467775525));
#35353=CARTESIAN_POINT('Ctrl Pts',(-5.15915757866682,-4.38238869428596,
107.921603493918));
#35354=CARTESIAN_POINT('Ctrl Pts',(-5.04378540357022,-4.51137648647639,
107.929739212311));
#35355=CARTESIAN_POINT('Ctrl Pts',(-4.92850546265413,-4.64026115949359,
107.937868426611));
#35356=CARTESIAN_POINT('Ctrl Pts',(-4.80817974230355,-4.76483881366017,
107.945997640911));
#35357=CARTESIAN_POINT('Ctrl Pts',(-4.68316930535853,-4.88469182828842,
107.954126855212));
#35358=CARTESIAN_POINT('Ctrl Pts',(-4.55823252289801,-5.00447422711672,
107.962251279887));
#35359=CARTESIAN_POINT('Ctrl Pts',(-4.42861678389364,-5.11953727760574,
107.970375704562));
#35360=CARTESIAN_POINT('Ctrl Pts',(-4.2947212710546,-5.22949884825986,107.978500129238));
#35361=CARTESIAN_POINT('Ctrl Pts',(-4.16001292673718,-5.34012795604158,
107.986673874372));
#35362=CARTESIAN_POINT('Ctrl Pts',(-4.02097292685055,-5.44559316305205,
107.994847619506));
#35363=CARTESIAN_POINT('Ctrl Pts',(-3.8780434613653,-5.54554487059313,108.00302136464));
#35364=CARTESIAN_POINT('Ctrl Pts',(-3.73602927435292,-5.64485651664706,
108.011142767503));
#35365=CARTESIAN_POINT('Ctrl Pts',(-3.59017560674146,-5.73872487720309,
108.019264170365));
#35366=CARTESIAN_POINT('Ctrl Pts',(-3.44094696811195,-5.82684931696721,
108.027385573227));
#35367=CARTESIAN_POINT('Ctrl Pts',(-3.2917067919097,-5.91498057004909,108.035507603993));
#35368=CARTESIAN_POINT('Ctrl Pts',(-3.13909144005077,-5.99736683160999,
108.043629634759));
#35369=CARTESIAN_POINT('Ctrl Pts',(-2.98359159460155,-6.07375256300609,
108.051751665526));
#35370=CARTESIAN_POINT('Ctrl Pts',(-2.82805011596196,-6.15015874575175,
108.059875870867));
#35371=CARTESIAN_POINT('Ctrl Pts',(-2.66962293432441,-6.2205610380697,108.068000076208));
#35372=CARTESIAN_POINT('Ctrl Pts',(-2.50882230458387,-6.2847513589658,108.076124281549));
#35373=CARTESIAN_POINT('Ctrl Pts',(-2.34628111929146,-6.34963649566948,
108.084336425791));
#35374=CARTESIAN_POINT('Ctrl Pts',(-2.18131515985527,-6.40817425168384,
108.092548570034));
#35375=CARTESIAN_POINT('Ctrl Pts',(-2.01447012225202,-6.46020116765368,
108.100760714276));
#35376=CARTESIAN_POINT('Ctrl Pts',(-1.84914819595518,-6.51175313522176,
108.108897890693));
#35377=CARTESIAN_POINT('Ctrl Pts',(-1.68198172595676,-6.55691260718002,
108.117035067109));
#35378=CARTESIAN_POINT('Ctrl Pts',(-1.51351238068621,-6.59557194438129,
108.125172243526));
#35379=CARTESIAN_POINT('Ctrl Pts',(-1.34271487268815,-6.63476553443312,
108.133421871681));
#35380=CARTESIAN_POINT('Ctrl Pts',(-1.17057860116143,-6.66727794398844,
108.141671499836));
#35381=CARTESIAN_POINT('Ctrl Pts',(-0.997673498291688,-6.69305136621604,
108.149921127992));
#35382=CARTESIAN_POINT('Ctrl Pts',(-0.824768395421815,-6.71882478844367,
108.158170756147));
#35383=CARTESIAN_POINT('Ctrl Pts',(-0.651094850587449,-6.73785924430758,
108.166420384303));
#35384=CARTESIAN_POINT('Ctrl Pts',(-0.477222493360277,-6.75015167917218,
108.174670012458));
#35385=CARTESIAN_POINT('Ctrl Pts',(-0.303871997551408,-6.76240721945736,
108.182894880136));
#35386=CARTESIAN_POINT('Ctrl Pts',(-0.129805729764351,-6.76799795827916,
108.191119747813));
#35387=CARTESIAN_POINT('Ctrl Pts',(0.0444228056201317,-6.76685418893749,
108.199344615491));
#35388=CARTESIAN_POINT('Ctrl Pts',(0.21845505305805,-6.76571170818,108.207560216935));
#35389=CARTESIAN_POINT('Ctrl Pts',(0.392648848574959,-6.75784982959583,
108.215775818378));
#35390=CARTESIAN_POINT('Ctrl Pts',(0.566445567877577,-6.74325058251819,
108.223991419822));
#35391=CARTESIAN_POINT('Ctrl Pts',(0.740081404970989,-6.7286648498448,108.23219941615));
#35392=CARTESIAN_POINT('Ctrl Pts',(0.913320542615075,-6.70735419908896,
108.240407412478));
#35393=CARTESIAN_POINT('Ctrl Pts',(1.08560426551689,-6.67935269159307,108.248615408806));
#35394=CARTESIAN_POINT('Ctrl Pts',(1.25776311085951,-6.65137148061649,108.256817455677));
#35395=CARTESIAN_POINT('Ctrl Pts',(1.42896756813976,-6.61670913006465,108.265019502549));
#35396=CARTESIAN_POINT('Ctrl Pts',(1.59866386525474,-6.57545153171467,108.27322154942));
#35397=CARTESIAN_POINT('Ctrl Pts',(1.76827123680715,-6.53421555348962,108.281419298192));
#35398=CARTESIAN_POINT('Ctrl Pts',(1.93637167484358,-6.48639129711199,108.289617046963));
#35399=CARTESIAN_POINT('Ctrl Pts',(2.10242134051472,-6.43211578774421,108.297814795735));
#35400=CARTESIAN_POINT('Ctrl Pts',(2.26843933554701,-6.3778506303398,108.306010980951));
#35401=CARTESIAN_POINT('Ctrl Pts',(2.43240699471959,-6.31713677628173,108.314207166166));
#35402=CARTESIAN_POINT('Ctrl Pts',(2.59379510021734,-6.25016127616628,108.322403351382));
#35403=CARTESIAN_POINT('Ctrl Pts',(2.75517126658728,-6.18319073074718,108.330598930262));
#35404=CARTESIAN_POINT('Ctrl Pts',(2.91396792756327,-6.10995959850189,108.338794509143));
#35405=CARTESIAN_POINT('Ctrl Pts',(3.06967538907312,-6.03070327621239,108.346990088023));
#35406=CARTESIAN_POINT('Ctrl Pts',(3.22539966082515,-5.95143839737743,108.355186551701));
#35407=CARTESIAN_POINT('Ctrl Pts',(3.37803374880273,-5.86614719534679,108.36338301538));
#35408=CARTESIAN_POINT('Ctrl Pts',(3.52709209003971,-5.77511128796488,108.371579479058));
#35409=CARTESIAN_POINT('Ctrl Pts',(3.67619364319029,-5.6840489893342,108.379778318886));
#35410=CARTESIAN_POINT('Ctrl Pts',(3.82171707865581,-5.5872388550992,108.387977158714));
#35411=CARTESIAN_POINT('Ctrl Pts',(3.96320533657081,-5.48500614951129,108.396175998542));
#35412=CARTESIAN_POINT('Ctrl Pts',(4.10484138299643,-5.38266665895396,108.404383402291));
#35413=CARTESIAN_POINT('Ctrl Pts',(4.24243353989542,-5.27489349148692,108.41259080604));
#35414=CARTESIAN_POINT('Ctrl Pts',(4.37555662367105,-5.16205319936248,108.420798209789));
#35415=CARTESIAN_POINT('Ctrl Pts',(4.50875101521519,-5.0491524640061,108.429010009858));
#35416=CARTESIAN_POINT('Ctrl Pts',(4.63747129710633,-4.93117943534259,108.437221809927));
#35417=CARTESIAN_POINT('Ctrl Pts',(4.76132887346901,-4.80853786079202,108.445433609996));
#35418=CARTESIAN_POINT('Ctrl Pts',(4.88536878549057,-4.68571574070716,108.453657498983));
#35419=CARTESIAN_POINT('Ctrl Pts',(5.00453144074282,-4.55821160189771,108.461881387969));
#35420=CARTESIAN_POINT('Ctrl Pts',(5.11846744566802,-4.42646360062259,108.470105276955));
#35421=CARTESIAN_POINT('Ctrl Pts',(5.22374234451304,-4.30473072508094,108.477704008205));
#35422=CARTESIAN_POINT('Ctrl Pts',(5.32455534103403,-4.17937520772323,108.485302739455));
#35423=CARTESIAN_POINT('Ctrl Pts',(5.42066408803459,-4.05076410627577,108.492901470705));
#35424=CARTESIAN_POINT('Ctrl Pts',(5.52469196327979,-3.9115557612076,108.501126319027));
#35425=CARTESIAN_POINT('Ctrl Pts',(5.62349986955515,-3.76814214549343,108.509351167349));
#35426=CARTESIAN_POINT('Ctrl Pts',(5.71672993877672,-3.6209512295934,108.517576015671));
#35427=CARTESIAN_POINT('Ctrl Pts',(5.80985501026929,-3.47392608329998,108.52579160099));
#35428=CARTESIAN_POINT('Ctrl Pts',(5.89741456331119,-3.32313240810039,108.53400718631));
#35429=CARTESIAN_POINT('Ctrl Pts',(5.97909148676538,-3.16903044997831,108.542222771629));
#35430=CARTESIAN_POINT('Ctrl Pts',(6.06069283441437,-3.01507108267719,108.550430755052));
#35431=CARTESIAN_POINT('Ctrl Pts',(6.13642222577955,-2.85780984381845,108.558638738475));
#35432=CARTESIAN_POINT('Ctrl Pts',(6.20600627425849,-2.69773518416176,108.566846721898));
#35433=CARTESIAN_POINT('Ctrl Pts',(6.27553991280148,-2.53777649006781,108.575048759075));
#35434=CARTESIAN_POINT('Ctrl Pts',(6.33893693350134,-2.37500876252847,108.583250796252));
#35435=CARTESIAN_POINT('Ctrl Pts',(6.39597022614917,-2.20994431292134,108.591452833428));
#35436=CARTESIAN_POINT('Ctrl Pts',(6.4529736540061,-2.04496629730817,108.599650575707));
#35437=CARTESIAN_POINT('Ctrl Pts',(6.50361987537532,-1.87769429379751,108.607848317987));
#35438=CARTESIAN_POINT('Ctrl Pts',(6.54773016761079,-1.70865989950009,108.616046060266));
#35439=CARTESIAN_POINT('Ctrl Pts',(6.59183207300411,-1.53965764429559,108.624242243881));
#35440=CARTESIAN_POINT('Ctrl Pts',(6.62940042803424,-1.36889401098159,108.632438427495));
#35441=CARTESIAN_POINT('Ctrl Pts',(6.66030649961352,-1.19691534003282,108.640634611109));
#35442=CARTESIAN_POINT('Ctrl Pts',(6.69121029607473,-1.02494932911375,108.64883019137));
#35443=CARTESIAN_POINT('Ctrl Pts',(6.71545272145503,-0.851768811698276,
108.657025771631));
#35444=CARTESIAN_POINT('Ctrl Pts',(6.73295626998631,-0.677929838886081,
108.665221351892));
#35445=CARTESIAN_POINT('Ctrl Pts',(6.75046171457579,-0.504072035103136,
108.673417819933));
#35446=CARTESIAN_POINT('Ctrl Pts',(6.76122679201078,-0.329555990916877,
108.681614287973));
#35447=CARTESIAN_POINT('Ctrl Pts',(6.76522592670201,-0.154942443116709,
108.689810756014));
#35448=CARTESIAN_POINT('Ctrl Pts',(6.76922622219469,0.0197217885630407,
108.698009603188));
#35449=CARTESIAN_POINT('Ctrl Pts',(6.76645665488345,0.194483221583864,108.706208450361));
#35450=CARTESIAN_POINT('Ctrl Pts',(6.75694377679353,0.368781503401733,108.714407297534));
#35451=CARTESIAN_POINT('Ctrl Pts',(6.74742095682094,0.543261943873229,108.7226147133));
#35452=CARTESIAN_POINT('Ctrl Pts',(6.73114076583603,0.717277907320158,108.730822129066));
#35453=CARTESIAN_POINT('Ctrl Pts',(6.70818172292812,0.890273537837168,108.739029544832));
#35454=CARTESIAN_POINT('Ctrl Pts',(6.68521037478073,1.06336188792753,108.747241359484));
#35455=CARTESIAN_POINT('Ctrl Pts',(6.65555309952177,1.23542846162337,108.755453174136));
#35456=CARTESIAN_POINT('Ctrl Pts',(6.61933948700453,1.4059280763192,108.763664988789));
#35457=CARTESIAN_POINT('Ctrl Pts',(6.5830725444375,1.57667877761777,108.771888896586));
#35458=CARTESIAN_POINT('Ctrl Pts',(6.54023005705052,1.74585756041812,108.780112804384));
#35459=CARTESIAN_POINT('Ctrl Pts',(6.49099175486399,1.91293362098316,108.788336712181));
#35460=CARTESIAN_POINT('Ctrl Pts',(6.44549647299097,2.06730881533578,108.795935451105));
#35461=CARTESIAN_POINT('Ctrl Pts',(6.39454143517043,2.2198888095163,108.803534190028));
#35462=CARTESIAN_POINT('Ctrl Pts',(6.33830442585919,2.37027129357249,108.811132928952));
#35463=CARTESIAN_POINT('Ctrl Pts',(6.27796846008213,2.53161473133012,108.819285518452));
#35464=CARTESIAN_POINT('Ctrl Pts',(6.21137310086153,2.6909063624389,108.827438107952));
#35465=CARTESIAN_POINT('Ctrl Pts',(6.13867664551614,2.84761971509446,108.835590697453));
#35466=CARTESIAN_POINT('Ctrl Pts',(6.06606751590959,3.00414481772821,108.843733493753));
#35467=CARTESIAN_POINT('Ctrl Pts',(5.98737203330339,3.15809747915696,108.851876290054));
#35468=CARTESIAN_POINT('Ctrl Pts',(5.90279789406262,3.3089675159859,108.860019086354));
#35469=CARTESIAN_POINT('Ctrl Pts',(5.81832523890025,3.45965651749149,108.86815211177));
#35470=CARTESIAN_POINT('Ctrl Pts',(5.72798816050227,3.60726994791767,108.876285137186));
#35471=CARTESIAN_POINT('Ctrl Pts',(5.63204177845997,3.75131902211495,108.884418162601));
#35472=CARTESIAN_POINT('Ctrl Pts',(5.53616136407185,3.89526905579284,108.892545596179));
#35473=CARTESIAN_POINT('Ctrl Pts',(5.43467952445377,4.03565930826703,108.900673029757));
#35474=CARTESIAN_POINT('Ctrl Pts',(5.32789673113761,4.17202653662859,108.908800463335));
#35475=CARTESIAN_POINT('Ctrl Pts',(5.2211670204732,4.30832597565942,108.916923856695));
#35476=CARTESIAN_POINT('Ctrl Pts',(5.10914182745673,4.44060608494335,108.925047250055));
#35477=CARTESIAN_POINT('Ctrl Pts',(4.9921642495206,4.56843355055193,108.933170643416));
#35478=CARTESIAN_POINT('Ctrl Pts',(4.87522254724616,4.69622181296454,108.941291545426));
#35479=CARTESIAN_POINT('Ctrl Pts',(4.75333173178667,4.81955988195647,108.949412447436));
#35480=CARTESIAN_POINT('Ctrl Pts',(4.62687436706289,4.93804845980843,108.957533349446));
#35481=CARTESIAN_POINT('Ctrl Pts',(4.50040460057786,5.0565486579172,108.965655047878));
#35482=CARTESIAN_POINT('Ctrl Pts',(4.36936765185437,5.17019815898645,108.973776746311));
#35483=CARTESIAN_POINT('Ctrl Pts',(4.23418226466472,5.27863519762436,108.981898444743));
#35484=CARTESIAN_POINT('Ctrl Pts',(4.0989913839812,5.38707664279038,108.990020473215));
#35485=CARTESIAN_POINT('Ctrl Pts',(3.95965201809419,5.49030497918769,108.998142501687));
#35486=CARTESIAN_POINT('Ctrl Pts',(3.81661487679756,5.58799963155042,109.006264530159));
#35487=CARTESIAN_POINT('Ctrl Pts',(3.6734965061454,5.68574976372473,109.014391171049));
#35488=CARTESIAN_POINT('Ctrl Pts',(3.52667647083157,5.77795973283162,109.022517811939));
#35489=CARTESIAN_POINT('Ctrl Pts',(3.37663368089296,5.86435281894424,109.03064445283));
#35490=CARTESIAN_POINT('Ctrl Pts',(3.28530383696744,5.91693959818328,109.03559107402));
#35491=CARTESIAN_POINT('Ctrl Pts',(3.19278045746336,5.96737206540541,109.04053769521));
#35492=CARTESIAN_POINT('Ctrl Pts',(3.09917575053271,6.01559628526633,109.0454843164));
#35493=CARTESIAN_POINT('Ctrl Pts',(3.0991757505325,6.01559628526643,107.045813349661));
#35494=CARTESIAN_POINT('Ctrl Pts',(2.9438094780766,6.09563945326048,107.054012219891));
#35495=CARTESIAN_POINT('Ctrl Pts',(2.78530897263697,6.1696758601344,107.06221109012));
#35496=CARTESIAN_POINT('Ctrl Pts',(2.624181600378,6.23746422260181,107.07040996035));
#35497=CARTESIAN_POINT('Ctrl Pts',(2.46305199894301,6.30525352291231,107.07860894401));
#35498=CARTESIAN_POINT('Ctrl Pts',(2.29929578858001,6.36679446737404,107.086807927669));
#35499=CARTESIAN_POINT('Ctrl Pts',(2.13344051535257,6.4218938458567,107.095006911329));
#35500=CARTESIAN_POINT('Ctrl Pts',(1.96755286063483,6.47700398191103,107.103207495754));
#35501=CARTESIAN_POINT('Ctrl Pts',(1.79956566691533,6.52566993411948,107.111408080179));
#35502=CARTESIAN_POINT('Ctrl Pts',(1.63002189542284,6.56774829149551,107.119608664604));
#35503=CARTESIAN_POINT('Ctrl Pts',(1.45710134210579,6.61066471818628,107.12797257903));
#35504=CARTESIAN_POINT('Ctrl Pts',(1.28256193294628,6.64672828420124,107.136336493456));
#35505=CARTESIAN_POINT('Ctrl Pts',(1.10699027058011,6.67584163539257,107.144700407882));
#35506=CARTESIAN_POINT('Ctrl Pts',(0.934608297546703,6.70442607124254,107.152912371315));
#35507=CARTESIAN_POINT('Ctrl Pts',(0.761231620545215,6.72631067366722,107.161124334747));
#35508=CARTESIAN_POINT('Ctrl Pts',(0.587419989921386,6.74145583353038,107.169336298179));
#35509=CARTESIAN_POINT('Ctrl Pts',(0.408784144552109,6.75702135366099,107.177776188102));
#35510=CARTESIAN_POINT('Ctrl Pts',(0.229689264636626,6.76546789067559,107.186216078025));
#35511=CARTESIAN_POINT('Ctrl Pts',(0.0507419610713189,6.76680975448451,
107.194655967949));
#35512=CARTESIAN_POINT('Ctrl Pts',(-0.128205342493988,6.76815161829342,
107.203095857872));
#35513=CARTESIAN_POINT('Ctrl Pts',(-0.307004666234908,6.76238887731013,
107.211535747795));
#35514=CARTESIAN_POINT('Ctrl Pts',(-0.485056527264841,6.74959325925332,
107.219975637718));
#35515=CARTESIAN_POINT('Ctrl Pts',(-0.667450634673003,6.73648558758559,
107.228621355771));
#35516=CARTESIAN_POINT('Ctrl Pts',(-0.849476241434182,6.71596863773433,
107.237267073823));
#35517=CARTESIAN_POINT('Ctrl Pts',(-1.03052163609518,6.6880725293271,107.245912791875));
#35518=CARTESIAN_POINT('Ctrl Pts',(-1.2113346053658,6.66021223383793,107.254547410588));
#35519=CARTESIAN_POINT('Ctrl Pts',(-1.39116957185494,6.62499171633672,107.2631820293));
#35520=CARTESIAN_POINT('Ctrl Pts',(-1.56941903346027,6.58249290902867,107.271816648013));
#35521=CARTESIAN_POINT('Ctrl Pts',(-1.7539635736031,6.53849320894178,107.280756207915));
#35522=CARTESIAN_POINT('Ctrl Pts',(-1.93680825493122,6.48669174887171,107.289695767817));
#35523=CARTESIAN_POINT('Ctrl Pts',(-2.11728625709747,6.42723796863833,107.29863532772));
#35524=CARTESIAN_POINT('Ctrl Pts',(-2.29112406528735,6.36997162747587,107.30724598099));
#35525=CARTESIAN_POINT('Ctrl Pts',(-2.46276589402842,6.30560607927925,107.315856634261));
#35526=CARTESIAN_POINT('Ctrl Pts',(-2.63162710199824,6.23432657117257,107.324467287531));
#35527=CARTESIAN_POINT('Ctrl Pts',(-2.80032847153802,6.16311453388887,107.333069790242));
#35528=CARTESIAN_POINT('Ctrl Pts',(-2.96625418783669,6.08500170293773,107.341672292954));
#35529=CARTESIAN_POINT('Ctrl Pts',(-3.12883680410529,6.00022243364996,107.350274795665));
#35530=CARTESIAN_POINT('Ctrl Pts',(-3.29123643690934,5.91553858172459,107.358867616432));
#35531=CARTESIAN_POINT('Ctrl Pts',(-3.45030020608423,5.82420340032712,107.3674604372));
#35532=CARTESIAN_POINT('Ctrl Pts',(-3.60548242248394,5.72649853760213,107.376053257967));
#35533=CARTESIAN_POINT('Ctrl Pts',(-3.62377135156097,5.7149835757314,107.377065960925));
#35534=CARTESIAN_POINT('Ctrl Pts',(-3.64200639260673,5.70338019469417,107.378078663883));
#35535=CARTESIAN_POINT('Ctrl Pts',(-3.66018667337285,5.69168889839069,107.379091366841));
#35536=CARTESIAN_POINT('Ctrl Pts',(-3.81449075443639,5.59245969749119,107.387686624601));
#35537=CARTESIAN_POINT('Ctrl Pts',(-3.9646663544448,5.48701045969764,107.396281882361));
#35538=CARTESIAN_POINT('Ctrl Pts',(-4.11022643393577,5.37571647892406,107.404877140121));
#35539=CARTESIAN_POINT('Ctrl Pts',(-4.25592282426801,5.26431827605744,107.413480446976));
#35540=CARTESIAN_POINT('Ctrl Pts',(-4.3969948241579,5.14706459065193,107.42208375383));
#35541=CARTESIAN_POINT('Ctrl Pts',(-4.53298929980819,5.02437030958353,107.430687060684));
#35542=CARTESIAN_POINT('Ctrl Pts',(-4.67462215357932,4.89658908107391,107.439647063624));
#35543=CARTESIAN_POINT('Ctrl Pts',(-4.81074720568499,4.7629067710744,107.448607066565));
#35544=CARTESIAN_POINT('Ctrl Pts',(-4.9408968752471,4.6238325086635,107.457567069505));
#35545=CARTESIAN_POINT('Ctrl Pts',(-5.06620719043081,4.48992944371309,107.466193912709));
#35546=CARTESIAN_POINT('Ctrl Pts',(-5.18597831737321,4.3510284281807,107.474820755914));
#35547=CARTESIAN_POINT('Ctrl Pts',(-5.29983536026046,4.20761620803667,107.483447599119));
#35548=CARTESIAN_POINT('Ctrl Pts',(-5.41380122169928,4.06406692206274,107.492082687405));
#35549=CARTESIAN_POINT('Ctrl Pts',(-5.52184153431556,3.9159980696293,107.500717775691));
#35550=CARTESIAN_POINT('Ctrl Pts',(-5.62362453945761,3.76392561552565,107.509352863977));
#35551=CARTESIAN_POINT('Ctrl Pts',(-5.72555871278871,3.61162730330887,107.518000777102));
#35552=CARTESIAN_POINT('Ctrl Pts',(-5.82121684441455,3.45531376477537,107.526648690227));
#35553=CARTESIAN_POINT('Ctrl Pts',(-5.91031219195361,3.29552708889558,107.535296603353));
#35554=CARTESIAN_POINT('Ctrl Pts',(-5.92030733363478,3.27760145631995,107.536266767557));
#35555=CARTESIAN_POINT('Ctrl Pts',(-5.93021992915776,3.25963213489651,107.537236931761));
#35556=CARTESIAN_POINT('Ctrl Pts',(-5.94004961119222,3.24161990624674,107.538207095965));
#35557=CARTESIAN_POINT('Ctrl Pts',(-6.02650562242684,3.08319510297793,107.546740080759));
#35558=CARTESIAN_POINT('Ctrl Pts',(-6.10671679174137,2.9211319740975,107.555273065552));
#35559=CARTESIAN_POINT('Ctrl Pts',(-6.18037722501124,2.75594382318696,107.563806050346));
#35560=CARTESIAN_POINT('Ctrl Pts',(-6.25393679587604,2.59098186255866,107.572327351019));
#35561=CARTESIAN_POINT('Ctrl Pts',(-6.32096338049466,2.42290369930237,107.580848651693));
#35562=CARTESIAN_POINT('Ctrl Pts',(-6.38119643998813,2.25224798685288,107.589369952366));
#35563=CARTESIAN_POINT('Ctrl Pts',(-6.44135375726403,2.08180687154008,107.597880537625));
#35564=CARTESIAN_POINT('Ctrl Pts',(-6.49473447280367,1.90879496828615,107.606391122883));
#35565=CARTESIAN_POINT('Ctrl Pts',(-6.54112551533562,1.73377218590718,107.614901708142));
#35566=CARTESIAN_POINT('Ctrl Pts',(-6.58744621359749,1.55901479635409,107.623399388519));
#35567=CARTESIAN_POINT('Ctrl Pts',(-6.62679829947891,1.38225291815665,107.631897068896));
#35568=CARTESIAN_POINT('Ctrl Pts',(-6.6590180784668,1.20406280178914,107.640394749274));
#35569=CARTESIAN_POINT('Ctrl Pts',(-6.69120843705091,1.02603539371257,107.648884670281));
#35570=CARTESIAN_POINT('Ctrl Pts',(-6.71627941206488,0.84658266026334,107.657374591288));
#35571=CARTESIAN_POINT('Ctrl Pts',(-6.73411774491939,0.666293627135781,
107.665864512295));
#35572=CARTESIAN_POINT('Ctrl Pts',(-6.7519376287008,0.486191055690526,107.674345652707));
#35573=CARTESIAN_POINT('Ctrl Pts',(-6.76253975861578,0.305254227259429,
107.68282679312));
#35574=CARTESIAN_POINT('Ctrl Pts',(-6.76586233578067,0.124080027661641,
107.691307933532));
#35575=CARTESIAN_POINT('Ctrl Pts',(-6.7666291224273,0.0822685210896604,
107.693265216958));
#35576=CARTESIAN_POINT('Ctrl Pts',(-6.76700841916055,0.0404444015700853,
107.695222500384));
#35577=CARTESIAN_POINT('Ctrl Pts',(-6.76699985827674,-0.00138494859027308,
107.69717978381));
#35578=CARTESIAN_POINT('',(-6.76721124277169,-0.000653705868658438,107.303185781308));
#35579=CARTESIAN_POINT('Ctrl Pts',(3.09917575053261,6.01559628526638,106.651392015122));
#35580=CARTESIAN_POINT('Ctrl Pts',(2.9338238445927,6.10078395293757,106.660141463035));
#35581=CARTESIAN_POINT('Ctrl Pts',(2.76495772122992,6.17915010267045,106.668890910947));
#35582=CARTESIAN_POINT('Ctrl Pts',(2.59315093316722,6.25042856433173,106.67764035886));
#35583=CARTESIAN_POINT('Ctrl Pts',(2.4213455324563,6.32170645041446,106.68638973612));
#35584=CARTESIAN_POINT('Ctrl Pts',(2.24659977927605,6.38589665313452,106.69513911338));
#35585=CARTESIAN_POINT('Ctrl Pts',(2.06950718689935,6.4427811543907,106.70388849064));
#35586=CARTESIAN_POINT('Ctrl Pts',(1.89241596572879,6.49966521519719,106.712637800154));
#35587=CARTESIAN_POINT('Ctrl Pts',(1.71297821457217,6.54924360009541,106.721387109669));
#35588=CARTESIAN_POINT('Ctrl Pts',(1.53180337335866,6.59134792173551,106.730136419184));
#35589=CARTESIAN_POINT('Ctrl Pts',(1.350629874778,6.63345193135301,106.73888566386));
#35590=CARTESIAN_POINT('Ctrl Pts',(1.16771959102965,6.66808192368236,106.747634908536));
#35591=CARTESIAN_POINT('Ctrl Pts',(0.983693746906934,6.69512028363167,106.756384153212));
#35592=CARTESIAN_POINT('Ctrl Pts',(0.799669205419912,6.72215845218867,106.765133335956));
#35593=CARTESIAN_POINT('Ctrl Pts',(0.614529402873468,6.74160505424579,106.7738825187));
#35594=CARTESIAN_POINT('Ctrl Pts',(0.428903127363191,6.75339404354122,106.782631701445));
#35595=CARTESIAN_POINT('Ctrl Pts',(0.243278104163796,6.7651829533033,106.791380825163));
#35596=CARTESIAN_POINT('Ctrl Pts',(0.0571669005390081,6.76931433552276,
106.800129948882));
#35597=CARTESIAN_POINT('Ctrl Pts',(-0.128798404777648,6.76577415902473,
106.8088790726));
#35598=CARTESIAN_POINT('Ctrl Pts',(-0.314762517259244,6.76223400523441,
106.8176281402));
#35599=CARTESIAN_POINT('Ctrl Pts',(-0.500580446819668,6.75102239665088,
106.826377207799));
#35600=CARTESIAN_POINT('Ctrl Pts',(-0.68562111884278,6.73217741012496,106.835126275398));
#35601=CARTESIAN_POINT('Ctrl Pts',(-0.870660665414785,6.71333253821768,
106.843875289784));
#35602=CARTESIAN_POINT('Ctrl Pts',(-1.05492267885529,6.68685441030606,106.85262430417));
#35603=CARTESIAN_POINT('Ctrl Pts',(-1.23778137635307,6.65283295028167,106.861373318555));
#35604=CARTESIAN_POINT('Ctrl Pts',(-1.42999922978891,6.61707018861856,106.870570128923));
#35605=CARTESIAN_POINT('Ctrl Pts',(-1.62066601233729,6.57297172934404,106.87976693929));
#35606=CARTESIAN_POINT('Ctrl Pts',(-1.80906628500408,6.52070304311288,106.888963749658));
#35607=CARTESIAN_POINT('Ctrl Pts',(-1.98831342545542,6.47097374915026,106.897713747395));
#35608=CARTESIAN_POINT('Ctrl Pts',(-2.16550875896709,6.41384933989526,106.906463745133));
#35609=CARTESIAN_POINT('Ctrl Pts',(-2.34005036714011,6.34952386240476,106.915213742871));
#35610=CARTESIAN_POINT('Ctrl Pts',(-2.51458843547092,6.28519968948595,106.923963563152));
#35611=CARTESIAN_POINT('Ctrl Pts',(-2.68647261718061,6.21367483971097,106.932713383433));
#35612=CARTESIAN_POINT('Ctrl Pts',(-2.8551190590874,6.1351922674384,106.941463203713));
#35613=CARTESIAN_POINT('Ctrl Pts',(-3.02376230488902,6.05671118252928,106.950212858172));
#35614=CARTESIAN_POINT('Ctrl Pts',(-3.18916767379931,5.97127275992619,106.95896251263));
#35615=CARTESIAN_POINT('Ctrl Pts',(-3.35077334102822,5.87916720437977,106.967712167089));
#35616=CARTESIAN_POINT('Ctrl Pts',(-3.51237616037403,5.78706327195622,106.976461667357));
#35617=CARTESIAN_POINT('Ctrl Pts',(-3.67017916302335,5.68829258362275,106.985211167626));
#35618=CARTESIAN_POINT('Ctrl Pts',(-3.82364636566498,5.58319061741018,106.993960667894));
#35619=CARTESIAN_POINT('Ctrl Pts',(-3.97711106778832,5.47809036367677,107.002710025603));
#35620=CARTESIAN_POINT('Ctrl Pts',(-4.12623987481959,5.366659200432,107.011459383311));
#35621=CARTESIAN_POINT('Ctrl Pts',(-4.2705262821396,5.2492755951231,107.02020874102));
#35622=CARTESIAN_POINT('Ctrl Pts',(-4.41481053025027,5.13189374642995,107.028957967796));
#35623=CARTESIAN_POINT('Ctrl Pts',(-4.55425230136596,5.00855981477294,107.037707194573));
#35624=CARTESIAN_POINT('Ctrl Pts',(-4.6883780063063,4.87969268191998,107.046456421349));
#35625=CARTESIAN_POINT('Ctrl Pts',(-4.82250188228965,4.75082730631738,107.05520552882));
#35626=CARTESIAN_POINT('Ctrl Pts',(-4.95130963053026,4.61642907903461,107.063954636291));
#35627=CARTESIAN_POINT('Ctrl Pts',(-5.07436379033417,4.47695444731633,107.072703743762));
#35628=CARTESIAN_POINT('Ctrl Pts',(-5.19741643562863,4.33748153220517,107.081452743551));
#35629=CARTESIAN_POINT('Ctrl Pts',(-5.31471544462838,4.19293255254507,107.090201743341));
#35630=CARTESIAN_POINT('Ctrl Pts',(-5.42586245275699,4.04379841779507,107.098950743131));
#35631=CARTESIAN_POINT('Ctrl Pts',(-5.53702160019218,3.8946479948425,107.107700698473));
#35632=CARTESIAN_POINT('Ctrl Pts',(-5.6420272308131,3.74091164443761,107.116450653815));
#35633=CARTESIAN_POINT('Ctrl Pts',(-5.7405226523302,3.58311159163148,107.125200609157));
#35634=CARTESIAN_POINT('Ctrl Pts',(-5.83901427066977,3.42531763191684,107.13395022664));
#35635=CARTESIAN_POINT('Ctrl Pts',(-5.93099603115803,3.26346052695498,107.142699844122));
#35636=CARTESIAN_POINT('Ctrl Pts',(-6.01615550622821,3.09809004466946,107.151449461605));
#35637=CARTESIAN_POINT('Ctrl Pts',(-6.10131214578867,2.93272506863688,107.160198787756));
#35638=CARTESIAN_POINT('Ctrl Pts',(-6.17964682328814,2.76384720416745,107.168948113907));
#35639=CARTESIAN_POINT('Ctrl Pts',(-6.25089348288629,2.59203002791435,107.177697440058));
#35640=CARTESIAN_POINT('Ctrl Pts',(-6.32213814889398,2.42021765936854,107.18644652139));
#35641=CARTESIAN_POINT('Ctrl Pts',(-6.38629508412653,2.24546640831725,107.195195602721));
#35642=CARTESIAN_POINT('Ctrl Pts',(-6.44314639819879,2.06836976659831,107.203944684053));
#35643=CARTESIAN_POINT('Ctrl Pts',(-6.50000285283766,1.8912571115805,107.212694556487));
#35644=CARTESIAN_POINT('Ctrl Pts',(-6.54955227673312,1.71179891440015,107.221444428922));
#35645=CARTESIAN_POINT('Ctrl Pts',(-6.59162635926444,1.53060476278177,107.230194301356));
#35646=CARTESIAN_POINT('Ctrl Pts',(-6.63369752055244,1.34942319164459,107.238943566279));
#35647=CARTESIAN_POINT('Ctrl Pts',(-6.66829431424292,1.16650618642486,107.247692831201));
#35648=CARTESIAN_POINT('Ctrl Pts',(-6.69529923745447,0.982474997616562,
107.256442096124));
#35649=CARTESIAN_POINT('Ctrl Pts',(-6.72230554731467,0.798434359175721,
107.265191810303));
#35650=CARTESIAN_POINT('Ctrl Pts',(-6.74171916496722,0.613279706238294,
107.273941524483));
#35651=CARTESIAN_POINT('Ctrl Pts',(-6.75347414817288,0.427639953653314,
107.282691238663));
#35652=CARTESIAN_POINT('Ctrl Pts',(-6.76248837758739,0.285283364198783,
107.289400897838));
#35653=CARTESIAN_POINT('Ctrl Pts',(-6.76699999999987,0.142641701107611,
107.296110557014));
#35654=CARTESIAN_POINT('Ctrl Pts',(-6.767,6.34351679601791E-12,107.30282021619));
#35655=CARTESIAN_POINT('Ctrl Pts',(-6.76699921757691,-0.00325412254306615,
107.30282021619));
#35656=CARTESIAN_POINT('Ctrl Pts',(-6.7669011553275,-0.207176118798005,
107.312373624824));
#35657=CARTESIAN_POINT('Ctrl Pts',(-6.75758045334832,-0.410786772883343,
107.321927033457));
#35658=CARTESIAN_POINT('Ctrl Pts',(-6.73915089857601,-0.613297779404236,
107.331480442091));
#35659=CARTESIAN_POINT('Ctrl Pts',(-6.721475047404,-0.80752680208984,107.340643150104));
#35660=CARTESIAN_POINT('Ctrl Pts',(-6.69542064108127,-1.00074419645186,
107.349805858117));
#35661=CARTESIAN_POINT('Ctrl Pts',(-6.66113955109404,-1.19227047302647,
107.35896856613));
#35662=CARTESIAN_POINT('Ctrl Pts',(-6.62676727658224,-1.38430619175933,
107.368155646098));
#35663=CARTESIAN_POINT('Ctrl Pts',(-6.58412459563606,-1.57464159892993,
107.377342726066));
#35664=CARTESIAN_POINT('Ctrl Pts',(-6.53341363497359,-1.76261035806021,
107.386529806034));
#35665=CARTESIAN_POINT('Ctrl Pts',(-6.48254029096963,-1.95118101853107,
107.395746304273));
#35666=CARTESIAN_POINT('Ctrl Pts',(-6.42354701191558,-2.13736966837478,
107.404962802511));
#35667=CARTESIAN_POINT('Ctrl Pts',(-6.35668567204398,-2.32052499810513,
107.414179300749));
#35668=CARTESIAN_POINT('Ctrl Pts',(-6.34874965654843,-2.34226437002954,
107.41527324043));
#35669=CARTESIAN_POINT('Ctrl Pts',(-6.34070284853216,-2.36396103460376,
107.416367180112));
#35670=CARTESIAN_POINT('Ctrl Pts',(-6.3325457126643,-2.38561392455213,107.417461119793));
#35671=CARTESIAN_POINT('Ctrl Pts',(-6.26807568330373,-2.55674782170998,
107.426107086284));
#35672=CARTESIAN_POINT('Ctrl Pts',(-6.19660697721829,-2.72541921646342,
107.434753052775));
#35673=CARTESIAN_POINT('Ctrl Pts',(-6.11834270474009,-2.8910502498839,107.443399019266));
#35674=CARTESIAN_POINT('Ctrl Pts',(-6.04017854290617,-3.05646941869561,
107.45203392639));
#35675=CARTESIAN_POINT('Ctrl Pts',(-5.95523627760394,-3.21885570674108,
107.460668833514));
#35676=CARTESIAN_POINT('Ctrl Pts',(-5.86376748714751,-3.37765004946808,
107.469303740639));
#35677=CARTESIAN_POINT('Ctrl Pts',(-5.76926200667351,-3.54171623620877,
107.47822531971));
#35678=CARTESIAN_POINT('Ctrl Pts',(-5.66778928891598,-3.70194756933119,
107.487146898782));
#35679=CARTESIAN_POINT('Ctrl Pts',(-5.55968042126128,-3.85775097867191,
107.496068477853));
#35680=CARTESIAN_POINT('Ctrl Pts',(-5.45533433771433,-4.00813157113072,
107.504679536829));
#35681=CARTESIAN_POINT('Ctrl Pts',(-5.34480643133607,-4.15438697055638,
107.513290595805));
#35682=CARTESIAN_POINT('Ctrl Pts',(-5.22844071569663,-4.29600939040474,
107.52190165478));
#35683=CARTESIAN_POINT('Ctrl Pts',(-5.11218473829912,-4.43749825377312,
107.53050459313));
#35684=CARTESIAN_POINT('Ctrl Pts',(-4.99010212077704,-4.57436261358622,
107.53910753148));
#35685=CARTESIAN_POINT('Ctrl Pts',(-4.86257905903547,-4.7061251465117,107.547710469829));
#35686=CARTESIAN_POINT('Ctrl Pts',(-4.73519879362234,-4.83774013588175,
107.556303774878));
#35687=CARTESIAN_POINT('Ctrl Pts',(-4.6023904490695,-4.9642644767047,107.564897079927));
#35688=CARTESIAN_POINT('Ctrl Pts',(-4.46457936745683,-5.08525516288797,
107.573490384975));
#35689=CARTESIAN_POINT('Ctrl Pts',(-4.4492249572258,-5.09873550574613,107.574447819816));
#35690=CARTESIAN_POINT('Ctrl Pts',(-4.43380848458944,-5.11214719161138,
107.575405254657));
#35691=CARTESIAN_POINT('Ctrl Pts',(-4.41833056731215,-5.12548963494758,
107.576362689497));
#35692=CARTESIAN_POINT('Ctrl Pts',(-4.27937132056985,-5.24527680285168,
107.584958447045));
#35693=CARTESIAN_POINT('Ctrl Pts',(-4.13561940654779,-5.35933932355982,
107.593554204592));
#35694=CARTESIAN_POINT('Ctrl Pts',(-3.98757292330089,-5.46731663445219,
107.60214996214));
#35695=CARTESIAN_POINT('Ctrl Pts',(-3.83938830765185,-5.57539469184662,
107.610753739821));
#35696=CARTESIAN_POINT('Ctrl Pts',(-3.68690137136883,-5.67737602660814,
107.619357517503));
#35697=CARTESIAN_POINT('Ctrl Pts',(-3.53063855954867,-5.77294382112177,
107.627961295185));
#35698=CARTESIAN_POINT('Ctrl Pts',(-3.3682344825807,-5.87226751352861,107.636903208853));
#35699=CARTESIAN_POINT('Ctrl Pts',(-3.20175206593238,-5.9646631704105,107.645845122521));
#35700=CARTESIAN_POINT('Ctrl Pts',(-3.03180835814051,-6.04982868183136,
107.654787036189));
#35701=CARTESIAN_POINT('Ctrl Pts',(-2.86784583217706,-6.13199678654658,
107.663414238519));
#35702=CARTESIAN_POINT('Ctrl Pts',(-2.70066179391385,-6.20743492554849,
107.67204144085));
#35703=CARTESIAN_POINT('Ctrl Pts',(-2.53082935546811,-6.27592158758384,
107.680668643181));
#35704=CARTESIAN_POINT('Ctrl Pts',(-2.36083517762041,-6.34447347268177,
107.689304061601));
#35705=CARTESIAN_POINT('Ctrl Pts',(-2.188187851084,-6.406060560975,107.697939480022));
#35706=CARTESIAN_POINT('Ctrl Pts',(-2.01347627982301,-6.46051099144565,
107.706574898442));
#35707=CARTESIAN_POINT('Ctrl Pts',(-1.83850659710088,-6.51504186467157,
107.715223074463));
#35708=CARTESIAN_POINT('Ctrl Pts',(-1.66146686887881,-6.56241492782876,
107.723871250484));
#35709=CARTESIAN_POINT('Ctrl Pts',(-1.48295828353281,-6.60250889657117,
107.732519426505));
#35710=CARTESIAN_POINT('Ctrl Pts',(-1.46407275205353,-6.60675068643997,
107.733434370737));
#35711=CARTESIAN_POINT('Ctrl Pts',(-1.44517078630128,-6.61091105022795,
107.734349314969));
#35712=CARTESIAN_POINT('Ctrl Pts',(-1.42625310231533,-6.61498987815824,
107.735264259201));
#35713=CARTESIAN_POINT('Ctrl Pts',(-1.25616980984483,-6.65166141175181,
107.743490251742));
#35714=CARTESIAN_POINT('Ctrl Pts',(-1.0844480393287,-6.68181714361858,107.751716244283));
#35715=CARTESIAN_POINT('Ctrl Pts',(-0.91162781215005,-6.70531309724718,
107.759942236825));
#35716=CARTESIAN_POINT('Ctrl Pts',(-0.738988764641646,-6.72878441840537,
107.768159605476));
#35717=CARTESIAN_POINT('Ctrl Pts',(-0.56525390581976,-6.74560981703483,
107.776376974128));
#35718=CARTESIAN_POINT('Ctrl Pts',(-0.390975243171381,-6.75569591968341,
107.784594342779));
#35719=CARTESIAN_POINT('Ctrl Pts',(-0.216844416769153,-6.76577346654248,
107.792804740841));
#35720=CARTESIAN_POINT('Ctrl Pts',(-0.0421710609531744,-6.76912308256552,
107.801015138904));
#35721=CARTESIAN_POINT('Ctrl Pts',(0.132485768440468,-6.76570295838952,
107.809225536966));
#35722=CARTESIAN_POINT('Ctrl Pts',(0.307029379032054,-6.76228505126031,
107.817430612755));
#35723=CARTESIAN_POINT('Ctrl Pts',(0.481556127602511,-6.75210615227238,
107.825635688544));
#35724=CARTESIAN_POINT('Ctrl Pts',(0.655504918904233,-6.73517648627654,
107.833840764333));
#35725=CARTESIAN_POINT('Ctrl Pts',(0.82937573990617,-6.71825440878489,107.842042162302));
#35726=CARTESIAN_POINT('Ctrl Pts',(1.0026687639085,-6.69458762748705,107.850243560272));
#35727=CARTESIAN_POINT('Ctrl Pts',(1.17482588738742,-6.66423837616305,107.858444958241));
#35728=CARTESIAN_POINT('Ctrl Pts',(1.34696952608683,-6.63389150204515,107.866645713809));
#35729=CARTESIAN_POINT('Ctrl Pts',(1.51797708740693,-6.59686325407021,107.874846469377));
#35730=CARTESIAN_POINT('Ctrl Pts',(1.68729818408293,-6.55326741694481,107.883047224944));
#35731=CARTESIAN_POINT('Ctrl Pts',(1.85661842068835,-6.50967180126551,107.891247938856));
#35732=CARTESIAN_POINT('Ctrl Pts',(2.02425186239254,-6.45950875121017,107.899448652768));
#35733=CARTESIAN_POINT('Ctrl Pts',(2.18966098654431,-6.40294258634308,107.90764936668));
#35734=CARTESIAN_POINT('Ctrl Pts',(2.35509924674841,-6.34636645760763,107.915851525109));
#35735=CARTESIAN_POINT('Ctrl Pts',(2.51831206970158,-6.28338508291823,107.924053683539));
#35736=CARTESIAN_POINT('Ctrl Pts',(2.67877964078278,-6.21421182742653,107.932255841968));
#35737=CARTESIAN_POINT('Ctrl Pts',(2.83930455851148,-6.14501385133692,107.940460931621));
#35738=CARTESIAN_POINT('Ctrl Pts',(2.99708194111754,-6.06961972818204,107.948666021274));
#35739=CARTESIAN_POINT('Ctrl Pts',(3.1516143525597,-5.98828990386569,107.956871110927));
#35740=CARTESIAN_POINT('Ctrl Pts',(3.30632329901144,-5.90686716984075,107.965085573925));
#35741=CARTESIAN_POINT('Ctrl Pts',(3.45777955091906,-5.81949535480991,107.973300036923));
#35742=CARTESIAN_POINT('Ctrl Pts',(3.60551165794221,-5.72648013045036,107.981514499921));
#35743=CARTESIAN_POINT('Ctrl Pts',(3.75333129156968,-5.63340979751014,107.989733829728));
#35744=CARTESIAN_POINT('Ctrl Pts',(3.89742208688876,-5.53468959248881,107.997953159536));
#35745=CARTESIAN_POINT('Ctrl Pts',(4.03734385191801,-5.43066695916623,108.006172489343));
#35746=CARTESIAN_POINT('Ctrl Pts',(4.17748241723885,-5.32648314908012,108.014404554504));
#35747=CARTESIAN_POINT('Ctrl Pts',(4.31343876444354,-5.21698071697537,108.022636619664));
#35748=CARTESIAN_POINT('Ctrl Pts',(4.44480688958729,-5.10254649310297,108.030868684825));
#35749=CARTESIAN_POINT('Ctrl Pts',(4.56288999321656,-4.99968479585735,108.038268256086));
#35750=CARTESIAN_POINT('Ctrl Pts',(4.67726631022453,-4.89283899070071,108.045667827348));
#35751=CARTESIAN_POINT('Ctrl Pts',(4.78766833474416,-4.78231334361186,108.053067398609));
#35752=CARTESIAN_POINT('Ctrl Pts',(4.90934823851321,-4.66049718887831,108.061222857016));
#35753=CARTESIAN_POINT('Ctrl Pts',(5.02657439131357,-4.53383532421019,108.069378315422));
#35754=CARTESIAN_POINT('Ctrl Pts',(5.13893230645968,-4.40268824124819,108.077533773829));
#35755=CARTESIAN_POINT('Ctrl Pts',(5.25115346725375,-4.27170078152526,108.085679305971));
#35756=CARTESIAN_POINT('Ctrl Pts',(5.35851794975707,-4.13623924461395,108.093824838113));
#35757=CARTESIAN_POINT('Ctrl Pts',(5.46064631275775,-3.99670249667963,108.101970370255));
#35758=CARTESIAN_POINT('Ctrl Pts',(5.56267184766199,-3.85730624153059,108.110107701055));
#35759=CARTESIAN_POINT('Ctrl Pts',(5.65947154441353,-3.71384323670518,108.118245031856));
#35760=CARTESIAN_POINT('Ctrl Pts',(5.7507046533086,-3.56674711612903,108.126382362656));
#35761=CARTESIAN_POINT('Ctrl Pts',(5.84186507693061,-3.41976818679871,108.134513210459));
#35762=CARTESIAN_POINT('Ctrl Pts',(5.92746755136478,-3.26916221418646,108.14264405826));
#35763=CARTESIAN_POINT('Ctrl Pts',(6.0072132843546,-3.11539364387129,108.150774906062));
#35764=CARTESIAN_POINT('Ctrl Pts',(6.08691223601707,-2.96171527898222,108.158900984056));
#35765=CARTESIAN_POINT('Ctrl Pts',(6.16076112060873,-2.80487833479093,108.16702706205));
#35766=CARTESIAN_POINT('Ctrl Pts',(6.22850595567014,-2.6453738034882,108.175153140044));
#35767=CARTESIAN_POINT('Ctrl Pts',(6.29649100154348,-2.48530369825005,108.183308031626));
#35768=CARTESIAN_POINT('Ctrl Pts',(6.35832843998911,-2.32254737285463,108.191462923208));
#35769=CARTESIAN_POINT('Ctrl Pts',(6.41380916033727,-2.1576239372916,108.19961781479));
#35770=CARTESIAN_POINT('Ctrl Pts',(6.46907352527439,-1.99334364546333,108.207740905147));
#35771=CARTESIAN_POINT('Ctrl Pts',(6.51803055986769,-1.82691346963807,108.215863995503));
#35772=CARTESIAN_POINT('Ctrl Pts',(6.56052278018734,-1.65886402415721,108.223987085859));
#35773=CARTESIAN_POINT('Ctrl Pts',(6.60301833719015,-1.49080138266653,108.232110814078));
#35774=CARTESIAN_POINT('Ctrl Pts',(6.63904797902274,-1.32111957290623,108.240234542296));
#35775=CARTESIAN_POINT('Ctrl Pts',(6.66850486910148,-1.15036160000663,108.248358270515));
#35776=CARTESIAN_POINT('Ctrl Pts',(6.69796967640807,-0.979557731909891,
108.256484182175));
#35777=CARTESIAN_POINT('Ctrl Pts',(6.72085815220533,-0.807677485085201,
108.264610093835));
#35778=CARTESIAN_POINT('Ctrl Pts',(6.73711507467389,-0.635271178790456,
108.272736005496));
#35779=CARTESIAN_POINT('Ctrl Pts',(6.75347596185154,-0.461762316245421,
108.280913883206));
#35780=CARTESIAN_POINT('Ctrl Pts',(6.76312014708903,-0.287721016406869,
108.289091760916));
#35781=CARTESIAN_POINT('Ctrl Pts',(6.76604456939785,-0.11370965184142,108.297269638626));
#35782=CARTESIAN_POINT('Ctrl Pts',(6.76895503407326,0.0594711942219803,
108.305408485099));
#35783=CARTESIAN_POINT('Ctrl Pts',(6.76520980862204,0.232622025700009,108.313547331573));
#35784=CARTESIAN_POINT('Ctrl Pts',(6.75485810033358,0.405192601558612,108.321686178046));
#35785=CARTESIAN_POINT('Ctrl Pts',(6.74443192695163,0.57900456518686,108.329883571374));
#35786=CARTESIAN_POINT('Ctrl Pts',(6.7273039019828,0.752227517647732,108.338080964703));
#35787=CARTESIAN_POINT('Ctrl Pts',(6.70357679070904,0.924309045215469,108.346278358031));
#35788=CARTESIAN_POINT('Ctrl Pts',(6.67984967943529,1.09639057278308,108.354475751359));
#35789=CARTESIAN_POINT('Ctrl Pts',(6.64952360704994,1.26733031962272,108.362673144688));
#35790=CARTESIAN_POINT('Ctrl Pts',(6.61275244723277,1.43659112889404,108.370870538016));
#35791=CARTESIAN_POINT('Ctrl Pts',(6.57584906158015,1.60646058505126,108.379097408445));
#35792=CARTESIAN_POINT('Ctrl Pts',(6.53234442784925,1.77514463446334,108.387324278874));
#35793=CARTESIAN_POINT('Ctrl Pts',(6.48232728054897,1.94209217800047,108.395551149303));
#35794=CARTESIAN_POINT('Ctrl Pts',(6.43236715978589,2.10884937800911,108.403768639951));
#35795=CARTESIAN_POINT('Ctrl Pts',(6.37590941385774,2.27387367424087,108.411986130598));
#35796=CARTESIAN_POINT('Ctrl Pts',(6.31309387566238,2.43662363057452,108.420203621245));
#35797=CARTESIAN_POINT('Ctrl Pts',(6.25033734753254,2.5992206966224,108.428413392231));
#35798=CARTESIAN_POINT('Ctrl Pts',(6.1812350510357,2.7595473455245,108.436623163217));
#35799=CARTESIAN_POINT('Ctrl Pts',(6.10597678161969,2.91707671176492,108.444832934204));
#35800=CARTESIAN_POINT('Ctrl Pts',(6.02713985275013,3.08209686885243,108.453433093844));
#35801=CARTESIAN_POINT('Ctrl Pts',(5.94154727860017,3.24404682343997,108.462033253485));
#35802=CARTESIAN_POINT('Ctrl Pts',(5.84947474930506,3.40234245149463,108.470633413126));
#35803=CARTESIAN_POINT('Ctrl Pts',(5.7616953094453,3.55325718870524,108.478832570918));
#35804=CARTESIAN_POINT('Ctrl Pts',(5.66802666498871,3.70085028319838,108.48703172871));
#35805=CARTESIAN_POINT('Ctrl Pts',(5.56875541167771,3.84463940635663,108.495230886502));
#35806=CARTESIAN_POINT('Ctrl Pts',(5.4695108546408,3.98838986138372,108.503427839355));
#35807=CARTESIAN_POINT('Ctrl Pts',(5.36466689280645,4.12833808747981,108.511624792209));
#35808=CARTESIAN_POINT('Ctrl Pts',(5.25455380262281,4.26403017523823,108.519821745063));
#35809=CARTESIAN_POINT('Ctrl Pts',(5.14445031197702,4.39971043350999,108.528017983315));
#35810=CARTESIAN_POINT('Ctrl Pts',(5.02907883426714,4.53113501443973,108.536214221568));
#35811=CARTESIAN_POINT('Ctrl Pts',(4.90881036653292,4.65788254311108,108.54441045982));
#35812=CARTESIAN_POINT('Ctrl Pts',(4.78853052612792,4.78464205711777,108.552607473115));
#35813=CARTESIAN_POINT('Ctrl Pts',(4.66335302104256,4.90672337871442,108.560804486409));
#35814=CARTESIAN_POINT('Ctrl Pts',(4.53368621275221,5.02374146670592,108.569001499703));
#35815=CARTESIAN_POINT('Ctrl Pts',(4.4039367973248,5.14083410368463,108.577203735088));
#35816=CARTESIAN_POINT('Ctrl Pts',(4.2696926326895,5.25285682389974,108.585405970473));
#35817=CARTESIAN_POINT('Ctrl Pts',(4.13139621060566,5.35946399847906,108.593608205858));
#35818=CARTESIAN_POINT('Ctrl Pts',(3.99304832634251,5.46611084319195,108.601813493418));
#35819=CARTESIAN_POINT('Ctrl Pts',(3.85064546936945,5.56733791543589,108.610018780978));
#35820=CARTESIAN_POINT('Ctrl Pts',(3.70465965353445,5.66284255930482,108.618224068539));
#35821=CARTESIAN_POINT('Ctrl Pts',(3.55853625432459,5.75843721089912,108.626437089118));
#35822=CARTESIAN_POINT('Ctrl Pts',(3.40882345864226,5.84829847758847,108.634650109698));
#35823=CARTESIAN_POINT('Ctrl Pts',(3.25601903814054,5.93216899820516,108.642863130277));
#35824=CARTESIAN_POINT('Ctrl Pts',(3.20408814465992,5.96067256543187,108.645654342046));
#35825=CARTESIAN_POINT('Ctrl Pts',(3.15180035632282,5.98848460848285,108.648445553815));
#35826=CARTESIAN_POINT('Ctrl Pts',(3.09917575053272,6.01559628526632,108.651236765584));
#35827=CARTESIAN_POINT('Origin',(0.,0.,-3.69717978381041));
#35828=CARTESIAN_POINT('',(3.09917575053272,6.01559628526632,111.045835064059));
#35829=CARTESIAN_POINT('',(3.09917575053264,6.01559628526636,110.651392015122));
#35830=CARTESIAN_POINT('',(3.09917575053259,6.01559628526639,-3.69717978381041));
#35831=CARTESIAN_POINT('',(-6.76699862514327,-0.0043136190180686,109.697179783784));
#35832=CARTESIAN_POINT('Ctrl Pts',(-6.76699862514293,-0.00431361956973403,
109.69717978381));
#35833=CARTESIAN_POINT('Ctrl Pts',(-6.76685589271447,-0.228225378934505,
109.70772212165));
#35834=CARTESIAN_POINT('Ctrl Pts',(-6.75559591374126,-0.451750734100564,
109.718264459491));
#35835=CARTESIAN_POINT('Ctrl Pts',(-6.73335608618393,-0.673947191291592,
109.728806797331));
#35836=CARTESIAN_POINT('Ctrl Pts',(-6.71079662375845,-0.899337096593478,
109.739500651579));
#35837=CARTESIAN_POINT('Ctrl Pts',(-6.67693942269762,-1.12335988097693,
109.750194505826));
#35838=CARTESIAN_POINT('Ctrl Pts',(-6.63197761234058,-1.3450509095991,109.760888360074));
#35839=CARTESIAN_POINT('Ctrl Pts',(-6.62505575980767,-1.37918015385788,
109.762534674613));
#35840=CARTESIAN_POINT('Ctrl Pts',(-6.61787081791661,-1.41325416636877,
109.764180989153));
#35841=CARTESIAN_POINT('Ctrl Pts',(-6.61042359516057,-1.4472694609313,109.765827303692));
#35842=CARTESIAN_POINT('Ctrl Pts',(-6.57321866317101,-1.61720351047717,
109.774051983211));
#35843=CARTESIAN_POINT('Ctrl Pts',(-6.52940775532851,-1.78592594270599,
109.78227666273));
#35844=CARTESIAN_POINT('Ctrl Pts',(-6.47908372953471,-1.95288581992872,
109.790501342249));
#35845=CARTESIAN_POINT('Ctrl Pts',(-6.42881259998526,-2.11967020343201,
109.798717376699));
#35846=CARTESIAN_POINT('Ctrl Pts',(-6.37204208792575,-2.28469538085837,
109.806933411149));
#35847=CARTESIAN_POINT('Ctrl Pts',(-6.30891606944647,-2.44742048464913,
109.815149445599));
#35848=CARTESIAN_POINT('Ctrl Pts',(-6.24584375930155,-2.61000714007112,
109.823358489754));
#35849=CARTESIAN_POINT('Ctrl Pts',(-6.17642684098778,-2.77029728703645,
109.831567533908));
#35850=CARTESIAN_POINT('Ctrl Pts',(-6.10085903600665,-2.92776502178299,
109.839776578063));
#35851=CARTESIAN_POINT('Ctrl Pts',(-6.02534039288434,-3.08513031334561,
109.847980281691));
#35852=CARTESIAN_POINT('Ctrl Pts',(-5.94367898836081,-3.23967652818743,
109.856183985319));
#35853=CARTESIAN_POINT('Ctrl Pts',(-5.85611673996379,-3.39089748118634,
109.864387688947));
#35854=CARTESIAN_POINT('Ctrl Pts',(-5.76859392625178,-3.54205033005641,
109.872587697941));
#35855=CARTESIAN_POINT('Ctrl Pts',(-5.67517574239427,-3.68988059112708,
109.880787706935));
#35856=CARTESIAN_POINT('Ctrl Pts',(-5.57615019217884,-3.83390636743568,
109.888987715929));
#35857=CARTESIAN_POINT('Ctrl Pts',(-5.47713256025519,-3.97792062713955,
109.897187069233));
#35858=CARTESIAN_POINT('Ctrl Pts',(-5.37250865077825,-4.11813070796377,
109.905386422537));
#35859=CARTESIAN_POINT('Ctrl Pts',(-5.26261017731818,-4.25408311173949,
109.913585775841));
#35860=CARTESIAN_POINT('Ctrl Pts',(-5.15271242036359,-4.39003462914583,
109.921785075687));
#35861=CARTESIAN_POINT('Ctrl Pts',(-5.03754039245939,-4.52172824529911,
109.929984375534));
#35862=CARTESIAN_POINT('Ctrl Pts',(-4.91746645641509,-4.64874312583869,
109.938183675381));
#35863=CARTESIAN_POINT('Ctrl Pts',(-4.79737152062709,-4.77578022002449,
109.946384409204));
#35864=CARTESIAN_POINT('Ctrl Pts',(-4.67237321497657,-4.89813668780901,
109.954585143027));
#35865=CARTESIAN_POINT('Ctrl Pts',(-4.54288118648516,-5.0154281497674,109.96278587685));
#35866=CARTESIAN_POINT('Ctrl Pts',(-4.41334301973963,-5.13276140289502,
109.97098953261));
#35867=CARTESIAN_POINT('Ctrl Pts',(-4.27930820618762,-5.24502581466851,
109.979193188369));
#35868=CARTESIAN_POINT('Ctrl Pts',(-4.14121995070203,-5.35187689693135,
109.987396844129));
#35869=CARTESIAN_POINT('Ctrl Pts',(-4.00297350624245,-5.45885038397808,
109.995609897704));
#35870=CARTESIAN_POINT('Ctrl Pts',(-3.86066462674346,-5.56039793262255,
110.003822951279));
#35871=CARTESIAN_POINT('Ctrl Pts',(-3.71476689498273,-5.65621745656409,
110.012036004854));
#35872=CARTESIAN_POINT('Ctrl Pts',(-3.56878283226078,-5.75209367906774,
110.020253918278));
#35873=CARTESIAN_POINT('Ctrl Pts',(-3.41920599069867,-5.84223493578066,
110.028471831701));
#35874=CARTESIAN_POINT('Ctrl Pts',(-3.26653499439086,-5.92638491244198,
110.036689745124));
#35875=CARTESIAN_POINT('Ctrl Pts',(-3.11362588282745,-6.01066613468161,
110.04492047572));
#35876=CARTESIAN_POINT('Ctrl Pts',(-2.95761329268543,-6.08893724214638,
110.053151206316));
#35877=CARTESIAN_POINT('Ctrl Pts',(-2.79901751809191,-6.16098936319603,
110.061381936912));
#35878=CARTESIAN_POINT('Ctrl Pts',(-2.65336626681946,-6.22716061911135,
110.068940878587));
#35879=CARTESIAN_POINT('Ctrl Pts',(-2.50553671752515,-6.28808713324493,
110.076499820263));
#35880=CARTESIAN_POINT('Ctrl Pts',(-2.3559424962054,-6.34364437485058,110.084058761939));
#35881=CARTESIAN_POINT('Ctrl Pts',(-2.19457398699976,-6.40357442545274,
110.092212654106));
#35882=CARTESIAN_POINT('Ctrl Pts',(-2.03065291637443,-6.45744132991262,
110.100366546273));
#35883=CARTESIAN_POINT('Ctrl Pts',(-1.86467927664805,-6.50501807801019,
110.108520438439));
#35884=CARTESIAN_POINT('Ctrl Pts',(-1.69890817113248,-6.55253676918291,
110.11666438058));
#35885=CARTESIAN_POINT('Ctrl Pts',(-1.53108982981379,-6.59378048312874,
110.12480832272));
#35886=CARTESIAN_POINT('Ctrl Pts',(-1.36174457958176,-6.62857003432714,
110.13295226486));
#35887=CARTESIAN_POINT('Ctrl Pts',(-1.19257033406992,-6.66332445506005,
110.141087983253));
#35888=CARTESIAN_POINT('Ctrl Pts',(-1.02187260468566,-6.69163761489769,
110.149223701646));
#35889=CARTESIAN_POINT('Ctrl Pts',(-0.850187255037952,-6.71337997072794,
110.157359420039));
#35890=CARTESIAN_POINT('Ctrl Pts',(-0.678639159086851,-6.73510494465159,
110.165488634339));
#35891=CARTESIAN_POINT('Ctrl Pts',(-0.506105376010765,-6.7502695281621,
110.173617848639));
#35892=CARTESIAN_POINT('Ctrl Pts',(-0.333132348388015,-6.75879514695167,
110.181747062939));
#35893=CARTESIAN_POINT('Ctrl Pts',(-0.160261234169782,-6.76731574256019,
110.189871487615));
#35894=CARTESIAN_POINT('Ctrl Pts',(0.0130482449213397,-6.76920514526511,
110.19799591229));
#35895=CARTESIAN_POINT('Ctrl Pts',(0.186244134243564,-6.764436570954,110.206120336966));
#35896=CARTESIAN_POINT('Ctrl Pts',(0.360491433488215,-6.75963904834414,
110.2142940821));
#35897=CARTESIAN_POINT('Ctrl Pts',(0.534623386956937,-6.74810240067998,
110.222467827234));
#35898=CARTESIAN_POINT('Ctrl Pts',(0.708076899331325,-6.7298526064568,110.230641572368));
#35899=CARTESIAN_POINT('Ctrl Pts',(0.880419666168669,-6.71171967857554,
110.23876297523));
#35900=CARTESIAN_POINT('Ctrl Pts',(1.0520922897976,-6.68695939252059,110.246884378092));
#35901=CARTESIAN_POINT('Ctrl Pts',(1.22254692741619,-6.65564933047597,110.255005780955));
#35902=CARTESIAN_POINT('Ctrl Pts',(1.3930147436899,-6.6243368477022,110.263127811721));
#35903=CARTESIAN_POINT('Ctrl Pts',(1.5622640264011,-6.58647364632309,110.271249842487));
#35904=CARTESIAN_POINT('Ctrl Pts',(1.72975674083793,-6.5421885189534,110.279371873253));
#35905=CARTESIAN_POINT('Ctrl Pts',(1.89729429941005,-6.49789153477998,110.287496078594));
#35906=CARTESIAN_POINT('Ctrl Pts',(2.06307399957685,-6.44716929451148,110.295620283936));
#35907=CARTESIAN_POINT('Ctrl Pts',(2.22657263568775,-6.39020056790133,110.303744489277));
#35908=CARTESIAN_POINT('Ctrl Pts',(2.39184103140226,-6.33261519424493,110.311956633519));
#35909=CARTESIAN_POINT('Ctrl Pts',(2.55477833010648,-6.26864744187902,110.320168777762));
#35910=CARTESIAN_POINT('Ctrl Pts',(2.71486533474273,-6.19853169825018,110.328380922004));
#35911=CARTESIAN_POINT('Ctrl Pts',(2.8734909214655,-6.12905603408306,110.33651809842));
#35912=CARTESIAN_POINT('Ctrl Pts',(3.02931773612832,-6.05354437649771,110.344655274837));
#35913=CARTESIAN_POINT('Ctrl Pts',(3.18186622310238,-5.97227061830592,110.352792451253));
#35914=CARTESIAN_POINT('Ctrl Pts',(3.33652285444479,-5.88987369711838,110.361042079409));
#35915=CARTESIAN_POINT('Ctrl Pts',(3.48780954592197,-5.80155444818604,110.369291707564));
#35916=CARTESIAN_POINT('Ctrl Pts',(3.63525807612075,-5.70764292155692,110.37754133572));
#35917=CARTESIAN_POINT('Ctrl Pts',(3.78270660631943,-5.61373139492788,110.385790963875));
#35918=CARTESIAN_POINT('Ctrl Pts',(3.92631669499138,-5.51422786174043,110.39404059203));
#35919=CARTESIAN_POINT('Ctrl Pts',(4.06565624941997,-5.40950351340605,110.402290220186));
#35920=CARTESIAN_POINT('Ctrl Pts',(4.20457758936896,-5.30509348528763,110.410515087864));
#35921=CARTESIAN_POINT('Ctrl Pts',(4.3396693489863,-5.1951819825892,110.418739955541));
#35922=CARTESIAN_POINT('Ctrl Pts',(4.47046790784446,-5.08007929907918,110.426964823219));
#35923=CARTESIAN_POINT('Ctrl Pts',(4.60111910748573,-4.96510629162562,110.435180424662));
#35924=CARTESIAN_POINT('Ctrl Pts',(4.72748647073325,-4.84495398395998,110.443396026106));
#35925=CARTESIAN_POINT('Ctrl Pts',(4.84913643400935,-4.71997508937951,110.451611627549));
#35926=CARTESIAN_POINT('Ctrl Pts',(4.97067378690417,-4.59511188674494,110.459819623878));
#35927=CARTESIAN_POINT('Ctrl Pts',(5.08750218785014,-4.465431250643,110.468027620206));
#35928=CARTESIAN_POINT('Ctrl Pts',(5.19922212118798,-4.33132523998714,110.476235616534));
#35929=CARTESIAN_POINT('Ctrl Pts',(5.31086107582188,-4.19731643428483,110.484437663405));
#35930=CARTESIAN_POINT('Ctrl Pts',(5.41739870942876,-4.05888891764186,110.492639710277));
#35931=CARTESIAN_POINT('Ctrl Pts',(5.51847322308392,-3.91647064154779,110.500841757148));
#35932=CARTESIAN_POINT('Ctrl Pts',(5.61949477089273,-3.77412699657741,110.50903950592));
#35933=CARTESIAN_POINT('Ctrl Pts',(5.71505869480656,-3.6277970501811,110.517237254691));
#35934=CARTESIAN_POINT('Ctrl Pts',(5.80484422325914,-3.4779408482168,110.525435003463));
#35935=CARTESIAN_POINT('Ctrl Pts',(5.89461262692539,-3.32811322831338,110.533631188679));
#35936=CARTESIAN_POINT('Ctrl Pts',(5.97860464085945,-3.17476099675327,110.541827373894));
#35937=CARTESIAN_POINT('Ctrl Pts',(6.05654333382081,-3.01837238351246,110.55002355911));
#35938=CARTESIAN_POINT('Ctrl Pts',(6.13447626105363,-2.86199533954819,110.55821913799));
#35939=CARTESIAN_POINT('Ctrl Pts',(6.20635659828984,-2.70258268200196,110.566414716871));
#35940=CARTESIAN_POINT('Ctrl Pts',(6.27195385526933,-2.54064634244362,110.574610295751));
#35941=CARTESIAN_POINT('Ctrl Pts',(6.33755819415582,-2.37869252017109,110.582806759429));
#35942=CARTESIAN_POINT('Ctrl Pts',(6.39687796660829,-2.21421480571479,110.591003223108));
#35943=CARTESIAN_POINT('Ctrl Pts',(6.44973120865177,-2.04774420671707,110.599199686786));
#35944=CARTESIAN_POINT('Ctrl Pts',(6.50259977281488,-1.88122534800373,110.607398526614));
#35945=CARTESIAN_POINT('Ctrl Pts',(6.54899796396364,-1.71271279589424,110.615597366442));
#35946=CARTESIAN_POINT('Ctrl Pts',(6.58879395725007,-1.54275182349752,110.62379620627));
#35947=CARTESIAN_POINT('Ctrl Pts',(6.62863151858366,-1.37261332202989,110.632003610019));
#35948=CARTESIAN_POINT('Ctrl Pts',(6.66185302246366,-1.2010237275144,110.640211013768));
#35949=CARTESIAN_POINT('Ctrl Pts',(6.68837778365413,-1.02853858611231,110.648418417517));
#35950=CARTESIAN_POINT('Ctrl Pts',(6.71491675291036,-0.855961052540755,
110.656630217586));
#35951=CARTESIAN_POINT('Ctrl Pts',(6.73475178771678,-0.682487371953734,
110.664842017655));
#35952=CARTESIAN_POINT('Ctrl Pts',(6.74785421614684,-0.508677184105277,
110.673053817724));
#35953=CARTESIAN_POINT('Ctrl Pts',(6.76097593318235,-0.334611123373883,
110.681277706711));
#35954=CARTESIAN_POINT('Ctrl Pts',(6.76734522321404,-0.160207923962732,
110.689501595697));
#35955=CARTESIAN_POINT('Ctrl Pts',(6.76698557477953,0.0139724989077925,
110.697725484683));
#35956=CARTESIAN_POINT('Ctrl Pts',(6.76665326584358,0.174912198439788,110.705324215933));
#35957=CARTESIAN_POINT('Ctrl Pts',(6.76057675465688,0.335661512626722,110.712922947183));
#35958=CARTESIAN_POINT('Ctrl Pts',(6.74881373515992,0.495784396806563,110.720521678433));
#35959=CARTESIAN_POINT('Ctrl Pts',(6.7360814713138,0.669101019269499,110.728746526755));
#35960=CARTESIAN_POINT('Ctrl Pts',(6.71665061774589,0.842170107914227,110.736971375077));
#35961=CARTESIAN_POINT('Ctrl Pts',(6.69053158575722,1.0144338815246,110.745196223399));
#35962=CARTESIAN_POINT('Ctrl Pts',(6.66444196958966,1.18650364793164,110.753411808718));
#35963=CARTESIAN_POINT('Ctrl Pts',(6.63167922716819,1.35776955381536,110.761627394038));
#35964=CARTESIAN_POINT('Ctrl Pts',(6.59230570527272,1.52767617256695,110.769842979357));
#35965=CARTESIAN_POINT('Ctrl Pts',(6.5529686157684,1.69742557641634,110.77805096278));
#35966=CARTESIAN_POINT('Ctrl Pts',(6.50703300933812,1.86581785066255,110.786258946203));
#35967=CARTESIAN_POINT('Ctrl Pts',(6.45461273974146,2.03230494266172,110.794466929627));
#35968=CARTESIAN_POINT('Ctrl Pts',(6.40223044583732,2.19867142363268,110.802668966803));
#35969=CARTESIAN_POINT('Ctrl Pts',(6.343372953196,2.36313513063809,110.81087100398));
#35970=CARTESIAN_POINT('Ctrl Pts',(6.27820470089683,2.52516033820369,110.819073041156));
#35971=CARTESIAN_POINT('Ctrl Pts',(6.21307057316136,2.68710070323751,110.827270783436));
#35972=CARTESIAN_POINT('Ctrl Pts',(6.14163240252789,2.84660478053349,110.835468525715));
#35973=CARTESIAN_POINT('Ctrl Pts',(6.06410380771575,3.00315401024445,110.843666267994));
#35974=CARTESIAN_POINT('Ctrl Pts',(5.98658995368304,3.15967347470982,110.851862451609));
#35975=CARTESIAN_POINT('Ctrl Pts',(5.90298813552255,3.31323888670916,110.860058635223));
#35976=CARTESIAN_POINT('Ctrl Pts',(5.81355938279019,3.46335333207171,110.868254818837));
#35977=CARTESIAN_POINT('Ctrl Pts',(5.72413721326177,3.61345672691661,110.876450399098));
#35978=CARTESIAN_POINT('Ctrl Pts',(5.62888914629168,3.76010935232465,110.884645979359));
#35979=CARTESIAN_POINT('Ctrl Pts',(5.52812125693116,3.90284055127363,110.89284155962));
#35980=CARTESIAN_POINT('Ctrl Pts',(5.42734245196785,4.04558721146808,110.901038027661));
#35981=CARTESIAN_POINT('Ctrl Pts',(5.32104284035047,4.18441130570462,110.909234495702));
#35982=CARTESIAN_POINT('Ctrl Pts',(5.20957077853204,4.31887268896237,110.917430963742));
#35983=CARTESIAN_POINT('Ctrl Pts',(5.09806636048116,4.45337310140558,110.925629810916));
#35984=CARTESIAN_POINT('Ctrl Pts',(4.98138673064542,4.58350800431764,110.933828658089));
#35985=CARTESIAN_POINT('Ctrl Pts',(4.85991935166817,4.70887172210937,110.942027505262));
#35986=CARTESIAN_POINT('Ctrl Pts',(4.73832502746805,4.83436645717691,110.950234921028));
#35987=CARTESIAN_POINT('Ctrl Pts',(4.61193320749025,4.95507978699414,110.958442336794));
#35988=CARTESIAN_POINT('Ctrl Pts',(4.48116764291128,5.07064350513078,110.96664975256));
#35989=CARTESIAN_POINT('Ctrl Pts',(4.35033199258888,5.18626916135582,110.974861567212));
#35990=CARTESIAN_POINT('Ctrl Pts',(4.21511820211421,5.29673947693754,110.983073381865));
#35991=CARTESIAN_POINT('Ctrl Pts',(4.07598158451339,5.40172779050442,110.991285196517));
#35992=CARTESIAN_POINT('Ctrl Pts',(3.93664006709109,5.50687071532374,110.999509104314));
#35993=CARTESIAN_POINT('Ctrl Pts',(3.79336447204605,5.6065152994204,111.007733012112));
#35994=CARTESIAN_POINT('Ctrl Pts',(3.64663854193452,5.70037861413413,111.01595691991));
#35995=CARTESIAN_POINT('Ctrl Pts',(3.51106649228901,5.78710658343437,111.023555658833));
#35996=CARTESIAN_POINT('Ctrl Pts',(3.37254922635882,5.86889923311976,111.031154397756));
#35997=CARTESIAN_POINT('Ctrl Pts',(3.23148476624057,5.94556937606107,111.03875313668));
#35998=CARTESIAN_POINT('Ctrl Pts',(3.18766134271625,5.96938790656103,111.041113779139));
#35999=CARTESIAN_POINT('Ctrl Pts',(3.14355466612796,5.99273270657428,111.043474421599));
#36000=CARTESIAN_POINT('Ctrl Pts',(3.09917575053272,6.01559628526632,111.045835064059));
#36001=CARTESIAN_POINT('Ctrl Pts',(3.09917575053271,6.01559628526633,109.0454843164));
#36002=CARTESIAN_POINT('Ctrl Pts',(2.94519484763712,6.09492572455532,109.053621569559));
#36003=CARTESIAN_POINT('Ctrl Pts',(2.78828698403167,6.16827687821786,109.061758822718));
#36004=CARTESIAN_POINT('Ctrl Pts',(2.62896692083732,6.23544881537353,109.069896075877));
#36005=CARTESIAN_POINT('Ctrl Pts',(2.46953857203641,6.30266640750706,109.07803885971));
#36006=CARTESIAN_POINT('Ctrl Pts',(2.30769509834838,6.36369628735901,109.086181643543));
#36007=CARTESIAN_POINT('Ctrl Pts',(2.14396668018385,6.41838732660015,109.094324427376));
#36008=CARTESIAN_POINT('Ctrl Pts',(1.98000008270331,6.47315792609397,109.102479056695));
#36009=CARTESIAN_POINT('Ctrl Pts',(1.81414341501669,6.52157117023759,109.110633686014));
#36010=CARTESIAN_POINT('Ctrl Pts',(1.64693819141886,6.56352676490665,109.118788315333));
#36011=CARTESIAN_POINT('Ctrl Pts',(1.57465309658292,6.58166473975154,109.122313672622));
#36012=CARTESIAN_POINT('Ctrl Pts',(1.50211604506174,6.59859646835207,109.12583902991));
#36013=CARTESIAN_POINT('Ctrl Pts',(1.4293710483408,6.61431685105614,109.129364387199));
#36014=CARTESIAN_POINT('Ctrl Pts',(1.25951018591324,6.65102422454118,109.13759615923));
#36015=CARTESIAN_POINT('Ctrl Pts',(1.08798504384715,6.68123804399826,109.145827931261));
#36016=CARTESIAN_POINT('Ctrl Pts',(0.91533308406224,6.70480830040808,109.154059703292));
#36017=CARTESIAN_POINT('Ctrl Pts',(0.742887287971219,6.72835041157627,109.162281645764));
#36018=CARTESIAN_POINT('Ctrl Pts',(0.569317704949634,6.74526470829783,109.170503588236));
#36019=CARTESIAN_POINT('Ctrl Pts',(0.395174483133718,6.75545158578463,109.178725530709));
#36020=CARTESIAN_POINT('Ctrl Pts',(0.221204314601722,6.76562834015216,109.186939302699));
#36021=CARTESIAN_POINT('Ctrl Pts',(0.0466619977576692,6.76909096827847,
109.195153074688));
#36022=CARTESIAN_POINT('Ctrl Pts',(-0.127894557792987,6.7657913049463,109.203366846678));
#36023=CARTESIAN_POINT('Ctrl Pts',(-0.302312610548465,6.76249425974895,
109.211574101409));
#36024=CARTESIAN_POINT('Ctrl Pts',(-0.476744522874798,6.75244561689631,
109.219781356139));
#36025=CARTESIAN_POINT('Ctrl Pts',(-0.650629627096702,6.73564919576013,
109.227988610869));
#36026=CARTESIAN_POINT('Ctrl Pts',(-0.824411578969602,6.71886273861886,
109.236190996881));
#36027=CARTESIAN_POINT('Ctrl Pts',(-0.997647013240173,6.69533651185546,
109.244393382893));
#36028=CARTESIAN_POINT('Ctrl Pts',(-1.16977753718885,6.66512636890617,109.252595768905));
#36029=CARTESIAN_POINT('Ctrl Pts',(-1.34185668435149,6.63492524295175,109.260795706704));
#36030=CARTESIAN_POINT('Ctrl Pts',(-1.51283122497298,6.59804423278493,109.268995644503));
#36031=CARTESIAN_POINT('Ctrl Pts',(-1.68214989877164,6.55459081240489,109.277195582301));
#36032=CARTESIAN_POINT('Ctrl Pts',(-1.85144489744949,6.51114346793458,109.285394373537));
#36033=CARTESIAN_POINT('Ctrl Pts',(-2.01908414317863,6.46112563182285,109.293593164773));
#36034=CARTESIAN_POINT('Ctrl Pts',(-2.18452852858125,6.40469547346434,109.301791956009));
#36035=CARTESIAN_POINT('Ctrl Pts',(-2.34997979305907,6.34826296877476,109.309991088145));
#36036=CARTESIAN_POINT('Ctrl Pts',(-2.51323567611532,6.28541772630625,109.318190220281));
#36037=CARTESIAN_POINT('Ctrl Pts',(-2.67377408946657,6.21636719624068,109.326389352418));
#36038=CARTESIAN_POINT('Ctrl Pts',(-2.83434830030004,6.14730126901831,109.334590312829));
#36039=CARTESIAN_POINT('Ctrl Pts',(-2.99220350535078,6.07202743990208,109.34279127324));
#36040=CARTESIAN_POINT('Ctrl Pts',(-3.14683933625071,5.99080054682387,109.350992233651));
#36041=CARTESIAN_POINT('Ctrl Pts',(-3.30162009814966,5.90949752459311,109.359200880336));
#36042=CARTESIAN_POINT('Ctrl Pts',(-3.45317513972735,5.82223045789055,109.367409527021));
#36043=CARTESIAN_POINT('Ctrl Pts',(-3.60102955021838,5.72929971099907,109.375618173706));
#36044=CARTESIAN_POINT('Ctrl Pts',(-3.74895455055768,5.63632459635893,109.383830739429));
#36045=CARTESIAN_POINT('Ctrl Pts',(-3.89317510145142,5.53768061245887,109.392043305153));
#36046=CARTESIAN_POINT('Ctrl Pts',(-4.03324693963188,5.43371034597448,109.400255870876));
#36047=CARTESIAN_POINT('Ctrl Pts',(-4.17351097658677,5.3295974172815,109.408479705425));
#36048=CARTESIAN_POINT('Ctrl Pts',(-4.30961464440236,5.22014382444315,109.416703539974));
#36049=CARTESIAN_POINT('Ctrl Pts',(-4.44114737597533,5.10573197346546,109.424927374522));
#36050=CARTESIAN_POINT('Ctrl Pts',(-4.56200121382049,5.00060900429826,109.432483531497));
#36051=CARTESIAN_POINT('Ctrl Pts',(-4.67899645747007,4.8913007846865,109.440039688471));
#36052=CARTESIAN_POINT('Ctrl Pts',(-4.79184372094166,4.77812962926624,109.447595845445));
#36053=CARTESIAN_POINT('Ctrl Pts',(-4.92096301084992,4.64863974376593,109.456241563498));
#36054=CARTESIAN_POINT('Ctrl Pts',(-5.04494591497753,4.51379721994059,109.46488728155));
#36055=CARTESIAN_POINT('Ctrl Pts',(-5.16335031922437,4.3740258893799,109.473532999602));
#36056=CARTESIAN_POINT('Ctrl Pts',(-5.28160271634628,4.23443399672308,109.482167618315));
#36057=CARTESIAN_POINT('Ctrl Pts',(-5.39429069811321,4.08992614645227,109.490802237027));
#36058=CARTESIAN_POINT('Ctrl Pts',(-5.50100930137731,3.94096253041822,109.499436855739));
#36059=CARTESIAN_POINT('Ctrl Pts',(-5.61149679114026,3.78673809814296,109.508376415642));
#36060=CARTESIAN_POINT('Ctrl Pts',(-5.71558532953905,3.62773764238932,109.517315975544));
#36061=CARTESIAN_POINT('Ctrl Pts',(-5.81286942987335,3.46451121967355,109.526255535447));
#36062=CARTESIAN_POINT('Ctrl Pts',(-5.90657422807939,3.30729026630176,109.534866188717));
#36063=CARTESIAN_POINT('Ctrl Pts',(-5.9939661405276,3.14614904002357,109.543476841988));
#36064=CARTESIAN_POINT('Ctrl Pts',(-6.07472520682089,2.98161074951357,109.552087495258));
#36065=CARTESIAN_POINT('Ctrl Pts',(-6.15540782925466,2.81722820550418,109.560689997969));
#36066=CARTESIAN_POINT('Ctrl Pts',(-6.2294699891014,2.6494552810904,109.56929250068));
#36067=CARTESIAN_POINT('Ctrl Pts',(-6.29663690795752,2.47884098912116,109.577895003391));
#36068=CARTESIAN_POINT('Ctrl Pts',(-6.36372823179869,2.30841872010268,109.586487824159));
#36069=CARTESIAN_POINT('Ctrl Pts',(-6.42393968504066,2.13516174643677,109.595080644926));
#36070=CARTESIAN_POINT('Ctrl Pts',(-6.47704392625067,1.95964052249879,109.603673465694));
#36071=CARTESIAN_POINT('Ctrl Pts',(-6.48330250229116,1.93895454899262,109.604686168652));
#36072=CARTESIAN_POINT('Ctrl Pts',(-6.48946241587,1.91823714958004,109.60569887161));
#36073=CARTESIAN_POINT('Ctrl Pts',(-6.49552333880982,1.89748927664348,109.606711574569));
#36074=CARTESIAN_POINT('Ctrl Pts',(-6.54330971000693,1.73390601258575,109.614696068013));
#36075=CARTESIAN_POINT('Ctrl Pts',(-6.58490844078597,1.56852987082132,109.622680561458));
#36076=CARTESIAN_POINT('Ctrl Pts',(-6.6201971399517,1.40188402807626,109.630665054903));
#36077=CARTESIAN_POINT('Ctrl Pts',(-6.65549177944812,1.2352101329678,109.638650892419));
#36078=CARTESIAN_POINT('Ctrl Pts',(-6.6844742029827,1.06726648420744,109.646636729935));
#36079=CARTESIAN_POINT('Ctrl Pts',(-6.70707341085314,0.8985851442278,109.654622567451));
#36080=CARTESIAN_POINT('Ctrl Pts',(-6.72969228739623,0.72975699653351,109.662615355247));
#36081=CARTESIAN_POINT('Ctrl Pts',(-6.74591681128877,0.560190252371543,
109.670608143043));
#36082=CARTESIAN_POINT('Ctrl Pts',(-6.75572795343816,0.390421335398477,
109.678600930839));
#36083=CARTESIAN_POINT('Ctrl Pts',(-6.76332979699452,0.258881426190013,
109.684793881821));
#36084=CARTESIAN_POINT('Ctrl Pts',(-6.76708247132931,0.127220256194025,
109.690986832802));
#36085=CARTESIAN_POINT('Ctrl Pts',(-6.76699862514328,-0.00431361901788746,
109.697179783784));
#36086=CARTESIAN_POINT('',(-6.767,6.1014472012115E-12,109.30282021619));
#36087=CARTESIAN_POINT('Ctrl Pts',(3.09917575053272,6.01559628526632,108.651236765584));
#36088=CARTESIAN_POINT('Ctrl Pts',(2.94407565780403,6.09550232009573,108.659463282396));
#36089=CARTESIAN_POINT('Ctrl Pts',(2.78604865213012,6.16932092097397,108.667689799207));
#36090=CARTESIAN_POINT('Ctrl Pts',(2.6256200252445,6.2368588634853,108.675916316018));
#36091=CARTESIAN_POINT('Ctrl Pts',(2.54269120615467,6.27177059915835,108.68016876982));
#36092=CARTESIAN_POINT('Ctrl Pts',(2.4591209175279,6.30500491425731,108.684421223622));
#36093=CARTESIAN_POINT('Ctrl Pts',(2.37498311842477,6.33654039576782,108.688673677424));
#36094=CARTESIAN_POINT('Ctrl Pts',(2.21222192667147,6.39754451767114,108.696899878443));
#36095=CARTESIAN_POINT('Ctrl Pts',(2.04688129247107,6.4523588191325,108.705126079462));
#36096=CARTESIAN_POINT('Ctrl Pts',(1.87947238656043,6.50075938242271,108.713352280481));
#36097=CARTESIAN_POINT('Ctrl Pts',(1.7122515292724,6.54910557788098,108.721569241096));
#36098=CARTESIAN_POINT('Ctrl Pts',(1.54296736792889,6.59105228254896,108.729786201712));
#36099=CARTESIAN_POINT('Ctrl Pts',(1.37215065393314,6.62642374006605,108.738003162328));
#36100=CARTESIAN_POINT('Ctrl Pts',(1.20149153224268,6.66176256453804,108.74621254213));
#36101=CARTESIAN_POINT('Ctrl Pts',(1.02930302272316,6.69053815065911,108.754421921931));
#36102=CARTESIAN_POINT('Ctrl Pts',(0.856130720629171,6.71262461256363,108.762631301733));
#36103=CARTESIAN_POINT('Ctrl Pts',(0.68308343815763,6.7346951294175,108.770834754873));
#36104=CARTESIAN_POINT('Ctrl Pts',(0.509054132095454,6.7500860956666,108.779038208014));
#36105=CARTESIAN_POINT('Ctrl Pts',(0.334598358714759,6.75872272980224,108.787241661154));
#36106=CARTESIAN_POINT('Ctrl Pts',(0.160233536149645,6.76735486131292,108.795440837504));
#36107=CARTESIAN_POINT('Ctrl Pts',(-0.0145569534579787,6.76923965808673,
108.803640013854));
#36108=CARTESIAN_POINT('Ctrl Pts',(-0.189212573766721,6.76435418956818,
108.811839190204));
#36109=CARTESIAN_POINT('Ctrl Pts',(-0.363835329985134,6.75946964032425,
108.820036823756));
#36110=CARTESIAN_POINT('Ctrl Pts',(-0.538322909153748,6.74781736711494,
108.828234457307));
#36111=CARTESIAN_POINT('Ctrl Pts',(-0.712114602225867,6.72942655753792,
108.836432090859));
#36112=CARTESIAN_POINT('Ctrl Pts',(-0.885893778030626,6.71103707255057,
108.844629133979));
#36113=CARTESIAN_POINT('Ctrl Pts',(-1.05897681077719,6.68591005464264,108.8528261771));
#36114=CARTESIAN_POINT('Ctrl Pts',(-1.23080799516007,6.65412659024835,108.86102322022));
#36115=CARTESIAN_POINT('Ctrl Pts',(-1.40265803351161,6.6223396384519,108.869221162752));
#36116=CARTESIAN_POINT('Ctrl Pts',(-1.57325559707273,6.5838948503112,108.877419105283));
#36117=CARTESIAN_POINT('Ctrl Pts',(-1.74205500329311,6.53892448079204,108.885617047814));
#36118=CARTESIAN_POINT('Ctrl Pts',(-1.9109036099483,6.49394100363356,108.893817379822));
#36119=CARTESIAN_POINT('Ctrl Pts',(-2.07795266878711,6.44242824879675,108.902017711831));
#36120=CARTESIAN_POINT('Ctrl Pts',(-2.24267144095204,6.38456841203367,108.910218043839));
#36121=CARTESIAN_POINT('Ctrl Pts',(-2.40756189459754,6.3266482696824,108.91842692281));
#36122=CARTESIAN_POINT('Ctrl Pts',(-2.57011687036094,6.26236794791452,108.926635801781));
#36123=CARTESIAN_POINT('Ctrl Pts',(-2.72982448024864,6.19195827723631,108.934844680752));
#36124=CARTESIAN_POINT('Ctrl Pts',(-2.88961782488563,6.12151080901378,108.943057966439));
#36125=CARTESIAN_POINT('Ctrl Pts',(-3.04656043442922,6.04492758954581,108.951271252126));
#36126=CARTESIAN_POINT('Ctrl Pts',(-3.20016494375342,5.96248549958586,108.959484537814));
#36127=CARTESIAN_POINT('Ctrl Pts',(-3.35399415754354,5.879922807009,108.967709838526));
#36128=CARTESIAN_POINT('Ctrl Pts',(-3.50447520308935,5.79148429746885,108.975935139238));
#36129=CARTESIAN_POINT('Ctrl Pts',(-3.65114854795072,5.69749096364333,108.98416043995));
#36130=CARTESIAN_POINT('Ctrl Pts',(-3.7837968954922,5.61248533140895,108.991599232244));
#36131=CARTESIAN_POINT('Ctrl Pts',(-3.91333115437953,5.52293706231391,108.999038024538));
#36132=CARTESIAN_POINT('Ctrl Pts',(-4.03943535765225,5.4291114366302,109.006476816832));
#36133=CARTESIAN_POINT('Ctrl Pts',(-4.17630503008599,5.32727595200764,109.014550656071));
#36134=CARTESIAN_POINT('Ctrl Pts',(-4.30955446625834,5.22008766297068,109.02262449531));
#36135=CARTESIAN_POINT('Ctrl Pts',(-4.43872698616404,5.10783630731243,109.030698334549));
#36136=CARTESIAN_POINT('Ctrl Pts',(-4.56774945848193,4.99571534351429,109.038762795167));
#36137=CARTESIAN_POINT('Ctrl Pts',(-4.69270416004923,4.87854325839703,109.046827255785));
#36138=CARTESIAN_POINT('Ctrl Pts',(-4.81316335252528,4.75665297682179,109.054891716403));
#36139=CARTESIAN_POINT('Ctrl Pts',(-4.93350898604421,4.63487760331604,109.062948574515));
#36140=CARTESIAN_POINT('Ctrl Pts',(-5.04936728488339,4.50839314912137,109.071005432627));
#36141=CARTESIAN_POINT('Ctrl Pts',(-5.16034367133203,4.37757263717502,109.079062290739));
#36142=CARTESIAN_POINT('Ctrl Pts',(-5.27123969934389,4.24684685287458,109.087113314848));
#36143=CARTESIAN_POINT('Ctrl Pts',(-5.37726061152404,4.11179154395132,109.095164338958));
#36144=CARTESIAN_POINT('Ctrl Pts',(-5.4780488726118,3.97281632463377,109.103215363067));
#36145=CARTESIAN_POINT('Ctrl Pts',(-5.58205542573057,3.82940345716147,109.11152346619));
#36146=CARTESIAN_POINT('Ctrl Pts',(-5.68048931894931,3.68181647099154,109.119831569313));
#36147=CARTESIAN_POINT('Ctrl Pts',(-5.77300244067269,3.53054270898783,109.128139672436));
#36148=CARTESIAN_POINT('Ctrl Pts',(-5.86259408574589,3.38404602892933,109.136185413541));
#36149=CARTESIAN_POINT('Ctrl Pts',(-5.94663302008584,3.23409222921794,109.144231154646));
#36150=CARTESIAN_POINT('Ctrl Pts',(-6.02484723544011,3.08115315906394,109.152276895751));
#36151=CARTESIAN_POINT('Ctrl Pts',(-6.10306004457755,2.92821683860823,109.160322492202));
#36152=CARTESIAN_POINT('Ctrl Pts',(-6.17544817281757,2.77229568653904,109.168368088652));
#36153=CARTESIAN_POINT('Ctrl Pts',(-6.24178595625474,2.61388543672081,109.176413685103));
#36154=CARTESIAN_POINT('Ctrl Pts',(-6.30813566481878,2.45544671048642,109.184460727859));
#36155=CARTESIAN_POINT('Ctrl Pts',(-6.36843271982456,2.29451834012415,109.192507770616));
#36156=CARTESIAN_POINT('Ctrl Pts',(-6.42249997207323,2.13161514085432,109.200554813373));
#36157=CARTESIAN_POINT('Ctrl Pts',(-6.4765876377089,1.96865043659004,109.208604894335));
#36158=CARTESIAN_POINT('Ctrl Pts',(-6.52444070196857,1.80370977322121,109.216654975297));
#36159=CARTESIAN_POINT('Ctrl Pts',(-6.56593218968929,1.63732204541504,109.224705056259));
#36160=CARTESIAN_POINT('Ctrl Pts',(-6.60746819406486,1.47075579846052,109.232763774237));
#36161=CARTESIAN_POINT('Ctrl Pts',(-6.64262890681234,1.3027397496562,109.240822492216));
#36162=CARTESIAN_POINT('Ctrl Pts',(-6.67133855704832,1.13381253178844,109.248881210195));
#36163=CARTESIAN_POINT('Ctrl Pts',(-6.70006664361088,0.96477683480887,109.256945103198));
#36164=CARTESIAN_POINT('Ctrl Pts',(-6.72233536982622,0.794829171801602,
109.265008996202));
#36165=CARTESIAN_POINT('Ctrl Pts',(-6.73812096766818,0.624511669282851,
109.273072889206));
#36166=CARTESIAN_POINT('Ctrl Pts',(-6.75392720729867,0.453971453762943,
109.281147326832));
#36167=CARTESIAN_POINT('Ctrl Pts',(-6.76323338022855,0.283060803695495,
109.289221764458));
#36168=CARTESIAN_POINT('Ctrl Pts',(-6.76606776734014,0.112320825142991,
109.297296202085));
#36169=CARTESIAN_POINT('Ctrl Pts',(-6.76668951966931,0.0748672328258921,
109.299067414062));
#36170=CARTESIAN_POINT('Ctrl Pts',(-6.7670000537757,0.0374218287909141,
109.30083862604));
#36171=CARTESIAN_POINT('Ctrl Pts',(-6.76699999999302,-9.72301229749807E-6,
109.302609838017));
#36172=CARTESIAN_POINT('Ctrl Pts',(-6.767,6.4861066398266E-12,109.30282021619));
#36173=CARTESIAN_POINT('Ctrl Pts',(-6.76700000000018,-0.186007249409342,
109.311569727996));
#36174=CARTESIAN_POINT('Ctrl Pts',(-6.75932637295473,-0.372014355521354,
109.320319239802));
#36175=CARTESIAN_POINT('Ctrl Pts',(-6.74400518266978,-0.557389537149031,
109.329068751608));
#36176=CARTESIAN_POINT('Ctrl Pts',(-6.72868405709709,-0.742763935805681,
109.337818226458));
#36177=CARTESIAN_POINT('Ctrl Pts',(-6.70571545653067,-0.927506129689624,
109.346567701309));
#36178=CARTESIAN_POINT('Ctrl Pts',(-6.67517739415735,-1.11098863924465,
109.35531717616));
#36179=CARTESIAN_POINT('Ctrl Pts',(-6.64463945823167,-1.29447038906158,
109.364066614782));
#36180=CARTESIAN_POINT('Ctrl Pts',(-6.60653217027233,-1.47669218227876,
109.372816053403));
#36181=CARTESIAN_POINT('Ctrl Pts',(-6.56098496116797,-1.65703510503784,
109.381565492025));
#36182=CARTESIAN_POINT('Ctrl Pts',(-6.51543793687604,-1.83737729603715,
109.390314895146));
#36183=CARTESIAN_POINT('Ctrl Pts',(-6.46245112202726,-2.01584035396779,
109.399064298266));
#36184=CARTESIAN_POINT('Ctrl Pts',(-6.40220448416326,-2.19181813637899,
109.407813701386));
#36185=CARTESIAN_POINT('Ctrl Pts',(-6.34195808575274,-2.36779521935712,
109.416563069732));
#36186=CARTESIAN_POINT('Ctrl Pts',(-6.27445201489324,-2.54128677544608,
109.425312438077));
#36187=CARTESIAN_POINT('Ctrl Pts',(-6.19991555136274,-2.71170355237634,
109.434061806422));
#36188=CARTESIAN_POINT('Ctrl Pts',(-6.12537937789128,-2.88211966612882,
109.442811140719));
#36189=CARTESIAN_POINT('Ctrl Pts',(-6.04381298133705,-3.0494607621027,109.451560475016));
#36190=CARTESIAN_POINT('Ctrl Pts',(-5.95549339426392,-3.21315848206696,
109.460309809313));
#36191=CARTESIAN_POINT('Ctrl Pts',(-5.86717414355249,-3.37685557859483,
109.469059110289));
#36192=CARTESIAN_POINT('Ctrl Pts',(-5.77210188986328,-3.53690907467164,
109.477808411264));
#36193=CARTESIAN_POINT('Ctrl Pts',(-5.6705995346716,-3.69277536784764,109.48655771224));
#36194=CARTESIAN_POINT('Ctrl Pts',(-5.56909755761868,-3.84864108035645,
109.495306980621));
#36195=CARTESIAN_POINT('Ctrl Pts',(-5.46116568338183,-4.00031938104125,
109.504056249001));
#36196=CARTESIAN_POINT('Ctrl Pts',(-5.34717048686239,-4.14729511663058,
109.512805517382));
#36197=CARTESIAN_POINT('Ctrl Pts',(-5.23317570555654,-4.29427031687874,
109.521554753895));
#36198=CARTESIAN_POINT('Ctrl Pts',(-5.11311782178954,-4.43654275986957,
109.530303990407));
#36199=CARTESIAN_POINT('Ctrl Pts',(-4.98740459172177,-4.57362924147472,
109.53905322692));
#36200=CARTESIAN_POINT('Ctrl Pts',(-4.86169180911002,-4.71071523514258,
109.547802432291));
#36201=CARTESIAN_POINT('Ctrl Pts',(-4.73032391415613,-4.84261509316346,
109.556551637662));
#36202=CARTESIAN_POINT('Ctrl Pts',(-4.59374707237484,-4.96888084331347,
109.565300843033));
#36203=CARTESIAN_POINT('Ctrl Pts',(-4.45717070537614,-5.09514615452538,
109.57405001799));
#36204=CARTESIAN_POINT('Ctrl Pts',(-4.31538563819742,-5.21577720253439,
109.582799192946));
#36205=CARTESIAN_POINT('Ctrl Pts',(-4.16887341290903,-5.3303642902845,109.591548367902));
#36206=CARTESIAN_POINT('Ctrl Pts',(-4.02236168477599,-5.44495098920984,
109.60029751317));
#36207=CARTESIAN_POINT('Ctrl Pts',(-3.87112305634705,-5.55349359238573,
109.609046658438));
#36208=CARTESIAN_POINT('Ctrl Pts',(-3.71567117317003,-5.65562346102295,
109.617795803706));
#36209=CARTESIAN_POINT('Ctrl Pts',(-3.56021980457579,-5.75775299158597,
109.626544920012));
#36210=CARTESIAN_POINT('Ctrl Pts',(-3.40055544862674,-5.85346967275187,
109.635294036318));
#36211=CARTESIAN_POINT('Ctrl Pts',(-3.23722036323697,-5.94244842803401,
109.644043152624));
#36212=CARTESIAN_POINT('Ctrl Pts',(-3.07388580496369,-6.0314268961631,109.652792240695));
#36213=CARTESIAN_POINT('Ctrl Pts',(-2.90688079258058,-6.11366734484655,
109.661541328766));
#36214=CARTESIAN_POINT('Ctrl Pts',(-2.73677251094995,-6.18889046787134,
109.670290416837));
#36215=CARTESIAN_POINT('Ctrl Pts',(-2.5666647641705,-6.26411335438104,109.679039477399));
#36216=CARTESIAN_POINT('Ctrl Pts',(-2.39345402972522,-6.33231884350128,
109.687788537962));
#36217=CARTESIAN_POINT('Ctrl Pts',(-2.21772856474491,-6.39327529620886,
109.696537598524));
#36218=CARTESIAN_POINT('Ctrl Pts',(-2.04200363768733,-6.45423156231935,
109.705286632304));
#36219=CARTESIAN_POINT('Ctrl Pts',(-1.86376426620566,-6.5079387425192,109.714035666084));
#36220=CARTESIAN_POINT('Ctrl Pts',(-1.68361578195171,-6.55421443795999,
109.722784699864));
#36221=CARTESIAN_POINT('Ctrl Pts',(-1.50346783420376,-6.60048999558563,
109.731533707588));
#36222=CARTESIAN_POINT('Ctrl Pts',(-1.3214110625778,-6.63933404145389,109.740282715312));
#36223=CARTESIAN_POINT('Ctrl Pts',(-1.13806375959602,-6.67061465526935,
109.749031723036));
#36224=CARTESIAN_POINT('Ctrl Pts',(-0.954716987424667,-6.70189517852402,
109.757780705431));
#36225=CARTESIAN_POINT('Ctrl Pts',(-0.770079973815318,-6.72561226535766,
109.766529687826));
#36226=CARTESIAN_POINT('Ctrl Pts',(-0.58477977055782,-6.74168536939736,
109.775278670221));
#36227=CARTESIAN_POINT('Ctrl Pts',(-0.391490647559245,-6.75845143942363,
109.784404850897));
#36228=CARTESIAN_POINT('Ctrl Pts',(-0.197480213109634,-6.76689975924011,
109.793531031573));
#36229=CARTESIAN_POINT('Ctrl Pts',(-0.00346532630305276,-6.76699911271707,
109.802657212249));
#36230=CARTESIAN_POINT('Ctrl Pts',(0.184486595290791,-6.76709536139788,
109.811498199779));
#36231=CARTESIAN_POINT('Ctrl Pts',(0.372442378179965,-6.75935659726799,
109.820339187309));
#36232=CARTESIAN_POINT('Ctrl Pts',(0.559750217716826,-6.7438096572906,109.829180174839));
#36233=CARTESIAN_POINT('Ctrl Pts',(0.745129914452536,-6.72842275717311,
109.837930153437));
#36234=CARTESIAN_POINT('Ctrl Pts',(0.929874656309014,-6.70538772273545,
109.846680132035));
#36235=CARTESIAN_POINT('Ctrl Pts',(1.11335688289266,-6.67478280180828,109.855430110632));
#36236=CARTESIAN_POINT('Ctrl Pts',(1.2968372311835,-6.64417819418122,109.864179999657));
#36237=CARTESIAN_POINT('Ctrl Pts',(1.47905480729734,-6.60600390230188,109.872929888682));
#36238=CARTESIAN_POINT('Ctrl Pts',(1.65939064804312,-6.5603895979726,109.881679777707));
#36239=CARTESIAN_POINT('Ctrl Pts',(1.83972470263769,-6.51477574543396,109.890429580068));
#36240=CARTESIAN_POINT('Ctrl Pts',(2.01817678125352,-6.46172209820255,109.899179382429));
#36241=CARTESIAN_POINT('Ctrl Pts',(2.19414072347184,-6.40140886724184,109.90792918479));
#36242=CARTESIAN_POINT('Ctrl Pts',(2.37010298131603,-6.34109621361559,109.916678903395));
#36243=CARTESIAN_POINT('Ctrl Pts',(2.54357687926423,-6.2735242082617,109.925428622001));
#36244=CARTESIAN_POINT('Ctrl Pts',(2.71397317789485,-6.1989223732571,109.934178340606));
#36245=CARTESIAN_POINT('Ctrl Pts',(2.88436790206728,-6.12432122757187,109.942927978365));
#36246=CARTESIAN_POINT('Ctrl Pts',(3.05168482125797,-6.04269049717649,109.951677616123));
#36247=CARTESIAN_POINT('Ctrl Pts',(3.21535561996943,-5.9543074523517,109.960427253881));
#36248=CARTESIAN_POINT('Ctrl Pts',(3.37902496074832,-5.86592519481775,109.9691768137));
#36249=CARTESIAN_POINT('Ctrl Pts',(3.53904799384424,-5.77079087940508,109.977926373519));
#36250=CARTESIAN_POINT('Ctrl Pts',(3.69488118814532,-5.66922763747319,109.986675933338));
#36251=CARTESIAN_POINT('Ctrl Pts',(3.85071304610394,-5.56766526649356,109.995425418126));
#36252=CARTESIAN_POINT('Ctrl Pts',(4.00235489705542,-5.45967423581026,110.004174902913));
#36253=CARTESIAN_POINT('Ctrl Pts',(4.14929168607241,-5.34562133936649,110.012924387701));
#36254=CARTESIAN_POINT('Ctrl Pts',(4.29622726385356,-5.23156938308861,110.021673800364));
#36255=CARTESIAN_POINT('Ctrl Pts',(4.43845763091677,-5.11145583677541,110.030423213027));
#36256=CARTESIAN_POINT('Ctrl Pts',(4.57549970660584,-4.98568866204558,110.039172625691));
#36257=CARTESIAN_POINT('Ctrl Pts',(4.71254069814922,-4.85992248226523,110.047921969137));
#36258=CARTESIAN_POINT('Ctrl Pts',(4.84439326930947,-4.72850295734378,110.056671312583));
#36259=CARTESIAN_POINT('Ctrl Pts',(4.97060959434338,-4.59187644222072,110.06542065603));
#36260=CARTESIAN_POINT('Ctrl Pts',(5.09682496280164,-4.45525096257066,110.074169933166));
#36261=CARTESIAN_POINT('Ctrl Pts',(5.21740397615497,-4.31341878218739,110.082919210302));
#36262=CARTESIAN_POINT('Ctrl Pts',(5.33193710451602,-4.16686161439102,110.091668487438));
#36263=CARTESIAN_POINT('Ctrl Pts',(5.44646940289061,-4.0203055086495,110.100417701171));
#36264=CARTESIAN_POINT('Ctrl Pts',(5.55495572749354,-3.8690247098058,110.109166914904));
#36265=CARTESIAN_POINT('Ctrl Pts',(5.65702762491156,-3.71353301466239,110.117916128637));
#36266=CARTESIAN_POINT('Ctrl Pts',(5.7590988165487,-3.55804239467354,110.126665281873));
#36267=CARTESIAN_POINT('Ctrl Pts',(5.85475551250514,-3.39834117620016,110.135414435109));
#36268=CARTESIAN_POINT('Ctrl Pts',(5.94367283727842,-3.23497174692434,110.144163588346));
#36269=CARTESIAN_POINT('Ctrl Pts',(6.03258957676081,-3.0716033930142,110.152912683991));
#36270=CARTESIAN_POINT('Ctrl Pts',(6.11476689685075,-2.90456712829946,110.161661779637));
#36271=CARTESIAN_POINT('Ctrl Pts',(6.18992570525071,-2.73443024476334,110.170410875282));
#36272=CARTESIAN_POINT('Ctrl Pts',(6.26508404388529,-2.56429442463443,110.179159916243));
#36273=CARTESIAN_POINT('Ctrl Pts',(6.33322384283166,-2.3910582865639,110.187908957204));
#36274=CARTESIAN_POINT('Ctrl Pts',(6.39411368719901,-2.21531017132461,110.196657998165));
#36275=CARTESIAN_POINT('Ctrl Pts',(6.45500317120764,-2.03956309619911,110.205406987348));
#36276=CARTESIAN_POINT('Ctrl Pts',(6.50864269269955,-1.86130434439045,110.21415597653));
#36277=CARTESIAN_POINT('Ctrl Pts',(6.55485008446224,-1.68113930720372,110.222904965713));
#36278=CARTESIAN_POINT('Ctrl Pts',(6.60199664749308,-1.49731239212262,110.231831779242));
#36279=CARTESIAN_POINT('Ctrl Pts',(6.64140563640825,-1.31150116500087,110.240758592771));
#36280=CARTESIAN_POINT('Ctrl Pts',(6.67293772282103,-1.1243625515607,110.249685406301));
#36281=CARTESIAN_POINT('Ctrl Pts',(6.70384494949815,-0.940932395055363,
110.258435320456));
#36282=CARTESIAN_POINT('Ctrl Pts',(6.72718449348886,-0.756227260510651,
110.267185234612));
#36283=CARTESIAN_POINT('Ctrl Pts',(6.742877073739,-0.570874564545538,110.275935148767));
#36284=CARTESIAN_POINT('Ctrl Pts',(6.75856934538648,-0.385525513636381,
110.284684890851));
#36285=CARTESIAN_POINT('Ctrl Pts',(6.76661493004091,-0.199529212422189,
110.293434632935));
#36286=CARTESIAN_POINT('Ctrl Pts',(6.76698649908906,-0.013517438604437,
110.302184375019));
#36287=CARTESIAN_POINT('Ctrl Pts',(6.767358061324,0.172490924441749,110.310933956665));
#36288=CARTESIAN_POINT('Ctrl Pts',(6.76005588896311,0.358514472897364,110.319683538311));
#36289=CARTESIAN_POINT('Ctrl Pts',(6.74510478454617,0.543921359658159,110.328433119957));
#36290=CARTESIAN_POINT('Ctrl Pts',(6.73015393440731,0.729325093146488,110.337182552796));
#36291=CARTESIAN_POINT('Ctrl Pts',(6.7075544355695,0.914111900252494,110.345931985635));
#36292=CARTESIAN_POINT('Ctrl Pts',(6.6773830468238,1.09765415591163,110.354681418474));
#36293=CARTESIAN_POINT('Ctrl Pts',(6.64721213111933,1.28119353390898,110.363430714135));
#36294=CARTESIAN_POINT('Ctrl Pts',(6.60946960955577,1.46348811672278,110.372180009797));
#36295=CARTESIAN_POINT('Ctrl Pts',(6.56428366991276,1.64391876347848,110.380929305458));
#36296=CARTESIAN_POINT('Ctrl Pts',(6.51909837867821,1.82434682109345,110.389678475569));
#36297=CARTESIAN_POINT('Ctrl Pts',(6.46646995272035,2.00291071820077,110.39842764568));
#36298=CARTESIAN_POINT('Ctrl Pts',(6.40657713281673,2.1790040021234,110.40717681579));
#36299=CARTESIAN_POINT('Ctrl Pts',(6.34668509279197,2.35509499309288,110.415925871976));
#36300=CARTESIAN_POINT('Ctrl Pts',(6.27952894037677,2.52871516397746,110.424674928162));
#36301=CARTESIAN_POINT('Ctrl Pts',(6.20533675061613,2.69927486771038,110.433423984348));
#36302=CARTESIAN_POINT('Ctrl Pts',(6.12832117908086,2.87632521635563,110.44250598563));
#36303=CARTESIAN_POINT('Ctrl Pts',(6.04372366626251,3.05007728919657,110.451587986912));
#36304=CARTESIAN_POINT('Ctrl Pts',(5.95185378008041,3.21989527477876,110.460669988195));
#36305=CARTESIAN_POINT('Ctrl Pts',(5.86334450817554,3.38350129286435,110.469419768502));
#36306=CARTESIAN_POINT('Ctrl Pts',(5.76808562057448,3.54345567124649,110.478169548809));
#36307=CARTESIAN_POINT('Ctrl Pts',(5.66640068804685,3.69921508465001,110.486919329116));
#36308=CARTESIAN_POINT('Ctrl Pts',(5.56471941108135,3.85496889851977,110.495668794869));
#36309=CARTESIAN_POINT('Ctrl Pts',(5.45661270815336,4.00652780919334,110.504418260623));
#36310=CARTESIAN_POINT('Ctrl Pts',(5.34244776449347,4.1533770456893,110.513167726376));
#36311=CARTESIAN_POINT('Ctrl Pts',(5.22828631819835,4.30022178355958,110.521916924096));
#36312=CARTESIAN_POINT('Ctrl Pts',(5.10806717844316,4.44235690972396,110.530666121816));
#36313=CARTESIAN_POINT('Ctrl Pts',(4.98219864544972,4.5792996907037,110.539415319535));
#36314=CARTESIAN_POINT('Ctrl Pts',(4.85633329944276,4.71623900429743,110.548164295725));
#36315=CARTESIAN_POINT('Ctrl Pts',(4.72481904033896,4.84798602483376,110.556913271916));
#36316=CARTESIAN_POINT('Ctrl Pts',(4.58810250737442,4.97409332258901,110.565662248106));
#36317=CARTESIAN_POINT('Ctrl Pts',(4.45137708685884,5.10020881821924,110.574411793042));
#36318=CARTESIAN_POINT('Ctrl Pts',(4.30944892636291,5.22068366307735,110.583161337978));
#36319=CARTESIAN_POINT('Ctrl Pts',(4.16280009466898,5.33510865604666,110.591910882914));
#36320=CARTESIAN_POINT('Ctrl Pts',(4.01615988349045,5.44952692272702,110.600659913523));
#36321=CARTESIAN_POINT('Ctrl Pts',(3.86479978232507,5.55789587288433,110.609408944131));
#36322=CARTESIAN_POINT('Ctrl Pts',(3.70923383581365,5.65984746713683,110.618157974739));
#36323=CARTESIAN_POINT('Ctrl Pts',(3.55366577799854,5.76180044505189,110.626907124087));
#36324=CARTESIAN_POINT('Ctrl Pts',(3.3938920002717,5.85733573570867,110.635656273435));
#36325=CARTESIAN_POINT('Ctrl Pts',(3.23045513626388,5.94612887621739,110.644405422783));
#36326=CARTESIAN_POINT('Ctrl Pts',(3.18695122151813,5.96976399206564,110.646734286896));
#36327=CARTESIAN_POINT('Ctrl Pts',(3.14318791262785,5.9929216543527,110.649063151009));
#36328=CARTESIAN_POINT('Ctrl Pts',(3.09917575053264,6.01559628526636,110.651392015122));
#36329=CARTESIAN_POINT('Origin',(0.,0.,-3.69717978381041));
#36330=CARTESIAN_POINT('',(3.09917575053268,6.01559628526634,113.045920956904));
#36331=CARTESIAN_POINT('',(3.09917575053259,6.01559628526639,112.651392015122));
#36332=CARTESIAN_POINT('',(3.09917575053259,6.01559628526639,-3.69717978381041));
#36333=CARTESIAN_POINT('',(-6.76699984597165,0.00144382119762321,111.697179783846));
#36334=CARTESIAN_POINT('Ctrl Pts',(-6.76699984597165,0.00144382119763222,
111.697179783846));
#36335=CARTESIAN_POINT('Ctrl Pts',(-6.76703761583499,-0.175578555110342,
111.705544669951));
#36336=CARTESIAN_POINT('Ctrl Pts',(-6.76012485488847,-0.352817258443799,
111.713909556056));
#36337=CARTESIAN_POINT('Ctrl Pts',(-6.74623679069683,-0.529696293972878,
111.722274442161));
#36338=CARTESIAN_POINT('Ctrl Pts',(-6.7323648860999,-0.706369520147311,
111.73062959522));
#36339=CARTESIAN_POINT('Ctrl Pts',(-6.71153387447242,-0.882683574078368,
111.738984748279));
#36340=CARTESIAN_POINT('Ctrl Pts',(-6.68377098569768,-1.05806162899233,
111.747339901339));
#36341=CARTESIAN_POINT('Ctrl Pts',(-6.65604385526244,-1.23321379862183,
111.755684293039));
#36342=CARTESIAN_POINT('Ctrl Pts',(-6.62140270326974,-1.40743203735987,
111.76402868474));
#36343=CARTESIAN_POINT('Ctrl Pts',(-6.57992658499906,-1.58014402382271,
111.77237307644));
#36344=CARTESIAN_POINT('Ctrl Pts',(-6.53848165704011,-1.75272612974412,
111.780711193104));
#36345=CARTESIAN_POINT('Ctrl Pts',(-6.49021208107389,-1.92380390897833,
111.789049309767));
#36346=CARTESIAN_POINT('Ctrl Pts',(-6.43524822976081,-2.09281370918684,
111.797387426431));
#36347=CARTESIAN_POINT('Ctrl Pts',(-6.38032466717979,-2.26169962450751,
111.80571943122));
#36348=CARTESIAN_POINT('Ctrl Pts',(-6.31871671730963,-2.42852025879494,
111.814051436009));
#36349=CARTESIAN_POINT('Ctrl Pts',(-6.25060500568759,-2.59272560500977,
111.822383440798));
#36350=CARTESIAN_POINT('Ctrl Pts',(-6.21804693548716,-2.67121738068288,
111.826366221298));
#36351=CARTESIAN_POINT('Ctrl Pts',(-6.1840035340459,-2.74911179372773,111.830349001797));
#36352=CARTESIAN_POINT('Ctrl Pts',(-6.14849852039715,-2.82635011006671,
111.834331782297));
#36353=CARTESIAN_POINT('Ctrl Pts',(-6.0718749796016,-2.99303849220699,111.842927040057));
#36354=CARTESIAN_POINT('Ctrl Pts',(-5.988514174124,-3.15651090180509,111.851522297817));
#36355=CARTESIAN_POINT('Ctrl Pts',(-5.89871943339522,-3.31623250784465,
111.860117555577));
#36356=CARTESIAN_POINT('Ctrl Pts',(-5.8088406036998,-3.47610368639473,111.868720862432));
#36357=CARTESIAN_POINT('Ctrl Pts',(-5.71251596204545,-3.63221678419541,
111.877324169286));
#36358=CARTESIAN_POINT('Ctrl Pts',(-5.61009279203003,-3.78406499214967,
111.88592747614));
#36359=CARTESIAN_POINT('Ctrl Pts',(-5.50342312186914,-3.94220887946116,
111.89488747908));
#36360=CARTESIAN_POINT('Ctrl Pts',(-5.39013867774819,-4.09572638509883,
111.90384748202));
#36361=CARTESIAN_POINT('Ctrl Pts',(-5.27067803046966,-4.24408318711173,
111.91280748496));
#36362=CARTESIAN_POINT('Ctrl Pts',(-5.15565928771743,-4.38692363905136,
111.921434328165));
#36363=CARTESIAN_POINT('Ctrl Pts',(-5.03491558889029,-4.52498005563022,
111.93006117137));
#36364=CARTESIAN_POINT('Ctrl Pts',(-4.90887633273898,-4.65781302221065,
111.938688014575));
#36365=CARTESIAN_POINT('Ctrl Pts',(-4.78271661491865,-4.79077294352998,
111.947323102861));
#36366=CARTESIAN_POINT('Ctrl Pts',(-4.65125145363274,-4.91849923518474,
111.955958191147));
#36367=CARTESIAN_POINT('Ctrl Pts',(-4.51494522387686,-5.0405910988089,111.964593279433));
#36368=CARTESIAN_POINT('Ctrl Pts',(-4.37843655201575,-5.16286429335205,
111.973241192559));
#36369=CARTESIAN_POINT('Ctrl Pts',(-4.23707267610891,-5.27948613977851,
111.981889105684));
#36370=CARTESIAN_POINT('Ctrl Pts',(-4.09135014666724,-5.39009675027879,
111.990537018809));
#36371=CARTESIAN_POINT('Ctrl Pts',(-4.075002297227,-5.40250557692955,111.991507183013));
#36372=CARTESIAN_POINT('Ctrl Pts',(-4.05859962102883,-5.41483879531184,
111.992477347216));
#36373=CARTESIAN_POINT('Ctrl Pts',(-4.04214284049685,-5.42709593217405,
111.99344751142));
#36374=CARTESIAN_POINT('Ctrl Pts',(-3.90262857552527,-5.5310072310252,112.001672190939));
#36375=CARTESIAN_POINT('Ctrl Pts',(-3.75892101225209,-5.62967227570346,
112.009896870458));
#36376=CARTESIAN_POINT('Ctrl Pts',(-3.61145150334582,-5.7227359749495,112.018121549977));
#36377=CARTESIAN_POINT('Ctrl Pts',(-3.46413700157703,-5.81570185371909,
112.026337584427));
#36378=CARTESIAN_POINT('Ctrl Pts',(-3.31306872905993,-5.90307792174032,
112.034553618877));
#36379=CARTESIAN_POINT('Ctrl Pts',(-3.15870995610597,-5.98455014292612,
112.042769653327));
#36380=CARTESIAN_POINT('Ctrl Pts',(-3.00448251335135,-6.06595304661966,
112.050978697482));
#36381=CARTESIAN_POINT('Ctrl Pts',(-2.84697046107697,-6.14146194113349,
112.059187741636));
#36382=CARTESIAN_POINT('Ctrl Pts',(-2.6866648930447,-6.21080677146545,112.067396785791));
#36383=CARTESIAN_POINT('Ctrl Pts',(-2.52646361439533,-6.28010648839524,
112.075600489419));
#36384=CARTESIAN_POINT('Ctrl Pts',(-2.36347276780517,-6.3432499871764,112.083804193047));
#36385=CARTESIAN_POINT('Ctrl Pts',(-2.19820690746325,-6.40001370248384,
112.092007896675));
#36386=CARTESIAN_POINT('Ctrl Pts',(-2.03301547653896,-6.45675185358664,
112.100207905669));
#36387=CARTESIAN_POINT('Ctrl Pts',(-1.86555141138387,-6.5071158292534,112.108407914663));
#36388=CARTESIAN_POINT('Ctrl Pts',(-1.69634813750132,-6.55093062063672,
112.116607923657));
#36389=CARTESIAN_POINT('Ctrl Pts',(-1.52715839346855,-6.59474190849714,
112.124807276961));
#36390=CARTESIAN_POINT('Ctrl Pts',(-1.35623006223046,-6.63200495693902,
112.133006630265));
#36391=CARTESIAN_POINT('Ctrl Pts',(-1.18411095100026,-6.66259485904113,
112.141205983568));
#36392=CARTESIAN_POINT('Ctrl Pts',(-1.01199296193552,-6.69318456170617,
112.149405283415));
#36393=CARTESIAN_POINT('Ctrl Pts',(-0.838684561136643,-6.7171011408871,
112.157604583262));
#36394=CARTESIAN_POINT('Ctrl Pts',(-0.66474283020421,-6.73427100506745,
112.165803883108));
#36395=CARTESIAN_POINT('Ctrl Pts',(-0.490770678583724,-6.75144387208719,
112.174004616931));
#36396=CARTESIAN_POINT('Ctrl Pts',(-0.316165332940904,-6.76186763806699,
112.182205350754));
#36397=CARTESIAN_POINT('Ctrl Pts',(-0.141488122766108,-6.76552068292723,
112.190406084577));
#36398=CARTESIAN_POINT('Ctrl Pts',(0.0332513252284336,-6.76917502937426,
112.198609740337));
#36399=CARTESIAN_POINT('Ctrl Pts',(0.208062330549596,-6.76605384154532,
112.206813396097));
#36400=CARTESIAN_POINT('Ctrl Pts',(0.382384382500243,-6.75618762202619,
112.215017051857));
#36401=CARTESIAN_POINT('Ctrl Pts',(0.556906131567837,-6.74631010011835,
112.223230105432));
#36402=CARTESIAN_POINT('Ctrl Pts',(0.730937449902314,-6.72967212972754,
112.231443159007));
#36403=CARTESIAN_POINT('Ctrl Pts',(0.903922692723735,-6.70635614664022,
112.239656212582));
#36404=CARTESIAN_POINT('Ctrl Pts',(1.07701029479464,-6.68302636696256,112.247874126005));
#36405=CARTESIAN_POINT('Ctrl Pts',(1.24905023488409,-6.65301075922937,112.256092039428));
#36406=CARTESIAN_POINT('Ctrl Pts',(1.41949797321629,-6.61644273790946,112.264309952851));
#36407=CARTESIAN_POINT('Ctrl Pts',(1.5902115525251,-6.57981768281136,112.272540683447));
#36408=CARTESIAN_POINT('Ctrl Pts',(1.75932762023771,-6.53661987976473,112.280771414043));
#36409=CARTESIAN_POINT('Ctrl Pts',(1.92631638239284,-6.48703277276483,112.289002144639));
#36410=CARTESIAN_POINT('Ctrl Pts',(2.07967558896,-6.4414929454895,112.296561086315));
#36411=CARTESIAN_POINT('Ctrl Pts',(2.23124058478261,-6.39056488042854,112.304120027991));
#36412=CARTESIAN_POINT('Ctrl Pts',(2.3806174150803,-6.33442576111019,112.311678969667));
#36413=CARTESIAN_POINT('Ctrl Pts',(2.54175142281211,-6.27386803426412,112.319832861834));
#36414=CARTESIAN_POINT('Ctrl Pts',(2.70083718573265,-6.20705874728179,112.327986754001));
#36415=CARTESIAN_POINT('Ctrl Pts',(2.85734834524032,-6.13415433731109,112.336140646167));
#36416=CARTESIAN_POINT('Ctrl Pts',(3.01366851740659,-6.06133889108892,112.344284588308));
#36417=CARTESIAN_POINT('Ctrl Pts',(3.16742001207413,-5.98244327961086,112.352428530448));
#36418=CARTESIAN_POINT('Ctrl Pts',(3.31809247529859,-5.8976733823913,112.360572472588));
#36419=CARTESIAN_POINT('Ctrl Pts',(3.46861278957044,-5.81298908575728,112.368708190981));
#36420=CARTESIAN_POINT('Ctrl Pts',(3.61605994593148,-5.72244249047124,112.376843909374));
#36421=CARTESIAN_POINT('Ctrl Pts',(3.75994440948221,-5.62628714496545,112.384979627767));
#36422=CARTESIAN_POINT('Ctrl Pts',(3.90371384472922,-5.53020867076331,112.393108842067));
#36423=CARTESIAN_POINT('Ctrl Pts',(4.0439259556214,-5.42853057649233,112.401238056367));
#36424=CARTESIAN_POINT('Ctrl Pts',(4.18011663927345,-5.32155183025302,112.409367270667));
#36425=CARTESIAN_POINT('Ctrl Pts',(4.31622708118886,-5.21463611446596,112.417491695343));
#36426=CARTESIAN_POINT('Ctrl Pts',(4.44832052754707,-5.10242619148798,112.425616120018));
#36427=CARTESIAN_POINT('Ctrl Pts',(4.57596267173852,-4.98526374697023,112.433740544694));
#36428=CARTESIAN_POINT('Ctrl Pts',(4.70437968545728,-4.86739005141094,112.441914289828));
#36429=CARTESIAN_POINT('Ctrl Pts',(4.82829086358383,-4.74450371615169,112.450088034962));
#36430=CARTESIAN_POINT('Ctrl Pts',(4.9472880835852,-4.61699356919802,112.458261780096));
#36431=CARTESIAN_POINT('Ctrl Pts',(5.0655232802109,-4.49029995991316,112.466383182958));
#36432=CARTESIAN_POINT('Ctrl Pts',(5.17890703408709,-4.35904187130088,112.47450458582));
#36433=CARTESIAN_POINT('Ctrl Pts',(5.28707657463593,-4.22363709306754,112.482625988683));
#36434=CARTESIAN_POINT('Ctrl Pts',(5.39525447828405,-4.08822184604976,112.490748019449));
#36435=CARTESIAN_POINT('Ctrl Pts',(5.49821713712489,-3.94865955672577,112.498870050215));
#36436=CARTESIAN_POINT('Ctrl Pts',(5.59564276395386,-3.80540024941016,112.506992080981));
#36437=CARTESIAN_POINT('Ctrl Pts',(5.69309447530815,-3.66210258615933,112.515116286323));
#36438=CARTESIAN_POINT('Ctrl Pts',(5.78500599705682,-3.51510623649389,112.523240491664));
#36439=CARTESIAN_POINT('Ctrl Pts',(5.87109950772212,-3.36488923598164,112.531364697005));
#36440=CARTESIAN_POINT('Ctrl Pts',(5.95812492106859,-3.21304624038041,112.539576841247));
#36441=CARTESIAN_POINT('Ctrl Pts',(6.03920544410244,-3.05791279641549,112.54778898549));
#36442=CARTESIAN_POINT('Ctrl Pts',(6.11410274967759,-2.90000630454228,112.556001129732));
#36443=CARTESIAN_POINT('Ctrl Pts',(6.18831632540041,-2.74354132490426,112.564138306149));
#36444=CARTESIAN_POINT('Ctrl Pts',(6.25645901989143,-2.58435407734079,112.572275482565));
#36445=CARTESIAN_POINT('Ctrl Pts',(6.31834833973038,-2.42296579790684,112.580412658982));
#36446=CARTESIAN_POINT('Ctrl Pts',(6.38109293924895,-2.25934721256086,112.588662287137));
#36447=CARTESIAN_POINT('Ctrl Pts',(6.4374099351969,-2.09346668712922,112.596911915292));
#36448=CARTESIAN_POINT('Ctrl Pts',(6.48716221335219,-1.92588042662453,112.605161543448));
#36449=CARTESIAN_POINT('Ctrl Pts',(6.53691449150748,-1.75829416611984,112.613411171603));
#36450=CARTESIAN_POINT('Ctrl Pts',(6.58010201805447,-1.58900255901556,112.621660799759));
#36451=CARTESIAN_POINT('Ctrl Pts',(6.61664193296375,-1.41856918440578,112.629910427914));
#36452=CARTESIAN_POINT('Ctrl Pts',(6.65307217677808,-1.24864734943308,112.638135295592));
#36453=CARTESIAN_POINT('Ctrl Pts',(6.68300371998199,-1.07708271244946,112.646360163269));
#36454=CARTESIAN_POINT('Ctrl Pts',(6.70628996835202,-0.904413545000902,
112.654585030947));
#36455=CARTESIAN_POINT('Ctrl Pts',(6.72954998215683,-0.731938908696387,
112.66280063239));
#36456=CARTESIAN_POINT('Ctrl Pts',(6.74617956147946,-0.558362572109245,
112.671016233834));
#36457=CARTESIAN_POINT('Ctrl Pts',(6.75608261991125,-0.384235127146414,
112.679231835277));
#36458=CARTESIAN_POINT('Ctrl Pts',(6.76597651116243,-0.210268870542459,
112.687439831606));
#36459=CARTESIAN_POINT('Ctrl Pts',(6.76915626185056,-0.0357528774845146,
112.695647827934));
#36460=CARTESIAN_POINT('Ctrl Pts',(6.76557729125571,0.138754877553961,112.703855824262));
#36461=CARTESIAN_POINT('Ctrl Pts',(6.76200091482999,0.313136142972685,112.712057871133));
#36462=CARTESIAN_POINT('Ctrl Pts',(6.75167558226842,0.487508825024241,112.720259918005));
#36463=CARTESIAN_POINT('Ctrl Pts',(6.73460872451394,0.661312579421232,112.728461964876));
#36464=CARTESIAN_POINT('Ctrl Pts',(6.71755081026585,0.83502525583471,112.736659713648));
#36465=CARTESIAN_POINT('Ctrl Pts',(6.69375844359767,1.00816924231583,112.744857462419));
#36466=CARTESIAN_POINT('Ctrl Pts',(6.66329107632034,1.18018686326773,112.753055211191));
#36467=CARTESIAN_POINT('Ctrl Pts',(6.63282952008147,1.35217167531291,112.761251396407));
#36468=CARTESIAN_POINT('Ctrl Pts',(6.59569555551616,1.52303019574673,112.769447581622));
#36469=CARTESIAN_POINT('Ctrl Pts',(6.55200021529622,1.69221221445727,112.777643766838));
#36470=CARTESIAN_POINT('Ctrl Pts',(6.50830810755886,1.86138171746414,112.785839345718));
#36471=CARTESIAN_POINT('Ctrl Pts',(6.45805567970994,2.0288746180972,112.794034924599));
#36472=CARTESIAN_POINT('Ctrl Pts',(6.40140456973998,2.19415326139997,112.802230503479));
#36473=CARTESIAN_POINT('Ctrl Pts',(6.34474734369284,2.3594497482532,112.810426967157));
#36474=CARTESIAN_POINT('Ctrl Pts',(6.28169017560345,2.52253116199824,112.818623430836));
#36475=CARTESIAN_POINT('Ctrl Pts',(6.212443850371,2.68287726256488,112.826819894514));
#36476=CARTESIAN_POINT('Ctrl Pts',(6.14317745067534,2.84326984735842,112.835018734342));
#36477=CARTESIAN_POINT('Ctrl Pts',(6.06771846218382,3.00092521014654,112.84321757417));
#36478=CARTESIAN_POINT('Ctrl Pts',(5.98632488021125,3.15534521543425,112.851416413998));
#36479=CARTESIAN_POINT('Ctrl Pts',(5.90484628032631,3.30992651681139,112.859623817747));
#36480=CARTESIAN_POINT('Ctrl Pts',(5.81742087000417,3.46126539118293,112.867831221496));
#36481=CARTESIAN_POINT('Ctrl Pts',(5.72435199260824,3.60888947804198,112.876038625245));
#36482=CARTESIAN_POINT('Ctrl Pts',(5.63123326259646,3.75659264017408,112.884250425314));
#36483=CARTESIAN_POINT('Ctrl Pts',(5.53246524198986,3.90057675237968,112.892462225383));
#36484=CARTESIAN_POINT('Ctrl Pts',(5.42839323009073,4.0404004677142,112.900674025452));
#36485=CARTESIAN_POINT('Ctrl Pts',(5.3241680096483,4.180430023095,112.908897914438));
#36486=CARTESIAN_POINT('Ctrl Pts',(5.21462341864902,4.31628666225212,112.917121803425));
#36487=CARTESIAN_POINT('Ctrl Pts',(5.10014431995143,4.44756303110672,112.925345692411));
#36488=CARTESIAN_POINT('Ctrl Pts',(4.99436761184972,4.56886012644521,112.932944423661));
#36489=CARTESIAN_POINT('Ctrl Pts',(4.88437866718782,4.68624708505496,112.940543154911));
#36490=CARTESIAN_POINT('Ctrl Pts',(4.7705069549644,4.79943250735296,112.948141886161));
#36491=CARTESIAN_POINT('Ctrl Pts',(4.64726925939531,4.92192746543924,112.956365615393));
#36492=CARTESIAN_POINT('Ctrl Pts',(4.51913753642527,5.03984460659206,112.964589344625));
#36493=CARTESIAN_POINT('Ctrl Pts',(4.38648522069382,5.15276978028659,112.972813073857));
#36494=CARTESIAN_POINT('Ctrl Pts',(4.25396400993284,5.26558334604212,112.981028675286));
#36495=CARTESIAN_POINT('Ctrl Pts',(4.11693136867661,5.37341453291452,112.989244276716));
#36496=CARTESIAN_POINT('Ctrl Pts',(3.97579855336091,5.47588484750121,112.997459878146));
#36497=CARTESIAN_POINT('Ctrl Pts',(3.83481094650602,5.57824973262681,113.005667026723));
#36498=CARTESIAN_POINT('Ctrl Pts',(3.68973185875539,5.67526452497526,113.013874175301));
#36499=CARTESIAN_POINT('Ctrl Pts',(3.54100646168675,5.76659017429648,113.022081323878));
#36500=CARTESIAN_POINT('Ctrl Pts',(3.39700359011511,5.85501593082232,113.03002786822));
#36501=CARTESIAN_POINT('Ctrl Pts',(3.24958270126473,5.93810811080855,113.037974412562));
#36502=CARTESIAN_POINT('Ctrl Pts',(3.09917575053269,6.01559628526634,113.045920956904));
#36503=CARTESIAN_POINT('Ctrl Pts',(3.09917575053272,6.01559628526632,111.045835064059));
#36504=CARTESIAN_POINT('Ctrl Pts',(2.94599616846457,6.09451289198494,111.053983127627));
#36505=CARTESIAN_POINT('Ctrl Pts',(2.78957094525295,6.16769307570725,111.062131191196));
#36506=CARTESIAN_POINT('Ctrl Pts',(2.63037268791528,6.23485593439571,111.070279254764));
#36507=CARTESIAN_POINT('Ctrl Pts',(2.47134965376088,6.30194486959974,111.078418350083));
#36508=CARTESIAN_POINT('Ctrl Pts',(2.3095599951337,6.36302952309325,111.086557445403));
#36509=CARTESIAN_POINT('Ctrl Pts',(2.14550169665552,6.41787437315879,111.094696540722));
#36510=CARTESIAN_POINT('Ctrl Pts',(1.98158945302321,6.47267039694612,111.102828390115));
#36511=CARTESIAN_POINT('Ctrl Pts',(1.81541293534023,6.52123756183,111.110960239508));
#36512=CARTESIAN_POINT('Ctrl Pts',(1.64749092867358,6.56338804581432,111.119092088902));
#36513=CARTESIAN_POINT('Ctrl Pts',(1.47968310346446,6.60550986885185,111.127218408904));
#36514=CARTESIAN_POINT('Ctrl Pts',(1.31013250607494,6.6412236103714,111.135344728906));
#36515=CARTESIAN_POINT('Ctrl Pts',(1.13937393368256,6.67039099597953,111.143471048909));
#36516=CARTESIAN_POINT('Ctrl Pts',(0.968695573767828,6.69954468044086,111.151593551637));
#36517=CARTESIAN_POINT('Ctrl Pts',(0.79681072883332,6.7221580720476,111.159716054365));
#36518=CARTESIAN_POINT('Ctrl Pts',(0.624265257620319,6.7381438013839,111.167838557093));
#36519=CARTESIAN_POINT('Ctrl Pts',(0.451735300993305,6.75412809334853,111.175960329479));
#36520=CARTESIAN_POINT('Ctrl Pts',(0.278545199562873,6.76348586692237,111.184082101865));
#36521=CARTESIAN_POINT('Ctrl Pts',(0.105247092715271,6.7661814969357,111.192203874251));
#36522=CARTESIAN_POINT('Ctrl Pts',(-0.068050230422212,6.76887711475852,
111.200325609908));
#36523=CARTESIAN_POINT('Ctrl Pts',(-0.241455192060132,6.76491064225783,
111.208447345564));
#36524=CARTESIAN_POINT('Ctrl Pts',(-0.414414701403533,6.7542985909168,111.216569081221));
#36525=CARTESIAN_POINT('Ctrl Pts',(-0.587406363512533,6.74368456682041,
111.224692326689));
#36526=CARTESIAN_POINT('Ctrl Pts',(-0.759952043109946,6.72642252596304,
111.232815572157));
#36527=CARTESIAN_POINT('Ctrl Pts',(-0.931502866286227,6.70258095140227,
111.240938817626));
#36528=CARTESIAN_POINT('Ctrl Pts',(-1.1031182494974,6.67873040449816,111.24906512013));
#36529=CARTESIAN_POINT('Ctrl Pts',(-1.2737376685576,6.64829544362148,111.257191422634));
#36530=CARTESIAN_POINT('Ctrl Pts',(-1.44282159062039,6.61139583277538,111.265317725138));
#36531=CARTESIAN_POINT('Ctrl Pts',(-1.61210274199256,6.57445318007955,111.273453506633));
#36532=CARTESIAN_POINT('Ctrl Pts',(-1.7798444611894,6.53103089407988,111.281589288128));
#36533=CARTESIAN_POINT('Ctrl Pts',(-1.94552064297387,6.48129913117444,111.289725069624));
#36534=CARTESIAN_POINT('Ctrl Pts',(-2.1113003983228,6.43153627812741,111.297865937257));
#36535=CARTESIAN_POINT('Ctrl Pts',(-2.27501169824269,6.37545620752656,111.30600680489));
#36536=CARTESIAN_POINT('Ctrl Pts',(-2.4361479277498,6.31327745898439,111.314147672523));
#36537=CARTESIAN_POINT('Ctrl Pts',(-2.59753321811656,6.25100260361006,111.322301123121));
#36538=CARTESIAN_POINT('Ctrl Pts',(-2.75633515188049,6.18261038399618,111.330454573719));
#36539=CARTESIAN_POINT('Ctrl Pts',(-2.91207022012727,6.10836606901125,111.338608024316));
#36540=CARTESIAN_POINT('Ctrl Pts',(-3.02907084637388,6.05258780759409,111.344733547853));
#36541=CARTESIAN_POINT('Ctrl Pts',(-3.14434096578099,5.99350746075695,111.35085907139));
#36542=CARTESIAN_POINT('Ctrl Pts',(-3.25768657164231,5.93125342578964,111.356984594926));
#36543=CARTESIAN_POINT('Ctrl Pts',(-3.41000582771465,5.8475934707198,111.365216366957));
#36544=CARTESIAN_POINT('Ctrl Pts',(-3.55932394366084,5.75793941617028,111.373448138988));
#36545=CARTESIAN_POINT('Ctrl Pts',(-3.70513675860652,5.66253040610139,111.381679911019));
#36546=CARTESIAN_POINT('Ctrl Pts',(-3.85077545847961,5.56723532392505,111.389901853491));
#36547=CARTESIAN_POINT('Ctrl Pts',(-3.99291689512999,5.46619916420568,111.398123795963));
#36548=CARTESIAN_POINT('Ctrl Pts',(-4.1310803784713,5.35970744599082,111.406345738436));
#36549=CARTESIAN_POINT('Ctrl Pts',(-4.26910656307485,5.25332155297767,111.414559510426));
#36550=CARTESIAN_POINT('Ctrl Pts',(-4.40316238502532,5.14149111542185,111.422773282416));
#36551=CARTESIAN_POINT('Ctrl Pts',(-4.53279502223442,5.02454558009049,111.430987054406));
#36552=CARTESIAN_POINT('Ctrl Pts',(-4.66232480176227,4.90769283579428,111.439194309136));
#36553=CARTESIAN_POINT('Ctrl Pts',(-4.78743812205835,4.78573331650393,111.447401563866));
#36554=CARTESIAN_POINT('Ctrl Pts',(-4.90771416413068,4.65903752755771,111.455608818597));
#36555=CARTESIAN_POINT('Ctrl Pts',(-5.02791885589199,4.53241689725316,111.463811204609));
#36556=CARTESIAN_POINT('Ctrl Pts',(-5.14329173993053,4.40106585362844,111.472013590621));
#36557=CARTESIAN_POINT('Ctrl Pts',(-5.25344783289772,4.2653926978676,111.480215976633));
#36558=CARTESIAN_POINT('Ctrl Pts',(-5.36357104694305,4.12976003725293,111.488415914431));
#36559=CARTESIAN_POINT('Ctrl Pts',(-5.46848034298784,3.98980810959565,111.49661585223));
#36560=CARTESIAN_POINT('Ctrl Pts',(-5.56782996976534,3.84597951473782,111.504815790029));
#36561=CARTESIAN_POINT('Ctrl Pts',(-5.66716570490075,3.70217103082984,111.513014581264));
#36562=CARTESIAN_POINT('Ctrl Pts',(-5.76094311472714,3.55448725364313,111.5212133725));
#36563=CARTESIAN_POINT('Ctrl Pts',(-5.84885886406463,3.40340109129862,111.529412163736));
#36564=CARTESIAN_POINT('Ctrl Pts',(-5.93677826888471,3.25230864688473,111.537611295872));
#36565=CARTESIAN_POINT('Ctrl Pts',(-6.01883534731291,3.09781384524642,111.545810428009));
#36566=CARTESIAN_POINT('Ctrl Pts',(-6.09477192685879,2.94041564401599,111.554009560145));
#36567=CARTESIAN_POINT('Ctrl Pts',(-6.17072543903968,2.78298234552009,111.562210520556));
#36568=CARTESIAN_POINT('Ctrl Pts',(-6.24055557839082,2.62264468073213,111.570411480967));
#36569=CARTESIAN_POINT('Ctrl Pts',(-6.30405164315535,2.45992314522838,111.578612441378));
#36570=CARTESIAN_POINT('Ctrl Pts',(-6.36760721901788,2.29704910047418,111.586821088063));
#36571=CARTESIAN_POINT('Ctrl Pts',(-6.42481672895831,2.13178705543421,111.595029734748));
#36572=CARTESIAN_POINT('Ctrl Pts',(-6.47551854354318,1.96467518746191,111.603238381433));
#36573=CARTESIAN_POINT('Ctrl Pts',(-6.52624456459836,1.79748353559025,111.611450947157));
#36574=CARTESIAN_POINT('Ctrl Pts',(-6.5704566049084,1.62844064650194,111.61966351288));
#36575=CARTESIAN_POINT('Ctrl Pts',(-6.60804385955467,1.45809648178776,111.627876078604));
#36576=CARTESIAN_POINT('Ctrl Pts',(-6.64568268933818,1.28751858029882,111.636099913152));
#36577=CARTESIAN_POINT('Ctrl Pts',(-6.67667850267813,1.11563618756065,111.644323747701));
#36578=CARTESIAN_POINT('Ctrl Pts',(-6.70097204536584,0.943007236040943,
111.65254758225));
#36579=CARTESIAN_POINT('Ctrl Pts',(-6.72329324126598,0.784393702624233,
111.660103739224));
#36580=CARTESIAN_POINT('Ctrl Pts',(-6.73995685897951,0.625150185465986,
111.667659896199));
#36581=CARTESIAN_POINT('Ctrl Pts',(-6.75095573916353,0.465709789305583,
111.675216053173));
#36582=CARTESIAN_POINT('Ctrl Pts',(-6.76161267506723,0.311226236987937,
111.682537296719));
#36583=CARTESIAN_POINT('Ctrl Pts',(-6.76696678843674,0.156380053440347,
111.689858540264));
#36584=CARTESIAN_POINT('Ctrl Pts',(-6.76699984597149,0.00144382195464194,
111.69717978381));
#36585=CARTESIAN_POINT('',(-6.767,-6.60172908859006E-10,111.302820216221));
#36586=CARTESIAN_POINT('Ctrl Pts',(3.09917575053264,6.01559628526636,110.651392015122));
#36587=CARTESIAN_POINT('Ctrl Pts',(2.93382384459273,6.10078395293755,110.660141463035));
#36588=CARTESIAN_POINT('Ctrl Pts',(2.76495772122995,6.17915010267044,110.668890910947));
#36589=CARTESIAN_POINT('Ctrl Pts',(2.59315093316725,6.25042856433172,110.67764035886));
#36590=CARTESIAN_POINT('Ctrl Pts',(2.42134553245632,6.32170645041445,110.68638973612));
#36591=CARTESIAN_POINT('Ctrl Pts',(2.24659977927607,6.38589665313452,110.69513911338));
#36592=CARTESIAN_POINT('Ctrl Pts',(2.06950718689937,6.44278115439069,110.70388849064));
#36593=CARTESIAN_POINT('Ctrl Pts',(1.89241596572869,6.49966521519722,110.712637800154));
#36594=CARTESIAN_POINT('Ctrl Pts',(1.71297821457194,6.54924360009547,110.721387109669));
#36595=CARTESIAN_POINT('Ctrl Pts',(1.5318033733583,6.5913479217356,110.730136419184));
#36596=CARTESIAN_POINT('Ctrl Pts',(1.35062987477763,6.63345193135309,110.73888566386));
#36597=CARTESIAN_POINT('Ctrl Pts',(1.16771959102928,6.66808192368242,110.747634908536));
#36598=CARTESIAN_POINT('Ctrl Pts',(0.983693746906564,6.69512028363172,110.756384153212));
#36599=CARTESIAN_POINT('Ctrl Pts',(0.799669205419412,6.72215845218873,110.765133335956));
#36600=CARTESIAN_POINT('Ctrl Pts',(0.614529402872837,6.74160505424585,110.7738825187));
#36601=CARTESIAN_POINT('Ctrl Pts',(0.428903127362429,6.75339404354127,110.782631701445));
#36602=CARTESIAN_POINT('Ctrl Pts',(0.243278104162903,6.76518295330334,110.791380825163));
#36603=CARTESIAN_POINT('Ctrl Pts',(0.0571669005379851,6.76931433552277,
110.800129948882));
#36604=CARTESIAN_POINT('Ctrl Pts',(-0.1287984047788,6.7657741590247,110.8088790726));
#36605=CARTESIAN_POINT('Ctrl Pts',(-0.314762517260398,6.76223400523435,
110.8176281402));
#36606=CARTESIAN_POINT('Ctrl Pts',(-0.50058044682082,6.75102239665079,110.826377207799));
#36607=CARTESIAN_POINT('Ctrl Pts',(-0.685621118843931,6.73217741012484,
110.835126275398));
#36608=CARTESIAN_POINT('Ctrl Pts',(-0.870660665416062,6.71333253821752,
110.843875289784));
#36609=CARTESIAN_POINT('Ctrl Pts',(-1.05492267885669,6.68685441030584,110.85262430417));
#36610=CARTESIAN_POINT('Ctrl Pts',(-1.23778137635459,6.65283295028139,110.861373318555));
#36611=CARTESIAN_POINT('Ctrl Pts',(-1.42999922979042,6.61707018861823,110.870570128923));
#36612=CARTESIAN_POINT('Ctrl Pts',(-1.62066601233879,6.57297172934367,110.87976693929));
#36613=CARTESIAN_POINT('Ctrl Pts',(-1.80906628500558,6.52070304311246,110.888963749658));
#36614=CARTESIAN_POINT('Ctrl Pts',(-1.98831342545691,6.4709737491498,110.897713747395));
#36615=CARTESIAN_POINT('Ctrl Pts',(-2.16550875896856,6.41384933989476,110.906463745133));
#36616=CARTESIAN_POINT('Ctrl Pts',(-2.34005036714157,6.34952386240422,110.915213742871));
#36617=CARTESIAN_POINT('Ctrl Pts',(-2.51458843547236,6.28519968948537,110.923963563152));
#36618=CARTESIAN_POINT('Ctrl Pts',(-2.68647261718205,6.21367483971035,110.932713383433));
#36619=CARTESIAN_POINT('Ctrl Pts',(-2.85511905908882,6.13519226743774,110.941463203713));
#36620=CARTESIAN_POINT('Ctrl Pts',(-3.02376230489042,6.05671118252858,110.950212858172));
#36621=CARTESIAN_POINT('Ctrl Pts',(-3.18916767380069,5.97127275992545,110.958962512631));
#36622=CARTESIAN_POINT('Ctrl Pts',(-3.35077334102958,5.87916720437899,110.967712167089));
#36623=CARTESIAN_POINT('Ctrl Pts',(-3.51237616037538,5.7870632719554,110.976461667358));
#36624=CARTESIAN_POINT('Ctrl Pts',(-3.67017916302467,5.6882925836219,110.985211167626));
#36625=CARTESIAN_POINT('Ctrl Pts',(-3.82364636566628,5.58319061740929,110.993960667894));
#36626=CARTESIAN_POINT('Ctrl Pts',(-3.97711106778959,5.47809036367585,111.002710025603));
#36627=CARTESIAN_POINT('Ctrl Pts',(-4.12623987482084,5.36665920043104,111.011459383311));
#36628=CARTESIAN_POINT('Ctrl Pts',(-4.27052628214082,5.2492755951221,111.02020874102));
#36629=CARTESIAN_POINT('Ctrl Pts',(-4.41481053025127,5.13189374642908,111.028957967796));
#36630=CARTESIAN_POINT('Ctrl Pts',(-4.55425230136675,5.00855981477221,111.037707194573));
#36631=CARTESIAN_POINT('Ctrl Pts',(-4.68837800630689,4.87969268191941,111.046456421349));
#36632=CARTESIAN_POINT('Ctrl Pts',(-4.82250188229041,4.75082730631662,111.05520552882));
#36633=CARTESIAN_POINT('Ctrl Pts',(-4.95130963053117,4.61642907903365,111.063954636291));
#36634=CARTESIAN_POINT('Ctrl Pts',(-5.07436379033522,4.47695444731515,111.072703743762));
#36635=CARTESIAN_POINT('Ctrl Pts',(-5.19741643562965,4.33748153220396,111.081452743552));
#36636=CARTESIAN_POINT('Ctrl Pts',(-5.31471544462937,4.19293255254382,111.090201743341));
#36637=CARTESIAN_POINT('Ctrl Pts',(-5.42586245275794,4.0437984177938,111.098950743131));
#36638=CARTESIAN_POINT('Ctrl Pts',(-5.53702160019302,3.8946479948413,111.107700698473));
#36639=CARTESIAN_POINT('Ctrl Pts',(-5.64202723081384,3.7409116444365,111.116450653815));
#36640=CARTESIAN_POINT('Ctrl Pts',(-5.74052265233084,3.58311159163046,111.125200609158));
#36641=CARTESIAN_POINT('Ctrl Pts',(-5.83901427067031,3.4253176319159,111.13395022664));
#36642=CARTESIAN_POINT('Ctrl Pts',(-5.93099603115849,3.26346052695414,111.142699844122));
#36643=CARTESIAN_POINT('Ctrl Pts',(-6.01615550622859,3.09809004466872,111.151449461605));
#36644=CARTESIAN_POINT('Ctrl Pts',(-6.10131214578897,2.93272506863624,111.160198787756));
#36645=CARTESIAN_POINT('Ctrl Pts',(-6.17964682328838,2.76384720416692,111.168948113907));
#36646=CARTESIAN_POINT('Ctrl Pts',(-6.25089348288647,2.59203002791393,111.177697440058));
#36647=CARTESIAN_POINT('Ctrl Pts',(-6.32213814889409,2.42021765936823,111.18644652139));
#36648=CARTESIAN_POINT('Ctrl Pts',(-6.3862950841266,2.24546640831706,111.195195602721));
#36649=CARTESIAN_POINT('Ctrl Pts',(-6.44314639819882,2.06836976659823,111.203944684053));
#36650=CARTESIAN_POINT('Ctrl Pts',(-6.50000285283768,1.89125711158043,111.212694556487));
#36651=CARTESIAN_POINT('Ctrl Pts',(-6.54955227673314,1.71179891440008,111.221444428922));
#36652=CARTESIAN_POINT('Ctrl Pts',(-6.59162635926446,1.53060476278169,111.230194301356));
#36653=CARTESIAN_POINT('Ctrl Pts',(-6.63369752055246,1.34942319164451,111.238943566279));
#36654=CARTESIAN_POINT('Ctrl Pts',(-6.66829431424293,1.16650618642478,111.247692831201));
#36655=CARTESIAN_POINT('Ctrl Pts',(-6.69529923745448,0.982474997616478,
111.256442096124));
#36656=CARTESIAN_POINT('Ctrl Pts',(-6.72230554731469,0.798434359175636,
111.265191810303));
#36657=CARTESIAN_POINT('Ctrl Pts',(-6.74171916496723,0.613279706238205,
111.273941524483));
#36658=CARTESIAN_POINT('Ctrl Pts',(-6.75347414817289,0.427639953653224,
111.282691238663));
#36659=CARTESIAN_POINT('Ctrl Pts',(-6.76248837758739,0.285283364198692,
111.289400897838));
#36660=CARTESIAN_POINT('Ctrl Pts',(-6.76699999999987,0.142641701107519,
111.296110557014));
#36661=CARTESIAN_POINT('Ctrl Pts',(-6.767,6.25035709384319E-12,111.30282021619));
#36662=CARTESIAN_POINT('Ctrl Pts',(-6.767,-6.59981407869779E-10,111.302820216221));
#36663=CARTESIAN_POINT('Ctrl Pts',(-6.76699999998186,-0.186007250075648,
111.311569728027));
#36664=CARTESIAN_POINT('Ctrl Pts',(-6.7593263729181,-0.372014356186741,
111.320319239833));
#36665=CARTESIAN_POINT('Ctrl Pts',(-6.74400518261492,-0.557389537812749,
111.329068751639));
#36666=CARTESIAN_POINT('Ctrl Pts',(-6.72868405702401,-0.74276393646773,
111.33781822649));
#36667=CARTESIAN_POINT('Ctrl Pts',(-6.70571545643943,-0.927506130349254,
111.34656770134));
#36668=CARTESIAN_POINT('Ctrl Pts',(-6.67517739404809,-1.11098863990112,
111.355317176191));
#36669=CARTESIAN_POINT('Ctrl Pts',(-6.64463945810433,-1.29447038971527,
111.364066614813));
#36670=CARTESIAN_POINT('Ctrl Pts',(-6.60653217012702,-1.47669218292891,
111.372816053435));
#36671=CARTESIAN_POINT('Ctrl Pts',(-6.56098496100484,-1.65703510568372,
111.381565492057));
#36672=CARTESIAN_POINT('Ctrl Pts',(-6.51543793669517,-1.83737729667852,
111.390314895177));
#36673=CARTESIAN_POINT('Ctrl Pts',(-6.46245112182883,-2.01584035460391,
111.399064298297));
#36674=CARTESIAN_POINT('Ctrl Pts',(-6.40220448394752,-2.19181813700915,
111.407813701418));
#36675=CARTESIAN_POINT('Ctrl Pts',(-6.34195808551965,-2.36779521998144,
111.416563069763));
#36676=CARTESIAN_POINT('Ctrl Pts',(-6.27445201464304,-2.54128677606384,
111.425312438108));
#36677=CARTESIAN_POINT('Ctrl Pts',(-6.19991555109572,-2.71170355298684,
111.434061806453));
#36678=CARTESIAN_POINT('Ctrl Pts',(-6.1253793776076,-2.88211966673172,111.44281114075));
#36679=CARTESIAN_POINT('Ctrl Pts',(-6.04381298103703,-3.04946076269732,
111.451560475048));
#36680=CARTESIAN_POINT('Ctrl Pts',(-5.95549339394793,-3.21315848265263,
111.460309809345));
#36681=CARTESIAN_POINT('Ctrl Pts',(-5.86717414322048,-3.37685557917168,
111.46905911032));
#36682=CARTESIAN_POINT('Ctrl Pts',(-5.77210188951562,-3.536909075239,111.477808411296));
#36683=CARTESIAN_POINT('Ctrl Pts',(-5.67059953430871,-3.69277536840489,
111.486557712271));
#36684=CARTESIAN_POINT('Ctrl Pts',(-5.56909755724049,-3.8486410809037,111.495306980652));
#36685=CARTESIAN_POINT('Ctrl Pts',(-5.46116568298875,-4.00031938157787,
111.504056249033));
#36686=CARTESIAN_POINT('Ctrl Pts',(-5.34717048645489,-4.14729511715597,
111.512805517413));
#36687=CARTESIAN_POINT('Ctrl Pts',(-5.23317570513439,-4.2942703173932,111.521554753926));
#36688=CARTESIAN_POINT('Ctrl Pts',(-5.11311782135318,-4.4365427603725,111.530303990439));
#36689=CARTESIAN_POINT('Ctrl Pts',(-4.98740459127167,-4.57362924196554,
111.539053226951));
#36690=CARTESIAN_POINT('Ctrl Pts',(-4.8616918086462,-4.71071523562129,111.547802432323));
#36691=CARTESIAN_POINT('Ctrl Pts',(-4.73032391367906,-4.84261509362948,
111.556551637694));
#36692=CARTESIAN_POINT('Ctrl Pts',(-4.59374707188508,-4.96888084376626,
111.565300843065));
#36693=CARTESIAN_POINT('Ctrl Pts',(-4.45717070487386,-5.09514615496477,
111.574050018021));
#36694=CARTESIAN_POINT('Ctrl Pts',(-4.31538563768318,-5.21577720295986,
111.582799192977));
#36695=CARTESIAN_POINT('Ctrl Pts',(-4.16887341238342,-5.33036429069558,
111.591548367933));
#36696=CARTESIAN_POINT('Ctrl Pts',(-4.022361684239,-5.44495098960653,111.600297513201));
#36697=CARTESIAN_POINT('Ctrl Pts',(-3.87112305579928,-5.55349359276757,
111.609046658469));
#36698=CARTESIAN_POINT('Ctrl Pts',(-3.71567117261211,-5.6556234613895,111.617795803737));
#36699=CARTESIAN_POINT('Ctrl Pts',(-3.56021980400825,-5.75775299193688,
111.626544920043));
#36700=CARTESIAN_POINT('Ctrl Pts',(-3.40055544805023,-5.85346967308677,
111.635294036349));
#36701=CARTESIAN_POINT('Ctrl Pts',(-3.23722036265219,-5.94244842835258,
111.644043152656));
#36702=CARTESIAN_POINT('Ctrl Pts',(-3.07388580437007,-6.03142689646564,
111.652792240727));
#36703=CARTESIAN_POINT('Ctrl Pts',(-2.90688079197878,-6.11366734513269,
111.661541328797));
#36704=CARTESIAN_POINT('Ctrl Pts',(-2.73677251034066,-6.18889046814077,
111.670290416868));
#36705=CARTESIAN_POINT('Ctrl Pts',(-2.56666476355359,-6.26411335463382,
111.679039477431));
#36706=CARTESIAN_POINT('Ctrl Pts',(-2.39345402910139,-6.33231884373708,
111.687788537993));
#36707=CARTESIAN_POINT('Ctrl Pts',(-2.21772856411486,-6.39327529642741,
111.696537598555));
#36708=CARTESIAN_POINT('Ctrl Pts',(-2.04200363705142,-6.45423156252053,
111.705286632335));
#36709=CARTESIAN_POINT('Ctrl Pts',(-1.86376426556463,-6.50793874270278,
111.714035666115));
#36710=CARTESIAN_POINT('Ctrl Pts',(-1.68361578130627,-6.55421443812578,
111.722784699895));
#36711=CARTESIAN_POINT('Ctrl Pts',(-1.5034678335538,-6.60048999573368,111.731533707619));
#36712=CARTESIAN_POINT('Ctrl Pts',(-1.32141106192404,-6.639334041584,111.740282715344));
#36713=CARTESIAN_POINT('Ctrl Pts',(-1.13806375893922,-6.6706146553814,111.749031723068));
#36714=CARTESIAN_POINT('Ctrl Pts',(-0.954716986764568,-6.70189517861806,
111.757780705463));
#36715=CARTESIAN_POINT('Ctrl Pts',(-0.770079973152659,-6.72561226543354,
111.766529687858));
#36716=CARTESIAN_POINT('Ctrl Pts',(-0.584779769893354,-6.74168536945499,
111.775278670252));
#36717=CARTESIAN_POINT('Ctrl Pts',(-0.39149064690006,-6.75845143946161,
111.784404850928));
#36718=CARTESIAN_POINT('Ctrl Pts',(-0.197480212456598,-6.76689975925897,
111.793531031604));
#36719=CARTESIAN_POINT('Ctrl Pts',(-0.00346532565696627,-6.7669991127174,
111.80265721228));
#36720=CARTESIAN_POINT('Ctrl Pts',(0.184486595930185,-6.76709536138026,
111.811498199809));
#36721=CARTESIAN_POINT('Ctrl Pts',(0.372442378811916,-6.75935659723298,
111.820339187339));
#36722=CARTESIAN_POINT('Ctrl Pts',(0.55975021834066,-6.74380965723882,111.829180174868));
#36723=CARTESIAN_POINT('Ctrl Pts',(0.745129915074913,-6.72842275710419,
111.837930153466));
#36724=CARTESIAN_POINT('Ctrl Pts',(0.929874656929226,-6.70538772264944,
111.846680132064));
#36725=CARTESIAN_POINT('Ctrl Pts',(1.11335688351,-6.6747828017053,111.855430110662));
#36726=CARTESIAN_POINT('Ctrl Pts',(1.29683723179798,-6.64417819406129,111.864179999687));
#36727=CARTESIAN_POINT('Ctrl Pts',(1.47905480790826,-6.60600390216509,111.872929888712));
#36728=CARTESIAN_POINT('Ctrl Pts',(1.65939064864979,-6.56038959781914,111.881679777737));
#36729=CARTESIAN_POINT('Ctrl Pts',(1.83972470324011,-6.51477574526384,111.890429580098));
#36730=CARTESIAN_POINT('Ctrl Pts',(2.018176781851,-6.46172209801594,111.899179382458));
#36731=CARTESIAN_POINT('Ctrl Pts',(2.19414072406371,-6.40140886703897,111.907929184819));
#36732=CARTESIAN_POINT('Ctrl Pts',(2.3701029819023,-6.34109621339646,111.916678903425));
#36733=CARTESIAN_POINT('Ctrl Pts',(2.54357687984421,-6.27352420802654,111.92542862203));
#36734=CARTESIAN_POINT('Ctrl Pts',(2.71397317846791,-6.1989223730062,111.934178340636));
#36735=CARTESIAN_POINT('Ctrl Pts',(2.88436790263341,-6.12432122730523,111.942927978394));
#36736=CARTESIAN_POINT('Ctrl Pts',(3.05168482181653,-6.04269049689441,111.951677616152));
#36737=CARTESIAN_POINT('Ctrl Pts',(3.21535562051979,-5.95430745205451,111.960427253911));
#36738=CARTESIAN_POINT('Ctrl Pts',(3.37902496129059,-5.86592519450538,111.96917681373));
#36739=CARTESIAN_POINT('Ctrl Pts',(3.5390479943778,-5.77079087907787,111.977926373549));
#36740=CARTESIAN_POINT('Ctrl Pts',(3.69488118866957,-5.66922763713151,111.986675933368));
#36741=CARTESIAN_POINT('Ctrl Pts',(3.85071304661876,-5.56766526613749,111.995425418155));
#36742=CARTESIAN_POINT('Ctrl Pts',(4.00235489756023,-5.4596742354402,112.004174902943));
#36743=CARTESIAN_POINT('Ctrl Pts',(4.14929168656665,-5.34562133898286,112.01292438773));
#36744=CARTESIAN_POINT('Ctrl Pts',(4.29622726433722,-5.23156938269141,112.021673800393));
#36745=CARTESIAN_POINT('Ctrl Pts',(4.43845763138931,-5.11145583636508,112.030423213057));
#36746=CARTESIAN_POINT('Ctrl Pts',(4.57549970706673,-4.98568866162261,112.03917262572));
#36747=CARTESIAN_POINT('Ctrl Pts',(4.71254069859846,-4.85992248182961,112.047921969166));
#36748=CARTESIAN_POINT('Ctrl Pts',(4.84439326974654,-4.728502956896,112.056671312613));
#36749=CARTESIAN_POINT('Ctrl Pts',(4.97060959476779,-4.5918764417613,112.065420656059));
#36750=CARTESIAN_POINT('Ctrl Pts',(5.09682496321357,-4.45525096209941,112.074169933195));
#36751=CARTESIAN_POINT('Ctrl Pts',(5.21740397655394,-4.31341878170482,112.082919210332));
#36752=CARTESIAN_POINT('Ctrl Pts',(5.33193710490156,-4.16686161389768,112.091668487468));
#36753=CARTESIAN_POINT('Ctrl Pts',(5.44646940326257,-4.02030550814558,112.100417701201));
#36754=CARTESIAN_POINT('Ctrl Pts',(5.55495572785148,-3.86902470929188,112.109166914934));
#36755=CARTESIAN_POINT('Ctrl Pts',(5.6570276252551,-3.71353301413905,112.117916128667));
#36756=CARTESIAN_POINT('Ctrl Pts',(5.75909881687784,-3.55804239414078,112.126665281903));
#36757=CARTESIAN_POINT('Ctrl Pts',(5.85475551281949,-3.39834117565858,112.135414435139));
#36758=CARTESIAN_POINT('Ctrl Pts',(5.94367283757764,-3.23497174637457,112.144163588375));
#36759=CARTESIAN_POINT('Ctrl Pts',(6.0325895770449,-3.07160339245624,112.152912684021));
#36760=CARTESIAN_POINT('Ctrl Pts',(6.11476689711938,-2.90456712773393,112.161661779666));
#36761=CARTESIAN_POINT('Ctrl Pts',(6.1899257055036,-2.73443024419088,112.170410875312));
#36762=CARTESIAN_POINT('Ctrl Pts',(6.26508404412242,-2.56429442405506,112.179159916273));
#36763=CARTESIAN_POINT('Ctrl Pts',(6.33322384305276,-2.39105828597825,112.187908957234));
#36764=CARTESIAN_POINT('Ctrl Pts',(6.39411368740385,-2.21531017073336,112.196657998195));
#36765=CARTESIAN_POINT('Ctrl Pts',(6.45500317139635,-2.0395630956019,112.205406987377));
#36766=CARTESIAN_POINT('Ctrl Pts',(6.50864269287186,-1.86130434378794,112.21415597656));
#36767=CARTESIAN_POINT('Ctrl Pts',(6.55485008461795,-1.6811393065966,112.222904965742));
#36768=CARTESIAN_POINT('Ctrl Pts',(6.60199664762854,-1.49731239152371,112.231831779271));
#36769=CARTESIAN_POINT('Ctrl Pts',(6.64140563652433,-1.31150116441116,112.2407585928));
#36770=CARTESIAN_POINT('Ctrl Pts',(6.6729377229187,-1.12436255098105,112.249685406328));
#36771=CARTESIAN_POINT('Ctrl Pts',(6.70384494957986,-0.940932394473189,
112.258435320484));
#36772=CARTESIAN_POINT('Ctrl Pts',(6.72718449355451,-0.75622725992661,112.267185234639));
#36773=CARTESIAN_POINT('Ctrl Pts',(6.74287707378854,-0.570874563960297,
112.275935148795));
#36774=CARTESIAN_POINT('Ctrl Pts',(6.75856934541995,-0.385525513049683,
112.284684890879));
#36775=CARTESIAN_POINT('Ctrl Pts',(6.76661493005824,-0.199529211834698,
112.293434632963));
#36776=CARTESIAN_POINT('Ctrl Pts',(6.76698649909023,-0.0135174380168191,
112.302184375047));
#36777=CARTESIAN_POINT('Ctrl Pts',(6.76735806130902,0.172490925029494,112.310933956693));
#36778=CARTESIAN_POINT('Ctrl Pts',(6.76005588893197,0.358514473484569,112.319683538339));
#36779=CARTESIAN_POINT('Ctrl Pts',(6.74510478449892,0.543921360244159,112.328433119985));
#36780=CARTESIAN_POINT('Ctrl Pts',(6.73015393434395,0.729325093731156,112.337182552824));
#36781=CARTESIAN_POINT('Ctrl Pts',(6.70755443549009,0.914111900835165,112.345931985663));
#36782=CARTESIAN_POINT('Ctrl Pts',(6.67738304672846,1.09765415649164,112.354681418502));
#36783=CARTESIAN_POINT('Ctrl Pts',(6.64721213100804,1.28119353448634,112.363430714163));
#36784=CARTESIAN_POINT('Ctrl Pts',(6.60946960942866,1.46348811729683,112.372180009824));
#36785=CARTESIAN_POINT('Ctrl Pts',(6.56428366976999,1.64391876404857,112.380929305486));
#36786=CARTESIAN_POINT('Ctrl Pts',(6.51909837851975,1.82434682165971,112.389678475596));
#36787=CARTESIAN_POINT('Ctrl Pts',(6.46646995254635,2.00291071876256,112.398427645707));
#36788=CARTESIAN_POINT('Ctrl Pts',(6.4065771326274,2.17900400268007,112.407176815818));
#36789=CARTESIAN_POINT('Ctrl Pts',(6.3466850925873,2.35509499364443,112.415925872004));
#36790=CARTESIAN_POINT('Ctrl Pts',(6.27952894015698,2.52871516452327,112.42467492819));
#36791=CARTESIAN_POINT('Ctrl Pts',(6.20533675038147,2.69927486824982,112.433423984375));
#36792=CARTESIAN_POINT('Ctrl Pts',(6.1283211788406,2.87632521686588,112.442505985657));
#36793=CARTESIAN_POINT('Ctrl Pts',(6.04372366601886,3.05007728967782,112.451587986938));
#36794=CARTESIAN_POINT('Ctrl Pts',(5.95185377983551,3.21989527523145,112.460669988219));
#36795=CARTESIAN_POINT('Ctrl Pts',(5.86334450791821,3.38350129331029,112.469419768526));
#36796=CARTESIAN_POINT('Ctrl Pts',(5.768085620305,3.54345567168515,112.478169548833));
#36797=CARTESIAN_POINT('Ctrl Pts',(5.66640068776555,3.69921508508091,112.48691932914));
#36798=CARTESIAN_POINT('Ctrl Pts',(5.56471941078815,3.85496889894302,112.495668794894));
#36799=CARTESIAN_POINT('Ctrl Pts',(5.45661270784858,4.00652780960844,112.504418260647));
#36800=CARTESIAN_POINT('Ctrl Pts',(5.34244776417745,4.15337704609578,112.513167726401));
#36801=CARTESIAN_POINT('Ctrl Pts',(5.22828631787118,4.30022178395735,112.52191692412));
#36802=CARTESIAN_POINT('Ctrl Pts',(5.1080671781052,4.44235691011256,112.53066612184));
#36803=CARTESIAN_POINT('Ctrl Pts',(4.98219864510137,4.5792996910827,112.539415319559));
#36804=CARTESIAN_POINT('Ctrl Pts',(4.85633329908418,4.71623900466664,112.54816429575));
#36805=CARTESIAN_POINT('Ctrl Pts',(4.72481903997058,4.84798602519277,112.55691327194));
#36806=CARTESIAN_POINT('Ctrl Pts',(4.58810250699667,4.97409332293744,112.56566224813));
#36807=CARTESIAN_POINT('Ctrl Pts',(4.45137708647154,5.10020881855727,112.574411793066));
#36808=CARTESIAN_POINT('Ctrl Pts',(4.30944892596649,5.22068366340458,112.583161338002));
#36809=CARTESIAN_POINT('Ctrl Pts',(4.16280009426389,5.33510865636273,112.591910882939));
#36810=CARTESIAN_POINT('Ctrl Pts',(4.0161598830765,5.4495269230321,112.600659913547));
#36811=CARTESIAN_POINT('Ctrl Pts',(3.86479978190271,5.55789587317804,112.609408944155));
#36812=CARTESIAN_POINT('Ctrl Pts',(3.70923383538335,5.65984746741883,112.618157974763));
#36813=CARTESIAN_POINT('Ctrl Pts',(3.55366577756041,5.76180044532212,112.626907124111));
#36814=CARTESIAN_POINT('Ctrl Pts',(3.39389199982622,5.8573357359668,112.63565627346));
#36815=CARTESIAN_POINT('Ctrl Pts',(3.23045513581156,5.94612887646313,112.644405422808));
#36816=CARTESIAN_POINT('Ctrl Pts',(3.18695122121477,5.96976399222616,112.646734286913));
#36817=CARTESIAN_POINT('Ctrl Pts',(3.14318791247529,5.99292165443131,112.649063151017));
#36818=CARTESIAN_POINT('Ctrl Pts',(3.09917575053259,6.01559628526639,112.651392015122));
#36819=CARTESIAN_POINT('Origin',(0.,0.,-3.69717978381041));
#36820=CARTESIAN_POINT('',(3.09917575053242,6.01559628526648,115.045751582742));
#36821=CARTESIAN_POINT('',(3.09917575053242,6.01559628526647,114.651222310038));
#36822=CARTESIAN_POINT('',(3.09917575053259,6.01559628526639,-3.69717978381041));
#36823=CARTESIAN_POINT('',(-6.767,6.57024998643174E-12,113.69717978381));
#36824=CARTESIAN_POINT('Ctrl Pts',(-6.767,6.95491030238324E-12,113.69717978381));
#36825=CARTESIAN_POINT('Ctrl Pts',(-6.76700000000019,-0.186007249408843,
113.705929295616));
#36826=CARTESIAN_POINT('Ctrl Pts',(-6.75932637295475,-0.372014355520823,
113.714678807422));
#36827=CARTESIAN_POINT('Ctrl Pts',(-6.74400518266982,-0.557389537148472,
113.723428319228));
#36828=CARTESIAN_POINT('Ctrl Pts',(-6.72868405709718,-0.742763935804837,
113.732177794078));
#36829=CARTESIAN_POINT('Ctrl Pts',(-6.70571545653082,-0.927506129688499,
113.740927268929));
#36830=CARTESIAN_POINT('Ctrl Pts',(-6.67517739415758,-1.11098863924325,
113.74967674378));
#36831=CARTESIAN_POINT('Ctrl Pts',(-6.64463945823192,-1.29447038906028,
113.758426182402));
#36832=CARTESIAN_POINT('Ctrl Pts',(-6.6065321702726,-1.47669218227757,113.767175621023));
#36833=CARTESIAN_POINT('Ctrl Pts',(-6.56098496116824,-1.65703510503675,
113.775925059645));
#36834=CARTESIAN_POINT('Ctrl Pts',(-6.51543793687635,-1.83737729603604,
113.784674462766));
#36835=CARTESIAN_POINT('Ctrl Pts',(-6.46245112202761,-2.01584035396665,
113.793423865886));
#36836=CARTESIAN_POINT('Ctrl Pts',(-6.40220448416365,-2.19181813637784,
113.802173269006));
#36837=CARTESIAN_POINT('Ctrl Pts',(-6.34195808575326,-2.36779521935571,
113.810922637351));
#36838=CARTESIAN_POINT('Ctrl Pts',(-6.2744520148939,-2.54128677544442,113.819672005697));
#36839=CARTESIAN_POINT('Ctrl Pts',(-6.19991555136358,-2.71170355237443,
113.828421374042));
#36840=CARTESIAN_POINT('Ctrl Pts',(-6.12537937789223,-2.88211966612679,
113.837170708339));
#36841=CARTESIAN_POINT('Ctrl Pts',(-6.04381298133813,-3.04946076210056,
113.845920042636));
#36842=CARTESIAN_POINT('Ctrl Pts',(-5.95549339426513,-3.21315848206471,
113.854669376933));
#36843=CARTESIAN_POINT('Ctrl Pts',(-5.86717414355384,-3.37685557859248,
113.863418677909));
#36844=CARTESIAN_POINT('Ctrl Pts',(-5.77210188986478,-3.53690907466919,
113.872167978884));
#36845=CARTESIAN_POINT('Ctrl Pts',(-5.67059953467325,-3.6927753678451,113.88091727986));
#36846=CARTESIAN_POINT('Ctrl Pts',(-5.56909755762027,-3.84864108035415,
113.889666548241));
#36847=CARTESIAN_POINT('Ctrl Pts',(-5.46116568338335,-4.00031938103918,
113.898415816621));
#36848=CARTESIAN_POINT('Ctrl Pts',(-5.34717048686382,-4.14729511662873,
113.907165085002));
#36849=CARTESIAN_POINT('Ctrl Pts',(-5.23317570555789,-4.2942703168771,113.915914321515));
#36850=CARTESIAN_POINT('Ctrl Pts',(-5.11311782179079,-4.43654275986814,
113.924663558027));
#36851=CARTESIAN_POINT('Ctrl Pts',(-4.9874045917229,-4.57362924147349,113.93341279454));
#36852=CARTESIAN_POINT('Ctrl Pts',(-4.86169180911112,-4.71071523514146,
113.942161999911));
#36853=CARTESIAN_POINT('Ctrl Pts',(-4.73032391415718,-4.84261509316243,
113.950911205282));
#36854=CARTESIAN_POINT('Ctrl Pts',(-4.59374707237585,-4.96888084331253,
113.959660410653));
#36855=CARTESIAN_POINT('Ctrl Pts',(-4.45717070537701,-5.09514615452463,
113.96840958561));
#36856=CARTESIAN_POINT('Ctrl Pts',(-4.31538563819814,-5.2157772025338,113.977158760566));
#36857=CARTESIAN_POINT('Ctrl Pts',(-4.16887341290959,-5.33036429028407,
113.985907935522));
#36858=CARTESIAN_POINT('Ctrl Pts',(-4.02236168477658,-5.4449509892094,113.99465708079));
#36859=CARTESIAN_POINT('Ctrl Pts',(-3.87112305634767,-5.5534935923853,114.003406226058));
#36860=CARTESIAN_POINT('Ctrl Pts',(-3.71567117317069,-5.65562346102252,
114.012155371326));
#36861=CARTESIAN_POINT('Ctrl Pts',(-3.56021980457638,-5.75775299158561,
114.020904487632));
#36862=CARTESIAN_POINT('Ctrl Pts',(-3.40055544862726,-5.85346967275157,
114.029653603938));
#36863=CARTESIAN_POINT('Ctrl Pts',(-3.23722036323741,-5.94244842803378,
114.038402720244));
#36864=CARTESIAN_POINT('Ctrl Pts',(-3.07388580496405,-6.03142689616292,
114.047151808315));
#36865=CARTESIAN_POINT('Ctrl Pts',(-2.90688079258086,-6.11366734484642,
114.055900896386));
#36866=CARTESIAN_POINT('Ctrl Pts',(-2.73677251095014,-6.18889046787125,
114.064649984457));
#36867=CARTESIAN_POINT('Ctrl Pts',(-2.56666476417083,-6.2641133543809,114.073399045019));
#36868=CARTESIAN_POINT('Ctrl Pts',(-2.3934540297257,-6.33231884350109,114.082148105582));
#36869=CARTESIAN_POINT('Ctrl Pts',(-2.21772856474555,-6.39327529620864,
114.090897166144));
#36870=CARTESIAN_POINT('Ctrl Pts',(-2.042003637688,-6.45423156231914,114.099646199924));
#36871=CARTESIAN_POINT('Ctrl Pts',(-1.86376426620638,-6.507938742519,114.108395233704));
#36872=CARTESIAN_POINT('Ctrl Pts',(-1.68361578195245,-6.5542144379598,114.117144267484));
#36873=CARTESIAN_POINT('Ctrl Pts',(-1.50346783420479,-6.60048999558539,
114.125893275208));
#36874=CARTESIAN_POINT('Ctrl Pts',(-1.32141106257911,-6.63933404145362,
114.134642282932));
#36875=CARTESIAN_POINT('Ctrl Pts',(-1.13806375959763,-6.67061465526907,
114.143391290656));
#36876=CARTESIAN_POINT('Ctrl Pts',(-0.954716987426435,-6.70189517852377,
114.152140273051));
#36877=CARTESIAN_POINT('Ctrl Pts',(-0.770079973817251,-6.72561226535743,
114.160889255446));
#36878=CARTESIAN_POINT('Ctrl Pts',(-0.584779770559915,-6.74168536939717,
114.169638237841));
#36879=CARTESIAN_POINT('Ctrl Pts',(-0.391490647561377,-6.75845143942351,
114.178764418517));
#36880=CARTESIAN_POINT('Ctrl Pts',(-0.1974802131118,-6.76689975924005,114.187890599193));
#36881=CARTESIAN_POINT('Ctrl Pts',(-0.00346532630524953,-6.76699911271707,
114.197016779869));
#36882=CARTESIAN_POINT('Ctrl Pts',(0.184486595288692,-6.76709536139794,
114.205857767399));
#36883=CARTESIAN_POINT('Ctrl Pts',(0.372442378177963,-6.7593565972681,114.214698754929));
#36884=CARTESIAN_POINT('Ctrl Pts',(0.559750217714926,-6.74380965729076,
114.223539742459));
#36885=CARTESIAN_POINT('Ctrl Pts',(0.74512991445061,-6.72842275717332,114.232289721057));
#36886=CARTESIAN_POINT('Ctrl Pts',(0.929874656307067,-6.70538772273572,
114.241039699654));
#36887=CARTESIAN_POINT('Ctrl Pts',(1.11335688289069,-6.67478280180861,114.249789678252));
#36888=CARTESIAN_POINT('Ctrl Pts',(1.29683723118151,-6.64417819418161,114.258539567277));
#36889=CARTESIAN_POINT('Ctrl Pts',(1.47905480729533,-6.60600390230232,114.267289456302));
#36890=CARTESIAN_POINT('Ctrl Pts',(1.6593906480411,-6.56038959797311,114.276039345327));
#36891=CARTESIAN_POINT('Ctrl Pts',(1.83972470263565,-6.51477574543454,114.284789147688));
#36892=CARTESIAN_POINT('Ctrl Pts',(2.01817678125147,-6.46172209820319,114.293538950049));
#36893=CARTESIAN_POINT('Ctrl Pts',(2.19414072346978,-6.40140886724255,114.30228875241));
#36894=CARTESIAN_POINT('Ctrl Pts',(2.37010298131409,-6.34109621361632,114.311038471015));
#36895=CARTESIAN_POINT('Ctrl Pts',(2.54357687926239,-6.27352420826244,114.319788189621));
#36896=CARTESIAN_POINT('Ctrl Pts',(2.71397317789312,-6.19892237325785,114.328537908226));
#36897=CARTESIAN_POINT('Ctrl Pts',(2.88436790206543,-6.12432122757273,114.337287545985));
#36898=CARTESIAN_POINT('Ctrl Pts',(3.051684821256,-6.04269049717748,114.346037183743));
#36899=CARTESIAN_POINT('Ctrl Pts',(3.21535561996735,-5.95430745235282,114.354786821501));
#36900=CARTESIAN_POINT('Ctrl Pts',(3.37902496074636,-5.86592519481888,114.36353638132));
#36901=CARTESIAN_POINT('Ctrl Pts',(3.5390479938424,-5.77079087940621,114.372285941139));
#36902=CARTESIAN_POINT('Ctrl Pts',(3.69488118814359,-5.66922763747432,114.381035500958));
#36903=CARTESIAN_POINT('Ctrl Pts',(3.85071304610221,-5.56766526649475,114.389784985746));
#36904=CARTESIAN_POINT('Ctrl Pts',(4.0023548970537,-5.45967423581152,114.398534470533));
#36905=CARTESIAN_POINT('Ctrl Pts',(4.1492916860707,-5.34562133936781,114.407283955321));
#36906=CARTESIAN_POINT('Ctrl Pts',(4.29622726385176,-5.23156938309007,114.416033367984));
#36907=CARTESIAN_POINT('Ctrl Pts',(4.4384576309149,-5.11145583677703,114.424782780647));
#36908=CARTESIAN_POINT('Ctrl Pts',(4.57549970660391,-4.98568866204736,114.43353219331));
#36909=CARTESIAN_POINT('Ctrl Pts',(4.71254069814741,-4.85992248226699,114.442281536757));
#36910=CARTESIAN_POINT('Ctrl Pts',(4.84439326930777,-4.72850295734552,114.451030880203));
#36911=CARTESIAN_POINT('Ctrl Pts',(4.97060959434179,-4.59187644222243,114.459780223649));
#36912=CARTESIAN_POINT('Ctrl Pts',(5.09682496280016,-4.45525096257235,114.468529500786));
#36913=CARTESIAN_POINT('Ctrl Pts',(5.21740397615361,-4.31341878218905,114.477278777922));
#36914=CARTESIAN_POINT('Ctrl Pts',(5.33193710451476,-4.16686161439263,114.486028055058));
#36915=CARTESIAN_POINT('Ctrl Pts',(5.44646940288938,-4.02030550865117,114.494777268791));
#36916=CARTESIAN_POINT('Ctrl Pts',(5.55495572749233,-3.86902470980753,114.503526482524));
#36917=CARTESIAN_POINT('Ctrl Pts',(5.65702762491039,-3.71353301466417,114.512275696257));
#36918=CARTESIAN_POINT('Ctrl Pts',(5.75909881654756,-3.55804239467538,114.521024849493));
#36919=CARTESIAN_POINT('Ctrl Pts',(5.85475551250403,-3.39834117620206,114.529774002729));
#36920=CARTESIAN_POINT('Ctrl Pts',(5.94367283727735,-3.2349717469263,114.538523155966));
#36921=CARTESIAN_POINT('Ctrl Pts',(6.03258957675978,-3.07160339301621,114.547272251611));
#36922=CARTESIAN_POINT('Ctrl Pts',(6.11476689684977,-2.90456712830153,114.556021347257));
#36923=CARTESIAN_POINT('Ctrl Pts',(6.18992570524978,-2.73443024476546,114.564770442902));
#36924=CARTESIAN_POINT('Ctrl Pts',(6.26508404388429,-2.56429442463684,114.573519483863));
#36925=CARTESIAN_POINT('Ctrl Pts',(6.33322384283063,-2.3910582865666,114.582268524824));
#36926=CARTESIAN_POINT('Ctrl Pts',(6.39411368719797,-2.21531017132761,114.591017565785));
#36927=CARTESIAN_POINT('Ctrl Pts',(6.45500317120672,-2.03956309620204,114.599766554968));
#36928=CARTESIAN_POINT('Ctrl Pts',(6.50864269269873,-1.86130434439332,114.60851554415));
#36929=CARTESIAN_POINT('Ctrl Pts',(6.55485008446152,-1.68113930720651,114.617264533332));
#36930=CARTESIAN_POINT('Ctrl Pts',(6.60199664749247,-1.49731239212534,114.626191346862));
#36931=CARTESIAN_POINT('Ctrl Pts',(6.64140563640773,-1.31150116500351,114.635118160391));
#36932=CARTESIAN_POINT('Ctrl Pts',(6.6729377228206,-1.12436255156325,114.644044973921));
#36933=CARTESIAN_POINT('Ctrl Pts',(6.70384494949778,-0.940932395057959,
114.652794888076));
#36934=CARTESIAN_POINT('Ctrl Pts',(6.72718449348857,-0.756227260513285,
114.661544802232));
#36935=CARTESIAN_POINT('Ctrl Pts',(6.74287707373877,-0.570874564548209,
114.670294716387));
#36936=CARTESIAN_POINT('Ctrl Pts',(6.75856934538633,-0.385525513638959,
114.679044458471));
#36937=CARTESIAN_POINT('Ctrl Pts',(6.76661493004084,-0.199529212424675,
114.687794200555));
#36938=CARTESIAN_POINT('Ctrl Pts',(6.76698649908905,-0.0135174386068253,
114.696543942639));
#36939=CARTESIAN_POINT('Ctrl Pts',(6.76735806132406,0.172490924439331,114.705293524285));
#36940=CARTESIAN_POINT('Ctrl Pts',(6.76005588896323,0.358514472894918,114.714043105931));
#36941=CARTESIAN_POINT('Ctrl Pts',(6.74510478454637,0.543921359655689,114.722792687577));
#36942=CARTESIAN_POINT('Ctrl Pts',(6.73015393440758,0.729325093143993,114.731542120416));
#36943=CARTESIAN_POINT('Ctrl Pts',(6.70755443556984,0.914111900249978,114.740291553255));
#36944=CARTESIAN_POINT('Ctrl Pts',(6.67738304682422,1.09765415590909,114.749040986094));
#36945=CARTESIAN_POINT('Ctrl Pts',(6.6472121311198,1.28119353390655,114.757790281755));
#36946=CARTESIAN_POINT('Ctrl Pts',(6.60946960955629,1.46348811672046,114.766539577417));
#36947=CARTESIAN_POINT('Ctrl Pts',(6.56428366991332,1.64391876347627,114.775288873078));
#36948=CARTESIAN_POINT('Ctrl Pts',(6.51909837867883,1.82434682109123,114.784038043189));
#36949=CARTESIAN_POINT('Ctrl Pts',(6.46646995272104,2.00291071819854,114.7927872133));
#36950=CARTESIAN_POINT('Ctrl Pts',(6.40657713281749,2.17900400212116,114.80153638341));
#36951=CARTESIAN_POINT('Ctrl Pts',(6.34668509279272,2.35509499309088,114.810285439596));
#36952=CARTESIAN_POINT('Ctrl Pts',(6.27952894037749,2.52871516397569,114.819034495782));
#36953=CARTESIAN_POINT('Ctrl Pts',(6.2053367506168,2.69927486770884,114.827783551968));
#36954=CARTESIAN_POINT('Ctrl Pts',(6.12832117908154,2.87632521635419,114.83686555325));
#36955=CARTESIAN_POINT('Ctrl Pts',(6.04372366626319,3.05007728919524,114.845947554532));
#36956=CARTESIAN_POINT('Ctrl Pts',(5.95185378008107,3.21989527477753,114.855029555815));
#36957=CARTESIAN_POINT('Ctrl Pts',(5.86334450817625,3.38350129286312,114.863779336122));
#36958=CARTESIAN_POINT('Ctrl Pts',(5.76808562057524,3.54345567124525,114.872529116429));
#36959=CARTESIAN_POINT('Ctrl Pts',(5.66640068804767,3.69921508464876,114.881278896736));
#36960=CARTESIAN_POINT('Ctrl Pts',(5.56471941108222,3.85496889851852,114.890028362489));
#36961=CARTESIAN_POINT('Ctrl Pts',(5.45661270815428,4.00652780919209,114.898777828243));
#36962=CARTESIAN_POINT('Ctrl Pts',(5.34244776449444,4.15337704568805,114.907527293996));
#36963=CARTESIAN_POINT('Ctrl Pts',(5.22828631819929,4.30022178355844,114.916276491716));
#36964=CARTESIAN_POINT('Ctrl Pts',(5.10806717844407,4.44235690972291,114.925025689436));
#36965=CARTESIAN_POINT('Ctrl Pts',(4.98219864545059,4.57929969070275,114.933774887155));
#36966=CARTESIAN_POINT('Ctrl Pts',(4.85633329944376,4.71623900429639,114.942523863345));
#36967=CARTESIAN_POINT('Ctrl Pts',(4.7248190403401,4.84798602483264,114.951272839536));
#36968=CARTESIAN_POINT('Ctrl Pts',(4.58810250737571,4.97409332258782,114.960021815726));
#36969=CARTESIAN_POINT('Ctrl Pts',(4.45137708686029,5.10020881821798,114.968771360662));
#36970=CARTESIAN_POINT('Ctrl Pts',(4.30944892636451,5.22068366307603,114.977520905598));
#36971=CARTESIAN_POINT('Ctrl Pts',(4.16280009467074,5.33510865604528,114.986270450534));
#36972=CARTESIAN_POINT('Ctrl Pts',(4.01615988349207,5.44952692272583,114.995019481143));
#36973=CARTESIAN_POINT('Ctrl Pts',(3.86479978232654,5.55789587288332,115.003768511751));
#36974=CARTESIAN_POINT('Ctrl Pts',(3.70923383581495,5.65984746713598,115.012517542359));
#36975=CARTESIAN_POINT('Ctrl Pts',(3.55366577799968,5.7618004450512,115.021266691707));
#36976=CARTESIAN_POINT('Ctrl Pts',(3.39389200027266,5.85733573570813,115.030015841055));
#36977=CARTESIAN_POINT('Ctrl Pts',(3.23045513626465,5.94612887621698,115.038764990403));
#36978=CARTESIAN_POINT('Ctrl Pts',(3.18695122151857,5.96976399206541,115.041093854516));
#36979=CARTESIAN_POINT('Ctrl Pts',(3.14318791262796,5.99292165435265,115.043422718629));
#36980=CARTESIAN_POINT('Ctrl Pts',(3.09917575053242,6.01559628526648,115.045751582742));
#36981=CARTESIAN_POINT('Ctrl Pts',(3.09917575053269,6.01559628526634,113.045920956904));
#36982=CARTESIAN_POINT('Ctrl Pts',(2.94401221333304,6.09553500606012,113.054118808949));
#36983=CARTESIAN_POINT('Ctrl Pts',(2.78567091600791,6.16950925910911,113.062316660994));
#36984=CARTESIAN_POINT('Ctrl Pts',(2.62465241465346,6.23726612405257,113.070514513038));
#36985=CARTESIAN_POINT('Ctrl Pts',(2.4636658376091,6.30500955519091,113.078710739737));
#36986=CARTESIAN_POINT('Ctrl Pts',(2.30000344177766,6.36653790893265,113.086906966436));
#36987=CARTESIAN_POINT('Ctrl Pts',(2.1341875282734,6.42164562975584,113.095103193135));
#36988=CARTESIAN_POINT('Ctrl Pts',(1.96838476817524,6.47674897913955,113.103298769665));
#36989=CARTESIAN_POINT('Ctrl Pts',(1.80042917083192,6.52543259589629,113.111494346195));
#36990=CARTESIAN_POINT('Ctrl Pts',(1.63085998250116,6.56754023341131,113.119689922725));
#36991=CARTESIAN_POINT('Ctrl Pts',(1.46127339420084,6.60965219170901,113.127886340227));
#36992=CARTESIAN_POINT('Ctrl Pts',(1.29007323335485,6.64518673986874,113.136082757728));
#36993=CARTESIAN_POINT('Ctrl Pts',(1.11781081896515,6.67403835567376,113.144279175229));
#36994=CARTESIAN_POINT('Ctrl Pts',(0.945499387013171,6.70289818125501,113.152477925035));
#36995=CARTESIAN_POINT('Ctrl Pts',(0.772125453262238,6.72507122739405,113.160676674841));
#36996=CARTESIAN_POINT('Ctrl Pts',(0.598247420093158,6.74050361800599,113.168875424647));
#36997=CARTESIAN_POINT('Ctrl Pts',(0.424188066599475,6.75595210154252,113.177082724123));
#36998=CARTESIAN_POINT('Ctrl Pts',(0.24962392135627,6.76464585412231,113.1852900236));
#36999=CARTESIAN_POINT('Ctrl Pts',(0.0751163829015089,6.76658307634066,
113.193497323077));
#37000=CARTESIAN_POINT('Ctrl Pts',(-0.0994837912842878,6.7685213269157,
113.201708979323));
#37001=CARTESIAN_POINT('Ctrl Pts',(-0.274026940389897,6.76369590689139,
113.20992063557));
#37002=CARTESIAN_POINT('Ctrl Pts',(-0.447954916019131,6.75215709186437,
113.218132291817));
#37003=CARTESIAN_POINT('Ctrl Pts',(-0.622140531443315,6.74060118437177,
113.226356112003));
#37004=CARTESIAN_POINT('Ctrl Pts',(-0.795708795276499,6.72231204483203,
113.23457993219));
#37005=CARTESIAN_POINT('Ctrl Pts',(-0.968108587432515,6.69739163876053,
113.242803752376));
#37006=CARTESIAN_POINT('Ctrl Pts',(-1.13280871767227,6.67358421953876,113.250660283053));
#37007=CARTESIAN_POINT('Ctrl Pts',(-1.29644222447555,6.64372506606673,113.25851681373));
#37008=CARTESIAN_POINT('Ctrl Pts',(-1.45854106774237,6.6079457438533,113.266373344407));
#37009=CARTESIAN_POINT('Ctrl Pts',(-1.62671514307631,6.57082546397929,113.274524326582));
#37010=CARTESIAN_POINT('Ctrl Pts',(-1.79373539429731,6.52722256301833,113.282675308756));
#37011=CARTESIAN_POINT('Ctrl Pts',(-1.95905868094594,6.47721993486483,113.29082629093));
#37012=CARTESIAN_POINT('Ctrl Pts',(-2.1241899292746,6.42727538939828,113.298967804983));
#37013=CARTESIAN_POINT('Ctrl Pts',(-2.2876277903659,6.37094601922237,113.307109319036));
#37014=CARTESIAN_POINT('Ctrl Pts',(-2.44883825663352,6.30836588926547,113.315250833089));
#37015=CARTESIAN_POINT('Ctrl Pts',(-2.60989538659826,6.24584528277491,113.323384603292));
#37016=CARTESIAN_POINT('Ctrl Pts',(-2.76872900099205,6.17708588444185,113.331518373496));
#37017=CARTESIAN_POINT('Ctrl Pts',(-2.92481923568579,6.10227182601385,113.339652143699));
#37018=CARTESIAN_POINT('Ctrl Pts',(-3.08079383320364,6.02751319249087,113.347779888117));
#37019=CARTESIAN_POINT('Ctrl Pts',(-3.23402876944185,5.94670898761275,113.355907632534));
#37020=CARTESIAN_POINT('Ctrl Pts',(-3.38402319921984,5.86009180705746,113.364035376952));
#37021=CARTESIAN_POINT('Ctrl Pts',(-3.53393804301192,5.7735205849669,113.372158808847));
#37022=CARTESIAN_POINT('Ctrl Pts',(-3.68061548855392,5.68114271216995,113.380282240741));
#37023=CARTESIAN_POINT('Ctrl Pts',(-3.82357840007248,5.58323716301746,113.388405672635));
#37024=CARTESIAN_POINT('Ctrl Pts',(-3.96744821206923,5.48471053957093,113.396580636386));
#37025=CARTESIAN_POINT('Ctrl Pts',(-4.10755586438943,5.38058603430221,113.404755600136));
#37026=CARTESIAN_POINT('Ctrl Pts',(-4.24344345309155,5.27119309648342,113.412930563887));
#37027=CARTESIAN_POINT('Ctrl Pts',(-4.3784438277465,5.16251438836008,113.42105215306));
#37028=CARTESIAN_POINT('Ctrl Pts',(-4.50927880893989,5.04863609115681,113.429173742233));
#37029=CARTESIAN_POINT('Ctrl Pts',(-4.63553175135842,4.92992235051911,113.437295331406));
#37030=CARTESIAN_POINT('Ctrl Pts',(-4.76180136175537,4.8111929372323,113.445417992796));
#37031=CARTESIAN_POINT('Ctrl Pts',(-4.88348746182124,4.68762705970827,113.453540654185));
#37032=CARTESIAN_POINT('Ctrl Pts',(-5.00020963035672,4.55962637202741,113.461663315574));
#37033=CARTESIAN_POINT('Ctrl Pts',(-5.11696943596483,4.43158441051454,113.469788596117));
#37034=CARTESIAN_POINT('Ctrl Pts',(-5.22876187624127,4.29910506155716,113.477913876659));
#37035=CARTESIAN_POINT('Ctrl Pts',(-5.33524628096075,4.1626237064494,113.486039157201));
#37036=CARTESIAN_POINT('Ctrl Pts',(-5.44289081117468,4.02465541529691,113.494252960989));
#37037=CARTESIAN_POINT('Ctrl Pts',(-5.54511073204309,3.88259770788784,113.502466764777));
#37038=CARTESIAN_POINT('Ctrl Pts',(-5.6415991215207,3.73693033813274,113.510680568564));
#37039=CARTESIAN_POINT('Ctrl Pts',(-5.73721278734684,3.59258352823217,113.51881990942));
#37040=CARTESIAN_POINT('Ctrl Pts',(-5.82719827915468,3.44469257941896,113.526959250275));
#37041=CARTESIAN_POINT('Ctrl Pts',(-5.91130347514983,3.2937486583954,113.53509859113));
#37042=CARTESIAN_POINT('Ctrl Pts',(-5.99656282840136,3.14073336687334,113.543349626384));
#37043=CARTESIAN_POINT('Ctrl Pts',(-6.07577914989964,2.98458105505613,113.551600661638));
#37044=CARTESIAN_POINT('Ctrl Pts',(-6.1487405934437,2.82582344008568,113.559851696892));
#37045=CARTESIAN_POINT('Ctrl Pts',(-6.2217020369877,2.66706582511535,113.568102732146));
#37046=CARTESIAN_POINT('Ctrl Pts',(-6.28840851789907,2.50570328737299,113.5763537674));
#37047=CARTESIAN_POINT('Ctrl Pts',(-6.34870092747996,2.34228212079911,113.584604802654));
#37048=CARTESIAN_POINT('Ctrl Pts',(-6.41983622137832,2.14947156978188,113.594339690045));
#37049=CARTESIAN_POINT('Ctrl Pts',(-6.48222538237985,1.95330680321043,113.604074577435));
#37050=CARTESIAN_POINT('Ctrl Pts',(-6.53559110260409,1.75451929016532,113.613809464825));
#37051=CARTESIAN_POINT('Ctrl Pts',(-6.58871805857496,1.5566211748822,113.623500797231));
#37052=CARTESIAN_POINT('Ctrl Pts',(-6.63290207036377,1.35612378478015,113.633192129637));
#37053=CARTESIAN_POINT('Ctrl Pts',(-6.66791581979843,1.15377104318053,113.642883462043));
#37054=CARTESIAN_POINT('Ctrl Pts',(-6.70259748840101,0.953337475273793,
113.652482878964));
#37055=CARTESIAN_POINT('Ctrl Pts',(-6.72828196471674,0.751083656522569,
113.662082295886));
#37056=CARTESIAN_POINT('Ctrl Pts',(-6.7447946739725,0.547753417106862,113.671681712808));
#37057=CARTESIAN_POINT('Ctrl Pts',(-6.75941508395749,0.367724118670178,
113.680181069809));
#37058=CARTESIAN_POINT('Ctrl Pts',(-6.76684596472719,0.186851288175511,
113.688680426809));
#37059=CARTESIAN_POINT('Ctrl Pts',(-6.76699762927843,0.0056643923045232,
113.69717978381));
#37060=CARTESIAN_POINT('',(-6.767,6.77926383649621E-12,113.30282021619));
#37061=CARTESIAN_POINT('Ctrl Pts',(3.09917575053259,6.01559628526639,112.651392015122));
#37062=CARTESIAN_POINT('Ctrl Pts',(2.9338238445926,6.10078395293762,112.660141463035));
#37063=CARTESIAN_POINT('Ctrl Pts',(2.76495772122972,6.17915010267055,112.668890910947));
#37064=CARTESIAN_POINT('Ctrl Pts',(2.59315093316693,6.25042856433185,112.67764035886));
#37065=CARTESIAN_POINT('Ctrl Pts',(2.42134553245592,6.32170645041461,112.68638973612));
#37066=CARTESIAN_POINT('Ctrl Pts',(2.24659977927557,6.38589665313469,112.69513911338));
#37067=CARTESIAN_POINT('Ctrl Pts',(2.06950718689877,6.44278115439088,112.70388849064));
#37068=CARTESIAN_POINT('Ctrl Pts',(1.89241596572812,6.49966521519739,112.712637800154));
#37069=CARTESIAN_POINT('Ctrl Pts',(1.7129782145714,6.54924360009561,112.721387109669));
#37070=CARTESIAN_POINT('Ctrl Pts',(1.53180337335779,6.59134792173571,112.730136419184));
#37071=CARTESIAN_POINT('Ctrl Pts',(1.35062987477728,6.63345193135315,112.73888566386));
#37072=CARTESIAN_POINT('Ctrl Pts',(1.16771959102909,6.66808192368245,112.747634908536));
#37073=CARTESIAN_POINT('Ctrl Pts',(0.983693746906529,6.69512028363173,112.756384153212));
#37074=CARTESIAN_POINT('Ctrl Pts',(0.799669205419791,6.72215845218867,112.765133335956));
#37075=CARTESIAN_POINT('Ctrl Pts',(0.614529402873635,6.74160505424577,112.7738825187));
#37076=CARTESIAN_POINT('Ctrl Pts',(0.428903127363647,6.7533940435412,112.782631701445));
#37077=CARTESIAN_POINT('Ctrl Pts',(0.243278104164413,6.76518295330328,112.791380825163));
#37078=CARTESIAN_POINT('Ctrl Pts',(0.0571669005397858,6.76931433552275,
112.800129948882));
#37079=CARTESIAN_POINT('Ctrl Pts',(-0.12879840477671,6.76577415902474,112.8088790726));
#37080=CARTESIAN_POINT('Ctrl Pts',(-0.314762517258404,6.76223400523445,
112.8176281402));
#37081=CARTESIAN_POINT('Ctrl Pts',(-0.500580446818923,6.75102239665094,
112.826377207799));
#37082=CARTESIAN_POINT('Ctrl Pts',(-0.685621118842133,6.73217741012502,
112.835126275398));
#37083=CARTESIAN_POINT('Ctrl Pts',(-0.870660665413852,6.7133325382178,112.843875289784));
#37084=CARTESIAN_POINT('Ctrl Pts',(-1.05492267885408,6.68685441030624,112.85262430417));
#37085=CARTESIAN_POINT('Ctrl Pts',(-1.23778137635158,6.65283295028195,112.861373318555));
#37086=CARTESIAN_POINT('Ctrl Pts',(-1.42999922978739,6.61707018861888,112.870570128923));
#37087=CARTESIAN_POINT('Ctrl Pts',(-1.62066601233575,6.57297172934442,112.87976693929));
#37088=CARTESIAN_POINT('Ctrl Pts',(-1.80906628500253,6.52070304311331,112.888963749657));
#37089=CARTESIAN_POINT('Ctrl Pts',(-1.98831342545397,6.47097374915071,112.897713747395));
#37090=CARTESIAN_POINT('Ctrl Pts',(-2.16550875896574,6.41384933989572,112.906463745133));
#37091=CARTESIAN_POINT('Ctrl Pts',(-2.34005036713886,6.34952386240522,112.915213742871));
#37092=CARTESIAN_POINT('Ctrl Pts',(-2.51458843546966,6.28519968948645,112.923963563152));
#37093=CARTESIAN_POINT('Ctrl Pts',(-2.68647261717933,6.21367483971152,112.932713383432));
#37094=CARTESIAN_POINT('Ctrl Pts',(-2.85511905908611,6.135192267439,112.941463203713));
#37095=CARTESIAN_POINT('Ctrl Pts',(-3.0237623048876,6.05671118252999,112.950212858172));
#37096=CARTESIAN_POINT('Ctrl Pts',(-3.18916767379777,5.97127275992701,112.95896251263));
#37097=CARTESIAN_POINT('Ctrl Pts',(-3.35077334102657,5.87916720438071,112.967712167089));
#37098=CARTESIAN_POINT('Ctrl Pts',(-3.51237616037249,5.78706327195715,112.976461667357));
#37099=CARTESIAN_POINT('Ctrl Pts',(-3.67017916302192,5.68829258362368,112.985211167626));
#37100=CARTESIAN_POINT('Ctrl Pts',(-3.82364636566365,5.58319061741109,112.993960667894));
#37101=CARTESIAN_POINT('Ctrl Pts',(-3.97711106778699,5.47809036367774,113.002710025603));
#37102=CARTESIAN_POINT('Ctrl Pts',(-4.12623987481826,5.36665920043302,113.011459383311));
#37103=CARTESIAN_POINT('Ctrl Pts',(-4.27052628213827,5.24927559512418,113.02020874102));
#37104=CARTESIAN_POINT('Ctrl Pts',(-4.41481053024875,5.13189374643125,113.028957967796));
#37105=CARTESIAN_POINT('Ctrl Pts',(-4.55425230136427,5.00855981477447,113.037707194573));
#37106=CARTESIAN_POINT('Ctrl Pts',(-4.68837800630445,4.87969268192176,113.046456421349));
#37107=CARTESIAN_POINT('Ctrl Pts',(-4.822501882288,4.75082730631905,113.05520552882));
#37108=CARTESIAN_POINT('Ctrl Pts',(-4.95130963052881,4.61642907903617,113.063954636291));
#37109=CARTESIAN_POINT('Ctrl Pts',(-5.07436379033291,4.47695444731776,113.072703743762));
#37110=CARTESIAN_POINT('Ctrl Pts',(-5.19741643562739,4.33748153220666,113.081452743551));
#37111=CARTESIAN_POINT('Ctrl Pts',(-5.31471544462716,4.19293255254661,113.090201743341));
#37112=CARTESIAN_POINT('Ctrl Pts',(-5.4258624527558,4.04379841779667,113.098950743131));
#37113=CARTESIAN_POINT('Ctrl Pts',(-5.53702160019108,3.89464799484406,113.107700698473));
#37114=CARTESIAN_POINT('Ctrl Pts',(-5.6420272308121,3.74091164443912,113.116450653815));
#37115=CARTESIAN_POINT('Ctrl Pts',(-5.74052265232929,3.58311159163293,113.125200609157));
#37116=CARTESIAN_POINT('Ctrl Pts',(-5.83901427066882,3.42531763191845,113.13395022664));
#37117=CARTESIAN_POINT('Ctrl Pts',(-5.93099603115705,3.26346052695676,113.142699844122));
#37118=CARTESIAN_POINT('Ctrl Pts',(-6.01615550622721,3.0980900446714,113.151449461605));
#37119=CARTESIAN_POINT('Ctrl Pts',(-6.10131214578765,2.932725068639,113.160198787756));
#37120=CARTESIAN_POINT('Ctrl Pts',(-6.17964682328711,2.76384720416975,113.168948113907));
#37121=CARTESIAN_POINT('Ctrl Pts',(-6.25089348288527,2.59203002791682,113.177697440058));
#37122=CARTESIAN_POINT('Ctrl Pts',(-6.32213814889296,2.42021765937118,113.18644652139));
#37123=CARTESIAN_POINT('Ctrl Pts',(-6.38629508412554,2.24546640832007,113.195195602721));
#37124=CARTESIAN_POINT('Ctrl Pts',(-6.44314639819783,2.06836976660131,113.203944684053));
#37125=CARTESIAN_POINT('Ctrl Pts',(-6.50000285283673,1.89125711158368,113.212694556487));
#37126=CARTESIAN_POINT('Ctrl Pts',(-6.54955227673224,1.71179891440351,113.221444428922));
#37127=CARTESIAN_POINT('Ctrl Pts',(-6.59162635926362,1.5306047627853,113.230194301356));
#37128=CARTESIAN_POINT('Ctrl Pts',(-6.63369752055177,1.34942319164793,113.238943566278));
#37129=CARTESIAN_POINT('Ctrl Pts',(-6.66829431424237,1.16650618642799,113.247692831201));
#37130=CARTESIAN_POINT('Ctrl Pts',(-6.69529923745404,0.982474997619488,
113.256442096123));
#37131=CARTESIAN_POINT('Ctrl Pts',(-6.72230554731432,0.79843435917869,113.265191810303));
#37132=CARTESIAN_POINT('Ctrl Pts',(-6.74171916496694,0.613279706241307,
113.273941524483));
#37133=CARTESIAN_POINT('Ctrl Pts',(-6.75347414817269,0.427639953656364,
113.282691238662));
#37134=CARTESIAN_POINT('Ctrl Pts',(-6.76248837758731,0.285283364200966,
113.289400897838));
#37135=CARTESIAN_POINT('Ctrl Pts',(-6.76699999999986,0.142641701108919,
113.296110557014));
#37136=CARTESIAN_POINT('Ctrl Pts',(-6.767,6.77926379006094E-12,113.30282021619));
#37137=CARTESIAN_POINT('Ctrl Pts',(-6.76699998064072,-0.000511867680200162,
113.30282021619));
#37138=CARTESIAN_POINT('Ctrl Pts',(-6.76698592553831,-0.186323321307884,
113.3115153707));
#37139=CARTESIAN_POINT('Ctrl Pts',(-6.75931444471214,-0.371956404917808,
113.320210525209));
#37140=CARTESIAN_POINT('Ctrl Pts',(-6.74405514830971,-0.556784659053514,
113.328905679719));
#37141=CARTESIAN_POINT('Ctrl Pts',(-6.72877104404935,-0.741913398411343,
113.337614970409));
#37142=CARTESIAN_POINT('Ctrl Pts',(-6.7058745076392,-0.926234409616834,
113.346324261098));
#37143=CARTESIAN_POINT('Ctrl Pts',(-6.67548653246502,-1.10912963844545,
113.355033551788));
#37144=CARTESIAN_POINT('Ctrl Pts',(-6.64501723535388,-1.29251431726821,
113.363766149604));
#37145=CARTESIAN_POINT('Ctrl Pts',(-6.60701643970961,-1.47446529659286,
113.37249874742));
#37146=CARTESIAN_POINT('Ctrl Pts',(-6.56165615842634,-1.65437524721139,
113.381231345237));
#37147=CARTESIAN_POINT('Ctrl Pts',(-6.51623406590506,-1.83453035629151,
113.38997584273));
#37148=CARTESIAN_POINT('Ctrl Pts',(-6.46343254003278,-2.01263860755329,
113.398720340222));
#37149=CARTESIAN_POINT('Ctrl Pts',(-6.40347279474744,-2.18810995311695,
113.407464837715));
#37150=CARTESIAN_POINT('Ctrl Pts',(-6.34337008561044,-2.36399968036815,
113.416230184981));
#37151=CARTESIAN_POINT('Ctrl Pts',(-6.27607511803839,-2.53723965654339,
113.424995532246));
#37152=CARTESIAN_POINT('Ctrl Pts',(-6.20185744489644,-2.70725935831471,
113.433760879511));
#37153=CARTESIAN_POINT('Ctrl Pts',(-6.13987808394496,-2.84924322844755,
113.441080842521));
#37154=CARTESIAN_POINT('Ctrl Pts',(-6.07307173041068,-2.98898164504308,
113.44840080553));
#37155=CARTESIAN_POINT('Ctrl Pts',(-6.00161913178858,-3.12615687337493,
113.455720768539));
#37156=CARTESIAN_POINT('Ctrl Pts',(-5.92203931340429,-3.27893479843274,
113.463873324752));
#37157=CARTESIAN_POINT('Ctrl Pts',(-5.83649751417518,-3.42891101393908,
113.472025880965));
#37158=CARTESIAN_POINT('Ctrl Pts',(-5.74521528562023,-3.57558251504222,
113.480178437179));
#37159=CARTESIAN_POINT('Ctrl Pts',(-5.65403880972769,-3.72208409367538,
113.488321548459));
#37160=CARTESIAN_POINT('Ctrl Pts',(-5.55713533400066,-3.86528827189059,
113.496464659739));
#37161=CARTESIAN_POINT('Ctrl Pts',(-5.45477343638876,-4.00471419175796,
113.50460777102));
#37162=CARTESIAN_POINT('Ctrl Pts',(-5.35250860718878,-4.14400789589918,
113.512743160297));
#37163=CARTESIAN_POINT('Ctrl Pts',(-5.24479587600462,-4.27953018208464,
113.520878549574));
#37164=CARTESIAN_POINT('Ctrl Pts',(-5.13194847685834,-4.41082688742954,
113.529013938852));
#37165=CARTESIAN_POINT('Ctrl Pts',(-5.01918437742275,-4.542026674479,113.53714332289));
#37166=CARTESIAN_POINT('Ctrl Pts',(-4.90129339429023,-4.66900681542773,
113.545272706929));
#37167=CARTESIAN_POINT('Ctrl Pts',(-4.77863060131114,-4.7913441304307,113.553402090968));
#37168=CARTESIAN_POINT('Ctrl Pts',(-4.65603258834482,-4.91361683731059,
113.56152718176));
#37169=CARTESIAN_POINT('Ctrl Pts',(-4.52866804259884,-5.03125134382306,
113.569652272552));
#37170=CARTESIAN_POINT('Ctrl Pts',(-4.39693064433775,-5.14385943712342,
113.577777363344));
#37171=CARTESIAN_POINT('Ctrl Pts',(-4.26469037586874,-5.2568973799277,113.585933469369));
#37172=CARTESIAN_POINT('Ctrl Pts',(-4.12804405328261,-5.36487018279817,
113.594089575394));
#37173=CARTESIAN_POINT('Ctrl Pts',(-3.98742575639107,-5.46742396721428,
113.602245681419));
#37174=CARTESIAN_POINT('Ctrl Pts',(-3.84737342271321,-5.56956499119532,
113.610368960593));
#37175=CARTESIAN_POINT('Ctrl Pts',(-3.7033813386149,-5.66633033724267,113.618492239766));
#37176=CARTESIAN_POINT('Ctrl Pts',(-3.55590960036512,-5.75741225847439,
113.62661551894));
#37177=CARTESIAN_POINT('Ctrl Pts',(-3.40841822500729,-5.84850630803355,
113.634739879796));
#37178=CARTESIAN_POINT('Ctrl Pts',(-3.25744658387856,-5.93391523312716,
113.642864240653));
#37179=CARTESIAN_POINT('Ctrl Pts',(-3.10348157311169,-6.01337601729313,
113.65098860151));
#37180=CARTESIAN_POINT('Ctrl Pts',(-2.949466767967,-6.09286250015706,113.659115589895));
#37181=CARTESIAN_POINT('Ctrl Pts',(-2.7924569903133,-6.16639684369086,113.667242578281));
#37182=CARTESIAN_POINT('Ctrl Pts',(-2.63296136991059,-6.23376318322717,
113.675369566666));
#37183=CARTESIAN_POINT('Ctrl Pts',(-2.47243462848122,-6.30156503847865,
113.683549095106));
#37184=CARTESIAN_POINT('Ctrl Pts',(-2.3093901376982,-6.36311871612374,113.691728623546));
#37185=CARTESIAN_POINT('Ctrl Pts',(-2.14436396617238,-6.41825460546569,
113.699908151986));
#37186=CARTESIAN_POINT('Ctrl Pts',(-1.98011495608991,-6.47313084212984,
113.70804916039));
#37187=CARTESIAN_POINT('Ctrl Pts',(-1.81390325858461,-6.52164956662919,
113.716190168794));
#37188=CARTESIAN_POINT('Ctrl Pts',(-1.64626880851799,-6.56369469202375,
113.724331177197));
#37189=CARTESIAN_POINT('Ctrl Pts',(-1.47744458843913,-6.6060382288089,113.732529965656));
#37190=CARTESIAN_POINT('Ctrl Pts',(-1.30717771530874,-6.64181585954267,
113.740728754114));
#37191=CARTESIAN_POINT('Ctrl Pts',(-1.13602575965488,-6.67096203507414,
113.748927542572));
#37192=CARTESIAN_POINT('Ctrl Pts',(-0.964873804000891,-6.70010821060564,
113.75712633103));
#37193=CARTESIAN_POINT('Ctrl Pts',(-0.792837142456745,-6.72262294697997,
113.765325119489));
#37194=CARTESIAN_POINT('Ctrl Pts',(-0.620473771617619,-6.73849399337379,
113.773523907947));
#37195=CARTESIAN_POINT('Ctrl Pts',(-0.447390116603392,-6.75443136281237,
113.781756958079));
#37196=CARTESIAN_POINT('Ctrl Pts',(-0.273438990090556,-6.76371906131375,
113.789990008211));
#37197=CARTESIAN_POINT('Ctrl Pts',(-0.0991722470327019,-6.76627326269184,
113.798223058343));
#37198=CARTESIAN_POINT('Ctrl Pts',(0.0748869711218329,-6.76882442240872,
113.806446304178));
#37199=CARTESIAN_POINT('Ctrl Pts',(0.249260702779041,-6.76465804674041,
113.814669550013));
#37200=CARTESIAN_POINT('Ctrl Pts',(0.423390610029359,-6.75374188071612,
113.822892795847));
#37201=CARTESIAN_POINT('Ctrl Pts',(0.597348007803099,-6.74283652927342,
113.831107894961));
#37202=CARTESIAN_POINT('Ctrl Pts',(0.771061707207564,-6.7251947269294,113.839322994074));
#37203=CARTESIAN_POINT('Ctrl Pts',(0.943971899508641,-6.70083622042339,
113.847538093188));
#37204=CARTESIAN_POINT('Ctrl Pts',(1.11674538654388,-6.67649697210028,113.855746697327));
#37205=CARTESIAN_POINT('Ctrl Pts',(1.28871627871096,-6.6454516464543,113.863955301466));
#37206=CARTESIAN_POINT('Ctrl Pts',(1.45932832718849,-6.60777192656233,113.872163905605));
#37207=CARTESIAN_POINT('Ctrl Pts',(1.62983961451151,-6.57011445980026,113.880367661854));
#37208=CARTESIAN_POINT('Ctrl Pts',(1.79899330804695,-6.52583048138147,113.888571418103));
#37209=CARTESIAN_POINT('Ctrl Pts',(1.9662417189917,-6.47504305024272,113.896775174351));
#37210=CARTESIAN_POINT('Ctrl Pts',(2.1334406453472,-6.42427064582474,113.904976503316));
#37211=CARTESIAN_POINT('Ctrl Pts',(2.29873506861704,-6.36699872188743,113.91317783228));
#37212=CARTESIAN_POINT('Ctrl Pts',(2.46159062951145,-6.3034007149079,113.921379161244));
#37213=CARTESIAN_POINT('Ctrl Pts',(2.62442373106923,-6.2398114787007,113.929579359167));
#37214=CARTESIAN_POINT('Ctrl Pts',(2.78481830621493,-6.16989802656108,113.93777955709));
#37215=CARTESIAN_POINT('Ctrl Pts',(2.94225819567853,-6.09388264655322,113.945979755012));
#37216=CARTESIAN_POINT('Ctrl Pts',(3.09970490398974,-6.01786397425843,113.954180308092));
#37217=CARTESIAN_POINT('Ctrl Pts',(3.25419634898187,-5.93574300332145,113.962380861172));
#37218=CARTESIAN_POINT('Ctrl Pts',(3.40523922879428,-5.84778888082329,113.970581414252));
#37219=CARTESIAN_POINT('Ctrl Pts',(3.55631602232321,-5.75981500995182,113.978783808605));
#37220=CARTESIAN_POINT('Ctrl Pts',(3.7039423989177,-5.66600555918314,113.986986202958));
#37221=CARTESIAN_POINT('Ctrl Pts',(3.84765234961335,-5.56667408750637,113.995188597312));
#37222=CARTESIAN_POINT('Ctrl Pts',(3.99149669437555,-5.46724972344219,114.003398662345));
#37223=CARTESIAN_POINT('Ctrl Pts',(4.13141700066247,-5.36229322508902,114.011608727379));
#37224=CARTESIAN_POINT('Ctrl Pts',(4.26697804002371,-5.25216026087889,114.019818792413));
#37225=CARTESIAN_POINT('Ctrl Pts',(4.40260395649353,-5.14197458898586,114.028032786638));
#37226=CARTESIAN_POINT('Ctrl Pts',(4.53386617739443,-5.0266077481711,114.036246780864));
#37227=CARTESIAN_POINT('Ctrl Pts',(4.66036500088654,-4.90645361320291,114.044460775089));
#37228=CARTESIAN_POINT('Ctrl Pts',(4.78703628440682,-4.78613566813017,114.052685967724));
#37229=CARTESIAN_POINT('Ctrl Pts',(4.90893094189138,-4.66101764195539,114.060911160359));
#37230=CARTESIAN_POINT('Ctrl Pts',(5.02568754258432,-4.53152885065435,114.069136352994));
#37231=CARTESIAN_POINT('Ctrl Pts',(5.1306865035162,-4.41507985797864,114.076533251114));
#37232=CARTESIAN_POINT('Ctrl Pts',(5.23153055144813,-4.29509665962651,114.083930149234));
#37233=CARTESIAN_POINT('Ctrl Pts',(5.32798648012009,-4.17191191993042,114.091327047354));
#37234=CARTESIAN_POINT('Ctrl Pts',(5.44073032404227,-4.02792573621825,114.099973013845));
#37235=CARTESIAN_POINT('Ctrl Pts',(5.5477344538295,-3.8792383743941,114.108618980336));
#37236=CARTESIAN_POINT('Ctrl Pts',(5.64861059834346,-3.72632356462532,114.117264946827));
#37237=CARTESIAN_POINT('Ctrl Pts',(5.74935770855487,-3.57360435368641,114.125899853951));
#37238=CARTESIAN_POINT('Ctrl Pts',(5.84399229685624,-3.41666873097097,114.134534761076));
#37239=CARTESIAN_POINT('Ctrl Pts',(5.93216732888985,-3.25602207947855,114.1431696682));
#37240=CARTESIAN_POINT('Ctrl Pts',(6.02326970081915,-3.0900420888177,114.152091247272));
#37241=CARTESIAN_POINT('Ctrl Pts',(6.10747602102705,-2.92010066302637,114.161012826343));
#37242=CARTESIAN_POINT('Ctrl Pts',(6.18445149906859,-2.74678878978131,114.169934405415));
#37243=CARTESIAN_POINT('Ctrl Pts',(6.2587478064584,-2.57950912440569,114.17854546439));
#37244=CARTESIAN_POINT('Ctrl Pts',(6.32630795757735,-2.4090899766247,114.187156523366));
#37245=CARTESIAN_POINT('Ctrl Pts',(6.38687675112069,-2.23608907827796,114.195767582342));
#37246=CARTESIAN_POINT('Ctrl Pts',(6.44738842549554,-2.06325132776503,114.204370520691));
#37247=CARTESIAN_POINT('Ctrl Pts',(6.50092178691575,-1.8878369677393,114.212973459041));
#37248=CARTESIAN_POINT('Ctrl Pts',(6.54726957670759,-1.7104239503466,114.22157639739));
#37249=CARTESIAN_POINT('Ctrl Pts',(6.59356546769672,-1.53320959449155,114.230169702439));
#37250=CARTESIAN_POINT('Ctrl Pts',(6.63269176204127,-1.35400134051198,114.238763007488));
#37251=CARTESIAN_POINT('Ctrl Pts',(6.66449085979511,-1.17339276446867,114.247356312536));
#37252=CARTESIAN_POINT('Ctrl Pts',(6.66803379978303,-1.15327001283657,114.248313747377));
#37253=CARTESIAN_POINT('Ctrl Pts',(6.67148583384404,-1.13312989349662,114.249271182217));
#37254=CARTESIAN_POINT('Ctrl Pts',(6.67484678254197,-1.11297323848738,114.250228617058));
#37255=CARTESIAN_POINT('Ctrl Pts',(6.70502105541736,-0.932008736149903,
114.258824374606));
#37256=CARTESIAN_POINT('Ctrl Pts',(6.727814051586,-0.749922628110056,114.267420132153));
#37257=CARTESIAN_POINT('Ctrl Pts',(6.7431764123795,-0.567327834262293,114.276015889701));
#37258=CARTESIAN_POINT('Ctrl Pts',(6.75855310677793,-0.384562673263889,
114.284619667382));
#37259=CARTESIAN_POINT('Ctrl Pts',(6.7664853016141,-0.201288183326025,114.293223445064));
#37260=CARTESIAN_POINT('Ctrl Pts',(6.76697574324738,-0.0181187831159108,
114.301827222746));
#37261=CARTESIAN_POINT('Ctrl Pts',(6.76748545966571,0.17224933469393,114.310769136414));
#37262=CARTESIAN_POINT('Ctrl Pts',(6.75995667130892,0.362503558851308,114.319711050082));
#37263=CARTESIAN_POINT('Ctrl Pts',(6.74445175682765,0.551959690398153,114.32865296375));
#37264=CARTESIAN_POINT('Ctrl Pts',(6.72949253900064,0.734747898865666,114.33728016608));
#37265=CARTESIAN_POINT('Ctrl Pts',(6.70710915170723,0.916792946695289,114.345907368411));
#37266=CARTESIAN_POINT('Ctrl Pts',(6.67741002177307,1.09749004602529,114.354534570742));
#37267=CARTESIAN_POINT('Ctrl Pts',(6.64768260796348,1.27835923168437,114.363169989162));
#37268=CARTESIAN_POINT('Ctrl Pts',(6.61062560311362,1.45787760733531,114.371805407583));
#37269=CARTESIAN_POINT('Ctrl Pts',(6.56639806318465,1.63545268222744,114.380440826003));
#37270=CARTESIAN_POINT('Ctrl Pts',(6.5221051833651,1.81329009899932,114.389089002024));
#37271=CARTESIAN_POINT('Ctrl Pts',(6.47062068069418,1.98917818406113,114.397737178045));
#37272=CARTESIAN_POINT('Ctrl Pts',(6.41215320994172,2.16254022210782,114.406385354067));
#37273=CARTESIAN_POINT('Ctrl Pts',(6.40596757322697,2.18088126839705,114.407300298298));
#37274=CARTESIAN_POINT('Ctrl Pts',(6.39970382132123,2.19919406032554,114.40821524253));
#37275=CARTESIAN_POINT('Ctrl Pts',(6.39336223237251,2.21747792901593,114.409130186762));
#37276=CARTESIAN_POINT('Ctrl Pts',(6.33633806085052,2.38188821683459,114.417357452393));
#37277=CARTESIAN_POINT('Ctrl Pts',(6.27289305289448,2.54431328152196,114.425584718025));
#37278=CARTESIAN_POINT('Ctrl Pts',(6.20318477630388,2.70421663907161,114.433811983656));
#37279=CARTESIAN_POINT('Ctrl Pts',(6.13355192339866,2.86394698272506,114.442030347465));
#37280=CARTESIAN_POINT('Ctrl Pts',(6.05766944069756,3.02116072729144,114.450248711274));
#37281=CARTESIAN_POINT('Ctrl Pts',(5.97574437115397,3.1753374955462,114.458467075083));
#37282=CARTESIAN_POINT('Ctrl Pts',(5.89390505274607,3.32935288666638,114.466676836714));
#37283=CARTESIAN_POINT('Ctrl Pts',(5.80603592069383,3.48033732246086,114.474886598345));
#37284=CARTESIAN_POINT('Ctrl Pts',(5.71239160679545,3.62779149491986,114.483096359977));
#37285=CARTESIAN_POINT('Ctrl Pts',(5.6188031726874,3.77515767796556,114.491301222648));
#37286=CARTESIAN_POINT('Ctrl Pts',(5.5194466102212,3.91899749110032,114.499506085318));
#37287=CARTESIAN_POINT('Ctrl Pts',(5.41462210654726,4.05883683378498,114.507710947989));
#37288=CARTESIAN_POINT('Ctrl Pts',(5.30984115660537,4.19861807435566,114.515912401606));
#37289=CARTESIAN_POINT('Ctrl Pts',(5.19959700470538,4.33440186885736,114.524113855223));
#37290=CARTESIAN_POINT('Ctrl Pts',(5.08423275478234,4.46574364414242,114.53231530884));
#37291=CARTESIAN_POINT('Ctrl Pts',(4.96889553121661,4.59705465001883,114.540514841105));
#37292=CARTESIAN_POINT('Ctrl Pts',(4.84844083572215,4.72392544117365,114.548714373369));
#37293=CARTESIAN_POINT('Ctrl Pts',(4.72325163232275,4.84594500771114,114.556913905633));
#37294=CARTESIAN_POINT('Ctrl Pts',(4.59803605321582,4.96799028215564,114.56511516543));
#37295=CARTESIAN_POINT('Ctrl Pts',(4.46808422538635,5.0851820351484,114.573316425228));
#37296=CARTESIAN_POINT('Ctrl Pts',(4.33381586545243,5.19714624042395,114.581517685025));
#37297=CARTESIAN_POINT('Ctrl Pts',(4.19953598187009,5.30912005508282,114.589719648699));
#37298=CARTESIAN_POINT('Ctrl Pts',(4.06093910691309,5.41586520299029,114.597921612373));
#37299=CARTESIAN_POINT('Ctrl Pts',(3.918477552277,5.51704836595632,114.606123576048));
#37300=CARTESIAN_POINT('Ctrl Pts',(3.77591697650975,5.61830185857217,114.614331240683));
#37301=CARTESIAN_POINT('Ctrl Pts',(3.62948664892684,5.71398543803148,114.622538905318));
#37302=CARTESIAN_POINT('Ctrl Pts',(3.47966797528055,5.80380907523731,114.630746569953));
#37303=CARTESIAN_POINT('Ctrl Pts',(3.35508327882642,5.87850370644273,114.637571816648));
#37304=CARTESIAN_POINT('Ctrl Pts',(3.22815610505373,5.94914688140496,114.644397063343));
#37305=CARTESIAN_POINT('Ctrl Pts',(3.09917575053242,6.01559628526648,114.651222310038));
#37306=CARTESIAN_POINT('Origin',(0.,0.,-3.69717978381041));
#37307=CARTESIAN_POINT('',(3.09917575053267,6.01559628526635,117.045557306694));
#37308=CARTESIAN_POINT('',(3.09917575053275,6.01559628526631,116.651505798254));
#37309=CARTESIAN_POINT('',(3.09917575053259,6.01559628526639,-3.69717978381041));
#37310=CARTESIAN_POINT('',(-6.76775516591789,-0.00305449199090704,115.695870839299));
#37311=CARTESIAN_POINT('Ctrl Pts',(-6.76699709111062,-0.00627446415628204,
115.69717978381));
#37312=CARTESIAN_POINT('Ctrl Pts',(-6.76680730651523,-0.210956772148241,
115.706766886024));
#37313=CARTESIAN_POINT('Ctrl Pts',(-6.75732645171492,-0.415249572054033,
115.716353988239));
#37314=CARTESIAN_POINT('Ctrl Pts',(-6.73868767582741,-0.618366725860837,
115.725941090453));
#37315=CARTESIAN_POINT('Ctrl Pts',(-6.72065192928063,-0.81491233204604,
115.735218016507));
#37316=CARTESIAN_POINT('Ctrl Pts',(-6.69404169089617,-1.01035708318455,
115.744494942562));
#37317=CARTESIAN_POINT('Ctrl Pts',(-6.65902800631947,-1.20400789492969,
115.753771868617));
#37318=CARTESIAN_POINT('Ctrl Pts',(-6.62225828582773,-1.40737084592869,
115.763514058911));
#37319=CARTESIAN_POINT('Ctrl Pts',(-6.57622078574109,-1.60875504036215,
115.773256249205));
#37320=CARTESIAN_POINT('Ctrl Pts',(-6.52116985770305,-1.80738282800996,
115.782998439499));
#37321=CARTESIAN_POINT('Ctrl Pts',(-6.466118929665,-2.00601061565777,115.792740629794));
#37322=CARTESIAN_POINT('Ctrl Pts',(-6.40205474218278,-2.20188183374535,
115.802482820088));
#37323=CARTESIAN_POINT('Ctrl Pts',(-6.32928672348502,-2.3942469738764,115.812225010382));
#37324=CARTESIAN_POINT('Ctrl Pts',(-6.26780057684206,-2.55678803829943,
115.820456782413));
#37325=CARTESIAN_POINT('Ctrl Pts',(-6.19995887359178,-2.71719767811901,
115.828688554444));
#37326=CARTESIAN_POINT('Ctrl Pts',(-6.12592773741431,-2.87494319178276,
115.836920326475));
#37327=CARTESIAN_POINT('Ctrl Pts',(-6.0519850018116,-3.03250034153918,115.845142268947));
#37328=CARTESIAN_POINT('Ctrl Pts',(-5.9718677008018,-3.18739937853694,115.85336421142));
#37329=CARTESIAN_POINT('Ctrl Pts',(-5.88579116493238,-3.33912434072227,
115.861586153892));
#37330=CARTESIAN_POINT('Ctrl Pts',(-5.79980016685805,-3.49069852757035,
115.869799925882));
#37331=CARTESIAN_POINT('Ctrl Pts',(-5.70786190302352,-3.63910461169729,
115.878013697872));
#37332=CARTESIAN_POINT('Ctrl Pts',(-5.61023910391608,-3.78384806736355,
115.886227469862));
#37333=CARTESIAN_POINT('Ctrl Pts',(-5.51269376411958,-3.92847667559212,
115.894434724592));
#37334=CARTESIAN_POINT('Ctrl Pts',(-5.40947307228732,-4.06944814802103,
115.902641979322));
#37335=CARTESIAN_POINT('Ctrl Pts',(-5.30088489756532,-4.20629389163001,
115.910849234053));
#37336=CARTESIAN_POINT('Ctrl Pts',(-5.19236113966223,-4.34305845542814,
115.919051620065));
#37337=CARTESIAN_POINT('Ctrl Pts',(-5.07847646411138,-4.47570188612679,
115.927254006077));
#37338=CARTESIAN_POINT('Ctrl Pts',(-4.95958118534052,-4.60378577542617,
115.935456392089));
#37339=CARTESIAN_POINT('Ctrl Pts',(-4.84072139392669,-4.73183143479114,
115.943656329887));
#37340=CARTESIAN_POINT('Ctrl Pts',(-4.71685421897549,-4.85531999872025,
115.951856267686));
#37341=CARTESIAN_POINT('Ctrl Pts',(-4.58836943354913,-4.97384709669206,
115.960056205485));
#37342=CARTESIAN_POINT('Ctrl Pts',(-4.45990261361194,-5.09235762151641,
115.96825499672));
#37343=CARTESIAN_POINT('Ctrl Pts',(-4.32681973192093,-5.20590781851671,
115.976453787956));
#37344=CARTESIAN_POINT('Ctrl Pts',(-4.18954651542873,-5.31413106679342,
115.984652579192));
#37345=CARTESIAN_POINT('Ctrl Pts',(-4.05226759120111,-5.42235881492585,
115.992851711328));
#37346=CARTESIAN_POINT('Ctrl Pts',(-3.91079826650141,-5.52525895108938,
116.001050843465));
#37347=CARTESIAN_POINT('Ctrl Pts',(-3.76559639038595,-5.62250592038037,
116.009249975601));
#37348=CARTESIAN_POINT('Ctrl Pts',(-3.62036213658901,-5.71977457418041,
116.017450936012));
#37349=CARTESIAN_POINT('Ctrl Pts',(-3.47139397142424,-5.81138735101325,
116.025651896423));
#37350=CARTESIAN_POINT('Ctrl Pts',(-3.31917772249466,-5.89706267954608,
116.033852856834));
#37351=CARTESIAN_POINT('Ctrl Pts',(-3.16681881029716,-5.98281830648616,
116.042061503519));
#37352=CARTESIAN_POINT('Ctrl Pts',(-3.01120604489765,-6.06262519092112,
116.050270150204));
#37353=CARTESIAN_POINT('Ctrl Pts',(-2.85284963880841,-6.13624787132583,
116.058478796889));
#37354=CARTESIAN_POINT('Ctrl Pts',(-2.69441762892312,-6.20990570126601,
116.066691362613));
#37355=CARTESIAN_POINT('Ctrl Pts',(-2.53323969710407,-6.27737330204125,
116.074903928336));
#37356=CARTESIAN_POINT('Ctrl Pts',(-2.36984484701867,-6.33846388339155,
116.08311649406));
#37357=CARTESIAN_POINT('Ctrl Pts',(-2.2062257956211,-6.39963828983483,116.091340328608));
#37358=CARTESIAN_POINT('Ctrl Pts',(-2.04038408696616,-6.45441807669556,
116.099564163157));
#37359=CARTESIAN_POINT('Ctrl Pts',(-1.8728638419333,-6.5026663784619,116.107787997706));
#37360=CARTESIAN_POINT('Ctrl Pts',(-1.71894424878949,-6.54699749185239,
116.11534415468));
#37361=CARTESIAN_POINT('Ctrl Pts',(-1.5636079609306,-6.58581516289413,116.122900311654));
#37362=CARTESIAN_POINT('Ctrl Pts',(-1.40728280485742,-6.61905160178954,
116.130456468629));
#37363=CARTESIAN_POINT('Ctrl Pts',(-1.22841632173521,-6.65708057349225,
116.139102186681));
#37364=CARTESIAN_POINT('Ctrl Pts',(-1.047847489858,-6.68788907397469,116.147747904733));
#37365=CARTESIAN_POINT('Ctrl Pts',(-0.866172348406481,-6.71133626507091,
116.156393622786));
#37366=CARTESIAN_POINT('Ctrl Pts',(-0.684730440812389,-6.73475335475216,
116.165028241498));
#37367=CARTESIAN_POINT('Ctrl Pts',(-0.502185356772583,-6.75082794082531,
116.17366286021));
#37368=CARTESIAN_POINT('Ctrl Pts',(-0.319143471558151,-6.75947013045859,
116.182297478923));
#37369=CARTESIAN_POINT('Ctrl Pts',(-0.129637258018095,-6.76841752865752,
116.191237038825));
#37370=CARTESIAN_POINT('Ctrl Pts',(0.0604011792848513,-6.76939788746322,
116.200176598727));
#37371=CARTESIAN_POINT('Ctrl Pts',(0.250289741133326,-6.76236970635911,
116.20911615863));
#37372=CARTESIAN_POINT('Ctrl Pts',(0.433191873223424,-6.75560010793705,
116.2177268119));
#37373=CARTESIAN_POINT('Ctrl Pts',(0.615954612343275,-6.74140072917829,
116.226337465171));
#37374=CARTESIAN_POINT('Ctrl Pts',(0.797964871851218,-6.71978727812804,
116.234948118441));
#37375=CARTESIAN_POINT('Ctrl Pts',(0.979802846471547,-6.69819428565522,
116.243550621152));
#37376=CARTESIAN_POINT('Ctrl Pts',(1.16088945969433,-6.66920124857419,116.252153123864));
#37377=CARTESIAN_POINT('Ctrl Pts',(1.34061451440626,-6.63287582604735,116.260755626575));
#37378=CARTESIAN_POINT('Ctrl Pts',(1.52013729218686,-6.59659128705235,116.269348447342));
#37379=CARTESIAN_POINT('Ctrl Pts',(1.69830127025123,-6.55299088630148,116.27794126811));
#37380=CARTESIAN_POINT('Ctrl Pts',(1.87450402870215,-6.50219375644708,116.286534088877));
#37381=CARTESIAN_POINT('Ctrl Pts',(1.89527032414664,-6.4962070839593,116.287546791835));
#37382=CARTESIAN_POINT('Ctrl Pts',(1.91600938847612,-6.49012050984338,116.288559494794));
#37383=CARTESIAN_POINT('Ctrl Pts',(1.93672024385675,-6.48393427611936,116.289572197752));
#37384=CARTESIAN_POINT('Ctrl Pts',(2.11250243048391,-6.43142897534787,116.298167455512));
#37385=CARTESIAN_POINT('Ctrl Pts',(2.28604463769046,-6.37180217845666,116.306762713272));
#37386=CARTESIAN_POINT('Ctrl Pts',(2.45677480068814,-6.30527926254689,116.315357971032));
#37387=CARTESIAN_POINT('Ctrl Pts',(2.62766484524282,-6.23869405074759,116.323961277887));
#37388=CARTESIAN_POINT('Ctrl Pts',(2.79573730478657,-6.16519994052419,116.332564584741));
#37389=CARTESIAN_POINT('Ctrl Pts',(2.96044169954073,-6.08506975667662,116.341167891596));
#37390=CARTESIAN_POINT('Ctrl Pts',(3.13197479561537,-6.00161734762025,116.350127894536));
#37391=CARTESIAN_POINT('Ctrl Pts',(3.29985425666727,-5.91096705046701,116.359087897476));
#37392=CARTESIAN_POINT('Ctrl Pts',(3.4634895674056,-5.81347822017702,116.368047900416));
#37393=CARTESIAN_POINT('Ctrl Pts',(3.6210404273729,-5.71961431647499,116.37667474362));
#37394=CARTESIAN_POINT('Ctrl Pts',(3.77465684366746,-5.61941146417097,116.385301586825));
#37395=CARTESIAN_POINT('Ctrl Pts',(3.92384355705187,-5.51323323828972,116.39392843003));
#37396=CARTESIAN_POINT('Ctrl Pts',(4.07317285522284,-5.40695353286427,116.402563518316));
#37397=CARTESIAN_POINT('Ctrl Pts',(4.21806375686963,-5.29468723858324,116.411198606602));
#37398=CARTESIAN_POINT('Ctrl Pts',(4.35805433583493,-5.17683797369691,116.419833694888));
#37399=CARTESIAN_POINT('Ctrl Pts',(4.49825282890344,-5.05881367900213,116.428481608014));
#37400=CARTESIAN_POINT('Ctrl Pts',(4.63353622735864,-4.93519004623905,116.437129521139));
#37401=CARTESIAN_POINT('Ctrl Pts',(4.76347860229511,-4.80640828534953,116.445777434264));
#37402=CARTESIAN_POINT('Ctrl Pts',(4.77805615862535,-4.79196093224712,116.446747598468));
#37403=CARTESIAN_POINT('Ctrl Pts',(4.79256653711481,-4.77744869677917,116.447717762672));
#37404=CARTESIAN_POINT('Ctrl Pts',(4.80700916793276,-4.76287222791148,116.448687926875));
#37405=CARTESIAN_POINT('Ctrl Pts',(4.92944824517308,-4.63929852308725,116.456912606394));
#37406=CARTESIAN_POINT('Ctrl Pts',(5.04728055501749,-4.51083762810376,116.465137285913));
#37407=CARTESIAN_POINT('Ctrl Pts',(5.16009405546968,-4.3778668708295,116.473361965432));
#37408=CARTESIAN_POINT('Ctrl Pts',(5.27278897617001,-4.24503588086447,116.481577999882));
#37409=CARTESIAN_POINT('Ctrl Pts',(5.38047536257406,-4.1077047394313,116.489794034332));
#37410=CARTESIAN_POINT('Ctrl Pts',(5.48277734926742,-3.96628813103135,116.498010068782));
#37411=CARTESIAN_POINT('Ctrl Pts',(5.58499229626716,-3.82499184148997,116.506219112937));
#37412=CARTESIAN_POINT('Ctrl Pts',(5.68183175847997,-3.67961729653564,116.514428157092));
#37413=CARTESIAN_POINT('Ctrl Pts',(5.77295951792179,-3.5306128935974,116.522637201246));
#37414=CARTESIAN_POINT('Ctrl Pts',(5.8640279927246,-3.38170542788546,116.530840904874));
#37415=CARTESIAN_POINT('Ctrl Pts',(5.94939198004753,-3.22917311268944,116.539044608502));
#37416=CARTESIAN_POINT('Ctrl Pts',(6.02875800466143,-3.07349408999444,116.54724831213));
#37417=CARTESIAN_POINT('Ctrl Pts',(6.10808828585596,-2.9178851791719,116.555448321124));
#37418=CARTESIAN_POINT('Ctrl Pts',(6.18142582352859,-2.75913270287075,116.563648330118));
#37419=CARTESIAN_POINT('Ctrl Pts',(6.24852257478594,-2.59774029348403,116.571848339112));
#37420=CARTESIAN_POINT('Ctrl Pts',(6.3156139608455,-2.43636078937488,116.580047692416));
#37421=CARTESIAN_POINT('Ctrl Pts',(6.37646540892027,-2.27234209999388,116.58824704572));
#37422=CARTESIAN_POINT('Ctrl Pts',(6.43087646788075,-2.10620911945077,116.596446399024));
#37423=CARTESIAN_POINT('Ctrl Pts',(6.48528717209718,-1.9400772220457,116.604645698871));
#37424=CARTESIAN_POINT('Ctrl Pts',(6.53325745821677,-1.77183140130505,116.612844998717));
#37425=CARTESIAN_POINT('Ctrl Pts',(6.57463638418398,-1.60201292621635,116.621044298564));
#37426=CARTESIAN_POINT('Ctrl Pts',(6.61602254691606,-1.432164751556,116.629245032387));
#37427=CARTESIAN_POINT('Ctrl Pts',(6.65081496793062,-1.26074372290376,116.63744576621));
#37428=CARTESIAN_POINT('Ctrl Pts',(6.67891356828393,-1.08830259918501,116.645646500033));
#37429=CARTESIAN_POINT('Ctrl Pts',(6.70702218022163,-0.915800034368081,
116.653850155793));
#37430=CARTESIAN_POINT('Ctrl Pts',(6.7284321627926,-0.742277004077402,116.662053811553));
#37431=CARTESIAN_POINT('Ctrl Pts',(6.74309516001384,-0.568292761697633,
116.670257467313));
#37432=CARTESIAN_POINT('Ctrl Pts',(6.757774954641,-0.394109209183751,116.678470520888));
#37433=CARTESIAN_POINT('Ctrl Pts',(6.76569229223513,-0.219463746644988,
116.686683574463));
#37434=CARTESIAN_POINT('Ctrl Pts',(6.76685091939767,-0.0449180881930758,
116.694896628038));
#37435=CARTESIAN_POINT('Ctrl Pts',(6.76801023214589,0.129730852841009,116.703114541461));
#37436=CARTESIAN_POINT('Ctrl Pts',(6.76240287389372,0.30427951432804,116.711332454884));
#37437=CARTESIAN_POINT('Ctrl Pts',(6.75008462315949,0.478170032714103,116.719550368307));
#37438=CARTESIAN_POINT('Ctrl Pts',(6.73774716010927,0.652331761652603,116.727781098903));
#37439=CARTESIAN_POINT('Ctrl Pts',(6.71867792672728,0.825832939991116,116.736011829499));
#37440=CARTESIAN_POINT('Ctrl Pts',(6.69298430393332,0.99812329263584,116.744242560095));
#37441=CARTESIAN_POINT('Ctrl Pts',(6.66938778429552,1.15635137600839,116.751801501771));
#37442=CARTESIAN_POINT('Ctrl Pts',(6.6402047450701,1.31355813791996,116.759360443447));
#37443=CARTESIAN_POINT('Ctrl Pts',(6.60555540683037,1.46932867912326,116.766919385123));
#37444=CARTESIAN_POINT('Ctrl Pts',(6.56817534673759,1.63737553042465,116.77507404863));
#37445=CARTESIAN_POINT('Ctrl Pts',(6.52431713584427,1.80427031315255,116.783228712137));
#37446=CARTESIAN_POINT('Ctrl Pts',(6.47406192174189,1.96946978485372,116.791383375644));
#37447=CARTESIAN_POINT('Ctrl Pts',(6.42386897374889,2.13446457474109,116.799527935539));
#37448=CARTESIAN_POINT('Ctrl Pts',(6.36729490548146,2.29776788881894,116.807672495434));
#37449=CARTESIAN_POINT('Ctrl Pts',(6.30447207342164,2.45884543545273,116.815817055329));
#37450=CARTESIAN_POINT('Ctrl Pts',(6.24171385401069,2.61975731545512,116.823953238627));
#37451=CARTESIAN_POINT('Ctrl Pts',(6.17271979817483,2.77844764744957,116.832089421924));
#37452=CARTESIAN_POINT('Ctrl Pts',(6.09767238299263,2.93439610647386,116.840225605222));
#37453=CARTESIAN_POINT('Ctrl Pts',(6.0187573433945,3.09838148544117,116.848781092783));
#37454=CARTESIAN_POINT('Ctrl Pts',(5.9331485951568,3.25933451142286,116.857336580344));
#37455=CARTESIAN_POINT('Ctrl Pts',(5.84111685766212,3.41667131213048,116.865892067906));
#37456=CARTESIAN_POINT('Ctrl Pts',(5.7537240793098,3.56607738144107,116.874016306875));
#37457=CARTESIAN_POINT('Ctrl Pts',(5.66054009726045,3.71222244486196,116.882140545844));
#37458=CARTESIAN_POINT('Ctrl Pts',(5.56184473932597,3.85462995573273,116.890264784813));
#37459=CARTESIAN_POINT('Ctrl Pts',(5.46318110551415,3.99699169187367,116.898386412369));
#37460=CARTESIAN_POINT('Ctrl Pts',(5.35900983063957,4.13561796683221,116.906508039925));
#37461=CARTESIAN_POINT('Ctrl Pts',(5.24965458963027,4.27006038476903,116.914629667481));
#37462=CARTESIAN_POINT('Ctrl Pts',(5.14031367721987,4.40448518698425,116.922750230876));
#37463=CARTESIAN_POINT('Ctrl Pts',(5.02579038232472,4.53472694036051,116.930870794271));
#37464=CARTESIAN_POINT('Ctrl Pts',(4.90644923350734,4.66036961184575,116.938991357666));
#37465=CARTESIAN_POINT('Ctrl Pts',(4.78710099840464,4.78601974379058,116.947112403248));
#37466=CARTESIAN_POINT('Ctrl Pts',(4.66293459268715,4.90706998587007,116.955233448829));
#37467=CARTESIAN_POINT('Ctrl Pts',(4.53435199154811,5.02314055315434,116.96335449441));
#37468=CARTESIAN_POINT('Ctrl Pts',(4.40569060790862,5.13928223682169,116.971480515752));
#37469=CARTESIAN_POINT('Ctrl Pts',(4.27260789653572,5.25043790678331,116.979606537094));
#37470=CARTESIAN_POINT('Ctrl Pts',(4.13553997474194,5.35626718128506,116.987732558437));
#37471=CARTESIAN_POINT('Ctrl Pts',(3.99842323160449,5.46213415043714,116.995861474134));
#37472=CARTESIAN_POINT('Ctrl Pts',(3.85731874578134,5.56267072954954,117.003990389832));
#37473=CARTESIAN_POINT('Ctrl Pts',(3.71269209764839,5.65757955207518,117.012119305529));
#37474=CARTESIAN_POINT('Ctrl Pts',(3.56792806304677,5.75257853217648,117.020255943199));
#37475=CARTESIAN_POINT('Ctrl Pts',(3.41963549707585,5.84193889063614,117.02839258087));
#37476=CARTESIAN_POINT('Ctrl Pts',(3.26830560347552,5.92540863420326,117.03652921854));
#37477=CARTESIAN_POINT('Ctrl Pts',(3.2123357350403,5.95628019866832,117.039538581258));
#37478=CARTESIAN_POINT('Ctrl Pts',(3.15595060002474,5.98634644394689,117.042547943976));
#37479=CARTESIAN_POINT('Ctrl Pts',(3.09917575053267,6.01559628526635,117.045557306694));
#37480=CARTESIAN_POINT('Ctrl Pts',(3.09917575053242,6.01559628526648,115.045751582742));
#37481=CARTESIAN_POINT('Ctrl Pts',(2.93382384459253,6.10078395293765,115.054501030655));
#37482=CARTESIAN_POINT('Ctrl Pts',(2.76495772122977,6.17915010267052,115.063250478567));
#37483=CARTESIAN_POINT('Ctrl Pts',(2.5931509331671,6.25042856433178,115.07199992648));
#37484=CARTESIAN_POINT('Ctrl Pts',(2.4213455324562,6.3217064504145,115.08074930374));
#37485=CARTESIAN_POINT('Ctrl Pts',(2.24659977927598,6.38589665313455,115.089498681));
#37486=CARTESIAN_POINT('Ctrl Pts',(2.0695071868993,6.44278115439071,115.09824805826));
#37487=CARTESIAN_POINT('Ctrl Pts',(1.89241596572877,6.49966521519719,115.106997367774));
#37488=CARTESIAN_POINT('Ctrl Pts',(1.71297821457218,6.54924360009541,115.115746677289));
#37489=CARTESIAN_POINT('Ctrl Pts',(1.53180337335869,6.5913479217355,115.124495986804));
#37490=CARTESIAN_POINT('Ctrl Pts',(1.35062987477819,6.63345193135297,115.13324523148));
#37491=CARTESIAN_POINT('Ctrl Pts',(1.16771959102999,6.66808192368229,115.141994476156));
#37492=CARTESIAN_POINT('Ctrl Pts',(0.983693746907436,6.6951202836316,115.150743720832));
#37493=CARTESIAN_POINT('Ctrl Pts',(0.799669205420572,6.72215845218858,115.159492903576));
#37494=CARTESIAN_POINT('Ctrl Pts',(0.614529402874287,6.74160505424571,115.16824208632));
#37495=CARTESIAN_POINT('Ctrl Pts',(0.428903127364168,6.75339404354116,115.176991269065));
#37496=CARTESIAN_POINT('Ctrl Pts',(0.243278104164932,6.76518295330326,115.185740392783));
#37497=CARTESIAN_POINT('Ctrl Pts',(0.0571669005403033,6.76931433552274,
115.194489516502));
#37498=CARTESIAN_POINT('Ctrl Pts',(-0.128798404776197,6.76577415902475,
115.20323864022));
#37499=CARTESIAN_POINT('Ctrl Pts',(-0.314762517257765,6.76223400523448,
115.21198770782));
#37500=CARTESIAN_POINT('Ctrl Pts',(-0.500580446818164,6.75102239665099,
115.220736775419));
#37501=CARTESIAN_POINT('Ctrl Pts',(-0.685621118841252,6.73217741012511,
115.229485843018));
#37502=CARTESIAN_POINT('Ctrl Pts',(-0.870660665413233,6.71333253821788,
115.238234857404));
#37503=CARTESIAN_POINT('Ctrl Pts',(-1.05492267885371,6.6868544103063,115.246983871789));
#37504=CARTESIAN_POINT('Ctrl Pts',(-1.23778137635147,6.65283295028197,115.255732886175));
#37505=CARTESIAN_POINT('Ctrl Pts',(-1.42999922978729,6.6170701886189,115.264929696543));
#37506=CARTESIAN_POINT('Ctrl Pts',(-1.62066601233565,6.57297172934445,115.27412650691));
#37507=CARTESIAN_POINT('Ctrl Pts',(-1.80906628500243,6.52070304311334,115.283323317277));
#37508=CARTESIAN_POINT('Ctrl Pts',(-1.98831342545388,6.47097374915073,115.292073315015));
#37509=CARTESIAN_POINT('Ctrl Pts',(-2.16550875896566,6.41384933989574,115.300823312753));
#37510=CARTESIAN_POINT('Ctrl Pts',(-2.34005036713878,6.34952386240525,115.309573310491));
#37511=CARTESIAN_POINT('Ctrl Pts',(-2.51458843546958,6.28519968948648,115.318323130772));
#37512=CARTESIAN_POINT('Ctrl Pts',(-2.68647261717926,6.21367483971155,115.327072951052));
#37513=CARTESIAN_POINT('Ctrl Pts',(-2.85511905908604,6.13519226743903,115.335822771333));
#37514=CARTESIAN_POINT('Ctrl Pts',(-3.02376230488754,6.05671118253002,115.344572425792));
#37515=CARTESIAN_POINT('Ctrl Pts',(-3.18916767379771,5.97127275992704,115.35332208025));
#37516=CARTESIAN_POINT('Ctrl Pts',(-3.35077334102651,5.87916720438074,115.362071734709));
#37517=CARTESIAN_POINT('Ctrl Pts',(-3.51237616037244,5.78706327195719,115.370821234977));
#37518=CARTESIAN_POINT('Ctrl Pts',(-3.67017916302186,5.68829258362372,115.379570735246));
#37519=CARTESIAN_POINT('Ctrl Pts',(-3.8236463656636,5.58319061741112,115.388320235514));
#37520=CARTESIAN_POINT('Ctrl Pts',(-3.97711106778694,5.47809036367777,115.397069593223));
#37521=CARTESIAN_POINT('Ctrl Pts',(-4.12623987481822,5.36665920043306,115.405818950931));
#37522=CARTESIAN_POINT('Ctrl Pts',(-4.27052628213823,5.24927559512421,115.41456830864));
#37523=CARTESIAN_POINT('Ctrl Pts',(-4.41481053024882,5.13189374643119,115.423317535416));
#37524=CARTESIAN_POINT('Ctrl Pts',(-4.55425230136443,5.00855981477433,115.432066762193));
#37525=CARTESIAN_POINT('Ctrl Pts',(-4.6883780063047,4.87969268192152,115.440815988969));
#37526=CARTESIAN_POINT('Ctrl Pts',(-4.82250188228816,4.75082730631889,115.44956509644));
#37527=CARTESIAN_POINT('Ctrl Pts',(-4.95130963052887,4.6164290790361,115.458314203911));
#37528=CARTESIAN_POINT('Ctrl Pts',(-5.07436379033289,4.47695444731778,115.467063311382));
#37529=CARTESIAN_POINT('Ctrl Pts',(-5.19741643562687,4.33748153220726,115.475812311171));
#37530=CARTESIAN_POINT('Ctrl Pts',(-5.31471544462618,4.19293255254782,115.484561310961));
#37531=CARTESIAN_POINT('Ctrl Pts',(-5.42586245275441,4.04379841779854,115.493310310751));
#37532=CARTESIAN_POINT('Ctrl Pts',(-5.53702160018975,3.89464799484596,115.502060266093));
#37533=CARTESIAN_POINT('Ctrl Pts',(-5.64202723081082,3.74091164444105,115.510810221435));
#37534=CARTESIAN_POINT('Ctrl Pts',(-5.74052265232807,3.5831115916349,115.519560176777));
#37535=CARTESIAN_POINT('Ctrl Pts',(-5.83901427066765,3.42531763192044,115.52830979426));
#37536=CARTESIAN_POINT('Ctrl Pts',(-5.93099603115594,3.26346052695878,115.537059411742));
#37537=CARTESIAN_POINT('Ctrl Pts',(-6.01615550622615,3.09809004467345,115.545809029225));
#37538=CARTESIAN_POINT('Ctrl Pts',(-6.10131214578665,2.93272506864107,115.554558355376));
#37539=CARTESIAN_POINT('Ctrl Pts',(-6.17964682328618,2.76384720417184,115.563307681527));
#37540=CARTESIAN_POINT('Ctrl Pts',(-6.25089348288439,2.59203002791894,115.572057007678));
#37541=CARTESIAN_POINT('Ctrl Pts',(-6.32213814889229,2.42021765937296,115.58080608901));
#37542=CARTESIAN_POINT('Ctrl Pts',(-6.38629508412504,2.24546640832151,115.589555170341));
#37543=CARTESIAN_POINT('Ctrl Pts',(-6.44314639819748,2.06836976660238,115.598304251673));
#37544=CARTESIAN_POINT('Ctrl Pts',(-6.50000285283646,1.89125711158464,115.607054124107));
#37545=CARTESIAN_POINT('Ctrl Pts',(-6.54955227673203,1.71179891440435,115.615803996541));
#37546=CARTESIAN_POINT('Ctrl Pts',(-6.59162635926345,1.53060476278602,115.624553868976));
#37547=CARTESIAN_POINT('Ctrl Pts',(-6.63369752055162,1.34942319164865,115.633303133898));
#37548=CARTESIAN_POINT('Ctrl Pts',(-6.66829431424225,1.16650618642871,115.642052398821));
#37549=CARTESIAN_POINT('Ctrl Pts',(-6.69529923745393,0.982474997620204,
115.650801663743));
#37550=CARTESIAN_POINT('Ctrl Pts',(-6.72230554731424,0.798434359179406,
115.659551377923));
#37551=CARTESIAN_POINT('Ctrl Pts',(-6.74171916496688,0.613279706242019,
115.668301092103));
#37552=CARTESIAN_POINT('Ctrl Pts',(-6.75347414817264,0.427639953657075,
115.677050806282));
#37553=CARTESIAN_POINT('Ctrl Pts',(-6.76248837758729,0.285283364201547,
115.683760465458));
#37554=CARTESIAN_POINT('Ctrl Pts',(-6.76699999999985,0.142641701109372,
115.690470124634));
#37555=CARTESIAN_POINT('Ctrl Pts',(-6.767,7.10081502014786E-12,115.69717978381));
#37556=CARTESIAN_POINT('',(-6.76699755877019,-0.0057480082024489,115.302820216158));
#37557=CARTESIAN_POINT('Ctrl Pts',(3.09917575053242,6.01559628526648,114.651222310038));
#37558=CARTESIAN_POINT('Ctrl Pts',(2.94386794804138,6.09560933011252,114.659440724924));
#37559=CARTESIAN_POINT('Ctrl Pts',(2.78558299399996,6.16954045709756,114.667659139811));
#37560=CARTESIAN_POINT('Ctrl Pts',(2.62484349248842,6.23718571472272,114.675877554697));
#37561=CARTESIAN_POINT('Ctrl Pts',(2.45841482043055,6.30722519034446,114.684386849943));
#37562=CARTESIAN_POINT('Ctrl Pts',(2.2893550773906,6.37052554480549,114.692896145188));
#37563=CARTESIAN_POINT('Ctrl Pts',(2.11826038758146,6.42691698486944,114.701405440433));
#37564=CARTESIAN_POINT('Ctrl Pts',(1.94716569777231,6.48330842493339,114.709914735679));
#37565=CARTESIAN_POINT('Ctrl Pts',(1.77403648248922,6.53279089961688,114.718424030924));
#37566=CARTESIAN_POINT('Ctrl Pts',(1.5994789746382,6.5752533038424,114.72693332617));
#37567=CARTESIAN_POINT('Ctrl Pts',(1.43217998526167,6.61595001978939,114.735088784577));
#37568=CARTESIAN_POINT('Ctrl Pts',(1.26305388888637,6.65032388175451,114.743244242983));
#37569=CARTESIAN_POINT('Ctrl Pts',(1.09262403249341,6.67820797247419,114.75139970139));
#37570=CARTESIAN_POINT('Ctrl Pts',(0.922401611638456,6.70605812459014,114.759545233532));
#37571=CARTESIAN_POINT('Ctrl Pts',(0.750878946201532,6.72743417022452,114.767690765674));
#37572=CARTESIAN_POINT('Ctrl Pts',(0.578593969420025,6.74221907227515,114.775836297816));
#37573=CARTESIAN_POINT('Ctrl Pts',(0.406482458027426,6.75698908812483,114.783973628616));
#37574=CARTESIAN_POINT('Ctrl Pts',(0.233610524755594,6.76518114107602,114.792110959417));
#37575=CARTESIAN_POINT('Ctrl Pts',(0.0605257131714355,6.76672931615009,
114.800248290217));
#37576=CARTESIAN_POINT('Ctrl Pts',(-0.112421202018021,6.76827625779554,
114.808379138019));
#37577=CARTESIAN_POINT('Ctrl Pts',(-0.285580294038634,6.76318985766359,
114.816509985821));
#37578=CARTESIAN_POINT('Ctrl Pts',(-0.458399485989158,6.75145605860283,
114.824640833623));
#37579=CARTESIAN_POINT('Ctrl Pts',(-0.631117296826381,6.73972914295357,
114.832766911617));
#37580=CARTESIAN_POINT('Ctrl Pts',(-0.803495240938185,6.72136261899128,
114.840892989611));
#37581=CARTESIAN_POINT('Ctrl Pts',(-0.974981834225679,6.69639450920642,
114.849019067605));
#37582=CARTESIAN_POINT('Ctrl Pts',(-1.14707648765193,6.67133786706456,114.857173959187));
#37583=CARTESIAN_POINT('Ctrl Pts',(-1.31827308564726,6.63963273996283,114.865328850769));
#37584=CARTESIAN_POINT('Ctrl Pts',(-1.48801942654411,6.60137009917088,114.873483742351));
#37585=CARTESIAN_POINT('Ctrl Pts',(-1.65710381606168,6.56325666929985,114.881606832708));
#37586=CARTESIAN_POINT('Ctrl Pts',(-1.82474888361939,6.51863687565459,114.889729923064));
#37587=CARTESIAN_POINT('Ctrl Pts',(-1.99041941501957,6.46765178038468,114.89785301342));
#37588=CARTESIAN_POINT('Ctrl Pts',(-2.15610295562624,6.41666268153232,114.905976741639));
#37589=CARTESIAN_POINT('Ctrl Pts',(-2.31981130157248,6.35930739300896,114.914100469857));
#37590=CARTESIAN_POINT('Ctrl Pts',(-2.48102495991978,6.2957766914222,114.922224198075));
#37591=CARTESIAN_POINT('Ctrl Pts',(-2.64228194820668,6.23222891447414,114.930350109736));
#37592=CARTESIAN_POINT('Ctrl Pts',(-2.80104257358362,6.16250255358571,114.938476021396));
#37593=CARTESIAN_POINT('Ctrl Pts',(-2.95680790489217,6.086836289368,114.946601933056));
#37594=CARTESIAN_POINT('Ctrl Pts',(-3.11356937168604,6.01068613152521,114.954779810766));
#37595=CARTESIAN_POINT('Ctrl Pts',(-3.26729676315548,5.92851999817133,114.962957688476));
#37596=CARTESIAN_POINT('Ctrl Pts',(-3.41750794396777,5.84062740233592,114.971135566187));
#37597=CARTESIAN_POINT('Ctrl Pts',(-3.56700219939296,5.75315429879762,114.97927441266));
#37598=CARTESIAN_POINT('Ctrl Pts',(-3.71301345948487,5.66000952394965,114.987413259133));
#37599=CARTESIAN_POINT('Ctrl Pts',(-3.85509710640812,5.56152095205653,114.995552105607));
#37600=CARTESIAN_POINT('Ctrl Pts',(-3.99820283314257,5.46232390186104,115.003749498935));
#37601=CARTESIAN_POINT('Ctrl Pts',(-4.13732392511519,5.35770611051118,115.011946892264));
#37602=CARTESIAN_POINT('Ctrl Pts',(-4.27204172903311,5.2480423459991,115.020144285592));
#37603=CARTESIAN_POINT('Ctrl Pts',(-4.40675953295094,5.13837858148711,115.02834167892));
#37604=CARTESIAN_POINT('Ctrl Pts',(-4.53707380978711,5.02366913563118,115.036539072249));
#37605=CARTESIAN_POINT('Ctrl Pts',(-4.66260549184018,4.90432452305736,115.044736465577));
#37606=CARTESIAN_POINT('Ctrl Pts',(-4.78687260473668,4.78618215292621,115.052851280782));
#37607=CARTESIAN_POINT('Ctrl Pts',(-4.9068439986788,4.66312580612143,115.060966095986));
#37608=CARTESIAN_POINT('Ctrl Pts',(-5.02210030006701,4.53550411487707,115.069080911191));
#37609=CARTESIAN_POINT('Ctrl Pts',(-5.13722482978538,4.40802833256057,115.077186448788));
#37610=CARTESIAN_POINT('Ctrl Pts',(-5.24764475170721,4.27599786668457,115.085291986385));
#37611=CARTESIAN_POINT('Ctrl Pts',(-5.35297499051895,4.13980044819538,115.093397523982));
#37612=CARTESIAN_POINT('Ctrl Pts',(-5.45820745226497,4.00372946048322,115.101495537285));
#37613=CARTESIAN_POINT('Ctrl Pts',(-5.55835941220256,3.86349951133587,115.109593550588));
#37614=CARTESIAN_POINT('Ctrl Pts',(-5.65308384297548,3.71953385040243,115.117691563891));
#37615=CARTESIAN_POINT('Ctrl Pts',(-5.74773479793613,3.57567986070092,115.12578329573));
#37616=CARTESIAN_POINT('Ctrl Pts',(-5.83696640731683,3.42809623867887,115.133875027569));
#37617=CARTESIAN_POINT('Ctrl Pts',(-5.92047311482842,3.27723772354003,115.141966759408));
#37618=CARTESIAN_POINT('Ctrl Pts',(-6.0039444365198,3.12644313443126,115.15005506239));
#37619=CARTESIAN_POINT('Ctrl Pts',(-6.08169550585098,2.97237673674744,115.158143365372));
#37620=CARTESIAN_POINT('Ctrl Pts',(-6.15346506327538,2.81552068276001,115.166231668354));
#37621=CARTESIAN_POINT('Ctrl Pts',(-6.22521816066974,2.65870060301363,115.174318116319));
#37622=CARTESIAN_POINT('Ctrl Pts',(-6.29099232365082,2.49909247655245,115.182404564285));
#37623=CARTESIAN_POINT('Ctrl Pts',(-6.35057312732416,2.33720130808373,115.19049101225));
#37624=CARTESIAN_POINT('Ctrl Pts',(-6.41015184862715,2.17531579776913,115.198577177591));
#37625=CARTESIAN_POINT('Ctrl Pts',(-6.46353751519334,2.01114775155845,115.206663342932));
#37626=CARTESIAN_POINT('Ctrl Pts',(-6.51056459216175,1.84522022839815,115.214749508273));
#37627=CARTESIAN_POINT('Ctrl Pts',(-6.55761635707495,1.67920559777138,115.222839918633));
#37628=CARTESIAN_POINT('Ctrl Pts',(-6.59830276205021,1.51143000064262,115.230930328992));
#37629=CARTESIAN_POINT('Ctrl Pts',(-6.63250859599296,1.34243015612713,115.239020739352));
#37630=CARTESIAN_POINT('Ctrl Pts',(-6.66672400141049,1.17338302208344,115.24711341357));
#37631=CARTESIAN_POINT('Ctrl Pts',(-6.69445516007678,1.00311132232287,115.255206087787));
#37632=CARTESIAN_POINT('Ctrl Pts',(-6.71563841851484,0.832159619164219,
115.263298762005));
#37633=CARTESIAN_POINT('Ctrl Pts',(-6.73684188433465,0.661044839756617,
115.271399156081));
#37634=CARTESIAN_POINT('Ctrl Pts',(-6.75148493977132,0.489249129225492,
115.279499550157));
#37635=CARTESIAN_POINT('Ctrl Pts',(-6.75955595540448,0.317320477996312,
115.287599944234));
#37636=CARTESIAN_POINT('Ctrl Pts',(-6.76461097912664,0.209638440197907,
115.292673368208));
#37637=CARTESIAN_POINT('Ctrl Pts',(-6.76708900053199,0.101904270120243,
115.297746792183));
#37638=CARTESIAN_POINT('Ctrl Pts',(-6.76699755877019,-0.0057480082026374,
115.302820216158));
#37639=CARTESIAN_POINT('Ctrl Pts',(-6.76699755876961,-0.00574800888219676,
115.30282021619));
#37640=CARTESIAN_POINT('Ctrl Pts',(-6.76678167727306,-0.259900288408448,
115.314797875077));
#37641=CARTESIAN_POINT('Ctrl Pts',(-6.75224451939847,-0.513469327072015,
115.326775533965));
#37642=CARTESIAN_POINT('Ctrl Pts',(-6.72360183255187,-0.765158413209378,
115.338753192852));
#37643=CARTESIAN_POINT('Ctrl Pts',(-6.70464134507653,-0.931768053951088,
115.346681996897));
#37644=CARTESIAN_POINT('Ctrl Pts',(-6.67950074655919,-1.09755475887882,
115.354610800941));
#37645=CARTESIAN_POINT('Ctrl Pts',(-6.64825307665784,-1.26214897247099,
115.362539604986));
#37646=CARTESIAN_POINT('Ctrl Pts',(-6.61583335578514,-1.43291685624495,
115.370765806004));
#37647=CARTESIAN_POINT('Ctrl Pts',(-6.57678454556754,-1.6026735155636,115.378992007023));
#37648=CARTESIAN_POINT('Ctrl Pts',(-6.53118084059293,-1.77086584118386,
115.387218208042));
#37649=CARTESIAN_POINT('Ctrl Pts',(-6.48562836176938,-1.93886923817469,
115.395435168658));
#37650=CARTESIAN_POINT('Ctrl Pts',(-6.43353574300848,-2.10531145753296,
115.403652129274));
#37651=CARTESIAN_POINT('Ctrl Pts',(-6.37502850393306,-2.26964767619141,
115.411869089889));
#37652=CARTESIAN_POINT('Ctrl Pts',(-6.31657524254206,-2.43383228132836,
115.420078469691));
#37653=CARTESIAN_POINT('Ctrl Pts',(-6.25171926630277,-2.59591441949666,
115.428287849492));
#37654=CARTESIAN_POINT('Ctrl Pts',(-6.18063641974115,-2.75536248921432,
115.436497229294));
#37655=CARTESIAN_POINT('Ctrl Pts',(-6.10960489056996,-2.914695447351,115.444700682434));
#37656=CARTESIAN_POINT('Ctrl Pts',(-6.03235559060419,-3.07139779853106,
115.452904135575));
#37657=CARTESIAN_POINT('Ctrl Pts',(-5.94911320717886,-3.22495597616,115.461107588715));
#37658=CARTESIAN_POINT('Ctrl Pts',(-5.86591422135814,-3.37843409773092,
115.469306765065));
#37659=CARTESIAN_POINT('Ctrl Pts',(-5.77672854701966,-3.52877099675739,
115.477505941416));
#37660=CARTESIAN_POINT('Ctrl Pts',(-5.68182776488053,-3.67547578555929,
115.485705117766));
#37661=CARTESIAN_POINT('Ctrl Pts',(-5.58694483975551,-3.82215296964157,
115.493902751317));
#37662=CARTESIAN_POINT('Ctrl Pts',(-5.48634913824785,-3.96519910063855,
115.502100384868));
#37663=CARTESIAN_POINT('Ctrl Pts',(-5.38035686555694,-4.10415021645825,
115.51029801842));
#37664=CARTESIAN_POINT('Ctrl Pts',(-5.27437222691092,-4.24309132438748,
115.51849506154));
#37665=CARTESIAN_POINT('Ctrl Pts',(-5.16299200800417,-4.3779377188147,115.526692104661));
#37666=CARTESIAN_POINT('Ctrl Pts',(-5.04657416216928,-4.50825667256485,
115.534889147781));
#37667=CARTESIAN_POINT('Ctrl Pts',(-4.93014354252737,-4.63858992540423,
115.543087090313));
#37668=CARTESIAN_POINT('Ctrl Pts',(-4.80867443373095,-4.76439448031514,
115.551285032844));
#37669=CARTESIAN_POINT('Ctrl Pts',(-4.68256330603861,-4.88527275440592,
115.559482975375));
#37670=CARTESIAN_POINT('Ctrl Pts',(-4.55641542038324,-5.00618626122525,
115.567683307383));
#37671=CARTESIAN_POINT('Ctrl Pts',(-4.42562307965035,-5.12217037899755,
115.575883639392));
#37672=CARTESIAN_POINT('Ctrl Pts',(-4.29061766570285,-5.23286623627612,
115.5840839714));
#37673=CARTESIAN_POINT('Ctrl Pts',(-4.15547153962493,-5.34367746855671,
115.592292850371));
#37674=CARTESIAN_POINT('Ctrl Pts',(-4.01610384518723,-5.44918920088608,
115.600501729342));
#37675=CARTESIAN_POINT('Ctrl Pts',(-3.87297773024824,-5.5490839334976,115.608710608313));
#37676=CARTESIAN_POINT('Ctrl Pts',(-3.72977478189105,-5.64903229191858,
115.616923894));
#37677=CARTESIAN_POINT('Ctrl Pts',(-3.5828096924262,-5.74335744589683,115.625137179687));
#37678=CARTESIAN_POINT('Ctrl Pts',(-3.4325722208913,-5.83178677151055,115.633350465375));
#37679=CARTESIAN_POINT('Ctrl Pts',(-3.2821149704518,-5.92034545832902,115.641575766087));
#37680=CARTESIAN_POINT('Ctrl Pts',(-3.12837608715594,-6.0029909107217,115.649801066799));
#37681=CARTESIAN_POINT('Ctrl Pts',(-2.97186856562106,-6.0794972019628,115.658026367511));
#37682=CARTESIAN_POINT('Ctrl Pts',(-2.83032639155331,-6.14868791360352,
115.665465159805));
#37683=CARTESIAN_POINT('Ctrl Pts',(-2.68652018770616,-6.21285794133146,
115.672903952099));
#37684=CARTESIAN_POINT('Ctrl Pts',(-2.5408407664906,-6.27187509436687,115.680342744393));
#37685=CARTESIAN_POINT('Ctrl Pts',(-2.38118317374816,-6.33655503684279,
115.688495300606));
#37686=CARTESIAN_POINT('Ctrl Pts',(-2.21880449344297,-6.39523577316451,
115.69664785682));
#37687=CARTESIAN_POINT('Ctrl Pts',(-2.05419958647906,-6.44767811377935,
115.704800413033));
#37688=CARTESIAN_POINT('Ctrl Pts',(-1.88978537826828,-6.50005969867828,
115.712943524313));
#37689=CARTESIAN_POINT('Ctrl Pts',(-1.72315042216969,-6.5462171647288,115.721086635594));
#37690=CARTESIAN_POINT('Ctrl Pts',(-1.55481101124606,-6.58595867883393,
115.729229746874));
#37691=CARTESIAN_POINT('Ctrl Pts',(-1.38663123432373,-6.62566250659528,
115.737365136151));
#37692=CARTESIAN_POINT('Ctrl Pts',(-1.21675057378088,-6.6589624117825,115.745500525429));
#37693=CARTESIAN_POINT('Ctrl Pts',(-1.04570200091712,-6.68571584239698,
115.753635914706));
#37694=CARTESIAN_POINT('Ctrl Pts',(-0.874779689684171,-6.712449524634,115.761765298744));
#37695=CARTESIAN_POINT('Ctrl Pts',(-0.702691542388614,-6.73264629812668,
115.769894682783));
#37696=CARTESIAN_POINT('Ctrl Pts',(-0.529982283951907,-6.74621432943671,
115.778024066822));
#37697=CARTESIAN_POINT('Ctrl Pts',(-0.357364235797033,-6.75977519527123,
115.786149157614));
#37698=CARTESIAN_POINT('Ctrl Pts',(-0.184126093387903,-6.76671426221848,
115.794274248406));
#37699=CARTESIAN_POINT('Ctrl Pts',(-0.0108192902924455,-6.76699135088538,
115.802399339198));
#37700=CARTESIAN_POINT('Ctrl Pts',(0.163149062441214,-6.76726949725979,
115.810555445223));
#37701=CARTESIAN_POINT('Ctrl Pts',(0.337186232143776,-6.76083465475762,
115.818711551248));
#37702=CARTESIAN_POINT('Ctrl Pts',(0.510732301391071,-6.74769897937925,
115.826867657273));
#37703=CARTESIAN_POINT('Ctrl Pts',(0.683579879095664,-6.73461617271868,
115.834990936447));
#37704=CARTESIAN_POINT('Ctrl Pts',(0.855939936531955,-6.71488642160143,
115.84311421562));
#37705=CARTESIAN_POINT('Ctrl Pts',(1.02726267157644,-6.68857386918808,115.851237494794));
#37706=CARTESIAN_POINT('Ctrl Pts',(1.19860821969072,-6.66225781303605,115.85936185565));
#37707=CARTESIAN_POINT('Ctrl Pts',(1.36891580866499,-6.62935726519153,115.867486216507));
#37708=CARTESIAN_POINT('Ctrl Pts',(1.53764424661283,-6.58998779747417,115.875610577364));
#37709=CARTESIAN_POINT('Ctrl Pts',(1.70642725363144,-6.55060559713571,115.883737565749));
#37710=CARTESIAN_POINT('Ctrl Pts',(1.8736297365495,-6.50475039390041,115.891864554135));
#37711=CARTESIAN_POINT('Ctrl Pts',(2.03872415980008,-6.45258806993345,115.89999154252));
#37712=CARTESIAN_POINT('Ctrl Pts',(2.20488589970089,-6.40008852248075,115.90817107096));
#37713=CARTESIAN_POINT('Ctrl Pts',(2.36891187034279,-6.34120013515826,115.9163505994));
#37714=CARTESIAN_POINT('Ctrl Pts',(2.53028402869268,-6.27614146862089,115.92453012784));
#37715=CARTESIAN_POINT('Ctrl Pts',(2.6908962335249,-6.21138918431819,115.932671136244));
#37716=CARTESIAN_POINT('Ctrl Pts',(2.84887926055234,-6.14052481960731,115.940812144648));
#37717=CARTESIAN_POINT('Ctrl Pts',(3.00374683638185,-6.06381018361608,115.948953153051));
#37718=CARTESIAN_POINT('Ctrl Pts',(3.15971357051451,-5.98655107258757,115.95715194151));
#37719=CARTESIAN_POINT('Ctrl Pts',(3.31252013607327,-5.90335852202639,115.965350729968));
#37720=CARTESIAN_POINT('Ctrl Pts',(3.46169961181315,-5.81454424676369,115.973549518426));
#37721=CARTESIAN_POINT('Ctrl Pts',(3.61087908755314,-5.72572997150092,115.981748306884));
#37722=CARTESIAN_POINT('Ctrl Pts',(3.75643119719572,-5.63129422801327,115.989947095343));
#37723=CARTESIAN_POINT('Ctrl Pts',(3.89792326152257,-5.53158957690113,115.998145883801));
#37724=CARTESIAN_POINT('Ctrl Pts',(4.0400066028375,-5.43146827298173,116.006378933933));
#37725=CARTESIAN_POINT('Ctrl Pts',(4.17843763551627,-5.32572280050154,116.014611984065));
#37726=CARTESIAN_POINT('Ctrl Pts',(4.31274193540481,-5.21464725543356,116.022845034197));
#37727=CARTESIAN_POINT('Ctrl Pts',(4.44688629951697,-5.10370398426562,116.031068280032));
#37728=CARTESIAN_POINT('Ctrl Pts',(4.57691344312677,-4.98744350558531,116.039291525867));
#37729=CARTESIAN_POINT('Ctrl Pts',(4.70237745363485,-4.86620337465941,116.047514771701));
#37730=CARTESIAN_POINT('Ctrl Pts',(4.82771716768466,-4.74508335561908,116.055729870815));
#37731=CARTESIAN_POINT('Ctrl Pts',(4.94850249580004,-4.61899375627437,116.063944969928));
#37732=CARTESIAN_POINT('Ctrl Pts',(5.0643201312491,-4.48831266827804,116.072160069042));
#37733=CARTESIAN_POINT('Ctrl Pts',(5.18004619962243,-4.35773489861517,116.080368673181));
#37734=CARTESIAN_POINT('Ctrl Pts',(5.29081216168008,-4.22257313757797,116.08857727732));
#37735=CARTESIAN_POINT('Ctrl Pts',(5.39624110344065,-4.0832427007879,116.096785881459));
#37736=CARTESIAN_POINT('Ctrl Pts',(5.50160778030266,-3.9439945506581,116.104989637708));
#37737=CARTESIAN_POINT('Ctrl Pts',(5.60164350047405,-3.80058291420172,116.113193393957));
#37738=CARTESIAN_POINT('Ctrl Pts',(5.69601118519311,-3.65345666159529,116.121397150206));
#37739=CARTESIAN_POINT('Ctrl Pts',(5.79035094889282,-3.50637393993865,116.12959847917));
#37740=CARTESIAN_POINT('Ctrl Pts',(5.87902582133705,-3.35557909044896,116.137799808134));
#37741=CARTESIAN_POINT('Ctrl Pts',(5.96174154195762,-3.20155068473025,116.146001137098));
#37742=CARTESIAN_POINT('Ctrl Pts',(6.0444458552907,-3.04754352099909,116.154201335021));
#37743=CARTESIAN_POINT('Ctrl Pts',(6.12119248343146,-2.8903040043522,116.162401532944));
#37744=CARTESIAN_POINT('Ctrl Pts',(6.19173270167273,-2.73033608756075,116.170601730867));
#37745=CARTESIAN_POINT('Ctrl Pts',(6.26227597506725,-2.57036124243092,116.178802283946));
#37746=CARTESIAN_POINT('Ctrl Pts',(6.32661215841506,-2.40765808955534,116.187002837026));
#37747=CARTESIAN_POINT('Ctrl Pts',(6.38454031569593,-2.24275142564961,116.195203390106));
#37748=CARTESIAN_POINT('Ctrl Pts',(6.44248147960843,-2.07780773518664,116.203405784459));
#37749=CARTESIAN_POINT('Ctrl Pts',(6.49401163305737,-1.91065988624609,116.211608178812));
#37750=CARTESIAN_POINT('Ctrl Pts',(6.53897941783983,-1.74184878019509,116.219810573166));
#37751=CARTESIAN_POINT('Ctrl Pts',(6.58398925540597,-1.57287980608452,116.228020638199));
#37752=CARTESIAN_POINT('Ctrl Pts',(6.62242437081179,-1.4022448138883,116.236230703233));
#37753=CARTESIAN_POINT('Ctrl Pts',(6.65418414511383,-1.23049679516678,116.244440768267));
#37754=CARTESIAN_POINT('Ctrl Pts',(6.68595911908042,-1.05866658089045,116.252654762492));
#37755=CARTESIAN_POINT('Ctrl Pts',(6.71105233081618,-0.885722632397782,
116.260868756718));
#37756=CARTESIAN_POINT('Ctrl Pts',(6.72941498191682,-0.712223982433492,
116.269082750943));
#37757=CARTESIAN_POINT('Ctrl Pts',(6.74780266742679,-0.538488796023771,
116.277307943578));
#37758=CARTESIAN_POINT('Ctrl Pts',(6.75944143007326,-0.364197754368599,
116.285533136213));
#37759=CARTESIAN_POINT('Ctrl Pts',(6.7643345877112,-0.189912046732136,116.293758328849));
#37760=CARTESIAN_POINT('Ctrl Pts',(6.76873499389469,-0.0331772831448199,
116.301155226969));
#37761=CARTESIAN_POINT('Ctrl Pts',(6.76768068728745,0.123552989384368,116.308552125088));
#37762=CARTESIAN_POINT('Ctrl Pts',(6.76120990434969,0.279874309867328,116.315949023208));
#37763=CARTESIAN_POINT('Ctrl Pts',(6.75364644037559,0.462592643526132,116.324594989699));
#37764=CARTESIAN_POINT('Ctrl Pts',(6.73866511629857,0.645166944255017,116.33324095619));
#37765=CARTESIAN_POINT('Ctrl Pts',(6.71627762428073,0.826984808558199,116.341886922681));
#37766=CARTESIAN_POINT('Ctrl Pts',(6.69391876890866,1.0085701030955,116.350521829805));
#37767=CARTESIAN_POINT('Ctrl Pts',(6.66417267339425,1.18940058941265,116.35915673693));
#37768=CARTESIAN_POINT('Ctrl Pts',(6.62710294664798,1.36886651450376,116.367791644054));
#37769=CARTESIAN_POINT('Ctrl Pts',(6.58880253489332,1.55429056345799,116.376713223126));
#37770=CARTESIAN_POINT('Ctrl Pts',(6.54268384206054,1.73825756793049,116.385634802197));
#37771=CARTESIAN_POINT('Ctrl Pts',(6.4888753152869,1.9201005553513,116.394556381269));
#37772=CARTESIAN_POINT('Ctrl Pts',(6.43693962164692,2.09561440513564,116.403167440244));
#37773=CARTESIAN_POINT('Ctrl Pts',(6.37784042856936,2.26914925848573,116.41177849922));
#37774=CARTESIAN_POINT('Ctrl Pts',(6.31174519670012,2.44011507350227,116.420389558196));
#37775=CARTESIAN_POINT('Ctrl Pts',(6.24571229568589,2.61091965986242,116.428992496545));
#37776=CARTESIAN_POINT('Ctrl Pts',(6.17269661934349,2.77915975465687,116.437595434895));
#37777=CARTESIAN_POINT('Ctrl Pts',(6.09291523490216,2.94426101769139,116.446198373244));
#37778=CARTESIAN_POINT('Ctrl Pts',(6.01322318715519,3.109177405505,116.454791678293));
#37779=CARTESIAN_POINT('Ctrl Pts',(5.9267806776756,3.27096169942259,116.463384983342));
#37780=CARTESIAN_POINT('Ctrl Pts',(5.83385270556431,3.42905987258608,116.47197828839));
#37781=CARTESIAN_POINT('Ctrl Pts',(5.82349900839469,3.44667459688076,116.472935723231));
#37782=CARTESIAN_POINT('Ctrl Pts',(5.81306485201848,3.46424358452819,116.473893158072));
#37783=CARTESIAN_POINT('Ctrl Pts',(5.80255063946714,3.48176608582764,116.474850592912));
#37784=CARTESIAN_POINT('Ctrl Pts',(5.70815505444422,3.63908141050357,116.48344635046));
#37785=CARTESIAN_POINT('Ctrl Pts',(5.6074136022374,3.79246338865814,116.492042108007));
#37786=CARTESIAN_POINT('Ctrl Pts',(5.5006862180251,3.94141346864659,116.500637865555));
#37787=CARTESIAN_POINT('Ctrl Pts',(5.3938592535346,4.09050252412398,116.509241643236));
#37788=CARTESIAN_POINT('Ctrl Pts',(5.28103538684278,4.23515117942921,116.517845420918));
#37789=CARTESIAN_POINT('Ctrl Pts',(5.16261518628268,4.37489353451755,116.5264491986));
#37790=CARTESIAN_POINT('Ctrl Pts',(5.03954096828901,4.52012788635739,116.535391112268));
#37791=CARTESIAN_POINT('Ctrl Pts',(4.91042189276452,4.66006221666755,116.544333025936));
#37792=CARTESIAN_POINT('Ctrl Pts',(4.77574917437988,4.79421618446748,116.553274939604));
#37793=CARTESIAN_POINT('Ctrl Pts',(4.64581627264668,4.92364859308257,116.561902141934));
#37794=CARTESIAN_POINT('Ctrl Pts',(4.51071423877705,5.04770042059937,116.570529344265));
#37795=CARTESIAN_POINT('Ctrl Pts',(4.37091783660762,5.16598163620675,116.579156546596));
#37796=CARTESIAN_POINT('Ctrl Pts',(4.23098829976288,5.28437549656744,116.587791965016));
#37797=CARTESIAN_POINT('Ctrl Pts',(4.08635570935484,5.39698758560126,116.596427383437));
#37798=CARTESIAN_POINT('Ctrl Pts',(3.93752539171492,5.50347006802075,116.605062801857));
#37799=CARTESIAN_POINT('Ctrl Pts',(3.78847519847974,5.61010986314089,116.613710977878));
#37800=CARTESIAN_POINT('Ctrl Pts',(3.63521513783199,5.71060178466762,116.622359153899));
#37801=CARTESIAN_POINT('Ctrl Pts',(3.47827805848217,5.80464217225158,116.63100732992));
#37802=CARTESIAN_POINT('Ctrl Pts',(3.46167471054514,5.81459128868511,116.631922274152));
#37803=CARTESIAN_POINT('Ctrl Pts',(3.44503022735508,5.82446823737708,116.632837218384));
#37804=CARTESIAN_POINT('Ctrl Pts',(3.42834525442852,5.834272689585,116.633752162616));
#37805=CARTESIAN_POINT('Ctrl Pts',(3.32042649839928,5.8976880928035,116.639670041162));
#37806=CARTESIAN_POINT('Ctrl Pts',(3.21064582768168,5.95816800324278,116.645587919708));
#37807=CARTESIAN_POINT('Ctrl Pts',(3.09917575053275,6.01559628526631,116.651505798254));
#37808=CARTESIAN_POINT('Origin',(0.,0.,-3.69717978381041));
#37809=CARTESIAN_POINT('',(3.09917575053247,6.01559628526645,119.046022396269));
#37810=CARTESIAN_POINT('',(3.09917575053253,6.01559628526642,118.651527161978));
#37811=CARTESIAN_POINT('',(3.09917575053259,6.01559628526639,-3.69717978381041));
#37812=CARTESIAN_POINT('',(-6.76699965976028,-0.00214588076116945,117.697179783767));
#37813=CARTESIAN_POINT('Ctrl Pts',(-6.76699965976,-0.00214588166216128,
117.69717978381));
#37814=CARTESIAN_POINT('Ctrl Pts',(-6.76694504869395,-0.174360907245154,
117.705324442494));
#37815=CARTESIAN_POINT('Ctrl Pts',(-6.76031701235983,-0.346435165966,117.713469101178));
#37816=CARTESIAN_POINT('Ctrl Pts',(-6.74714352014871,-0.518018646879894,
117.721613759863));
#37817=CARTESIAN_POINT('Ctrl Pts',(-6.73395980007567,-0.689735344720907,
117.729764742037));
#37818=CARTESIAN_POINT('Ctrl Pts',(-6.71419573128875,-0.861218168569709,
117.737915724211));
#37819=CARTESIAN_POINT('Ctrl Pts',(-6.68785726649924,-1.03191772100945,
117.746066706386));
#37820=CARTESIAN_POINT('Ctrl Pts',(-6.66154939627771,-1.20241899009811,
117.754208220439));
#37821=CARTESIAN_POINT('Ctrl Pts',(-6.62868238682205,-1.37213844116941,
117.762349734492));
#37822=CARTESIAN_POINT('Ctrl Pts',(-6.5893141368126,-1.54052854773993,117.770491248545));
#37823=CARTESIAN_POINT('Ctrl Pts',(-6.54998333215053,-1.70875848904946,
117.778625018748));
#37824=CARTESIAN_POINT('Ctrl Pts',(-6.50416368043779,-1.87566124947419,
117.786758788951));
#37825=CARTESIAN_POINT('Ctrl Pts',(-6.45196463525836,-2.04069628935213,
117.794892559154));
#37826=CARTESIAN_POINT('Ctrl Pts',(-6.39980426098045,-2.20560906542707,
117.803020303572));
#37827=CARTESIAN_POINT('Ctrl Pts',(-6.34127401341723,-2.36865652885589,
117.81114804799));
#37828=CARTESIAN_POINT('Ctrl Pts',(-6.27653399730527,-2.52931017881777,
117.819275792408));
#37829=CARTESIAN_POINT('Ctrl Pts',(-6.21182833178989,-2.68987858708447,
117.827399224302));
#37830=CARTESIAN_POINT('Ctrl Pts',(-6.14091959589431,-2.84805537294934,
117.835522656196));
#37831=CARTESIAN_POINT('Ctrl Pts',(-6.06401713821602,-3.00332901085153,
117.84364608809));
#37832=CARTESIAN_POINT('Ctrl Pts',(-5.98662684159426,-3.15958764363878,
117.851821051841));
#37833=CARTESIAN_POINT('Ctrl Pts',(-5.90316663576624,-3.31290581242271,
117.859996015592));
#37834=CARTESIAN_POINT('Ctrl Pts',(-5.81389854146031,-3.46278395941845,
117.868170979343));
#37835=CARTESIAN_POINT('Ctrl Pts',(-5.72521328115675,-3.61168354760253,
117.876292568516));
#37836=CARTESIAN_POINT('Ctrl Pts',(-5.63079595855679,-3.75718759590019,
117.884414157689));
#37837=CARTESIAN_POINT('Ctrl Pts',(-5.53094873084053,-3.8988325351076,117.892535746862));
#37838=CARTESIAN_POINT('Ctrl Pts',(-5.43108832124234,-4.04049617435213,
117.900658408251));
#37839=CARTESIAN_POINT('Ctrl Pts',(-5.32579678955697,-4.17829939054383,
117.90878106964));
#37840=CARTESIAN_POINT('Ctrl Pts',(-5.21541850811774,-4.31180922411729,
117.91690373103));
#37841=CARTESIAN_POINT('Ctrl Pts',(-5.10500463519188,-4.44536210794841,
117.925029011572));
#37842=CARTESIAN_POINT('Ctrl Pts',(-4.98950097940368,-4.574618570468,117.933154292114));
#37843=CARTESIAN_POINT('Ctrl Pts',(-4.86929087864139,-4.69918028374947,
117.941279572657));
#37844=CARTESIAN_POINT('Ctrl Pts',(-4.74777111377544,-4.82509907105003,
117.949493376444));
#37845=CARTESIAN_POINT('Ctrl Pts',(-4.62144201836745,-4.94621993675807,
117.957707180232));
#37846=CARTESIAN_POINT('Ctrl Pts',(-4.49073559487885,-5.06217174905081,
117.96592098402));
#37847=CARTESIAN_POINT('Ctrl Pts',(-4.36121410152119,-5.17707239038764,
117.974060324875));
#37848=CARTESIAN_POINT('Ctrl Pts',(-4.2273946426779,-5.28689713218874,117.98219966573));
#37849=CARTESIAN_POINT('Ctrl Pts',(-4.08972820139918,-5.3913275024506,117.990339006586));
#37850=CARTESIAN_POINT('Ctrl Pts',(-3.95017259358062,-5.49719094790064,
117.99859004184));
#37851=CARTESIAN_POINT('Ctrl Pts',(-3.80666397681182,-5.59751067173597,
118.006841077094));
#37852=CARTESIAN_POINT('Ctrl Pts',(-3.65969912910448,-5.69200239673455,
118.015092112348));
#37853=CARTESIAN_POINT('Ctrl Pts',(-3.51273428139714,-5.78649412173314,
118.023343147602));
#37854=CARTESIAN_POINT('Ctrl Pts',(-3.36231356751004,-5.87515771074063,
118.031594182856));
#37855=CARTESIAN_POINT('Ctrl Pts',(-3.20895558971995,-5.95775906051974,
118.03984521811));
#37856=CARTESIAN_POINT('Ctrl Pts',(-3.05595564808691,-6.04016756562088,
118.048076990141));
#37857=CARTESIAN_POINT('Ctrl Pts',(-2.89955458742374,-6.11679952677498,
118.056308762171));
#37858=CARTESIAN_POINT('Ctrl Pts',(-2.74022712140345,-6.18736166092826,
118.064540534202));
#37859=CARTESIAN_POINT('Ctrl Pts',(-2.58108990829981,-6.25783953684181,
118.072762476675));
#37860=CARTESIAN_POINT('Ctrl Pts',(-2.41903357242951,-6.32226187449051,
118.080984419147));
#37861=CARTESIAN_POINT('Ctrl Pts',(-2.25455900449175,-6.38038029393744,
118.089206361619));
#37862=CARTESIAN_POINT('Ctrl Pts',(-2.0902478816989,-6.43844095871987,118.097420133609));
#37863=CARTESIAN_POINT('Ctrl Pts',(-1.92352364810583,-6.49021006239716,
118.105633905599));
#37864=CARTESIAN_POINT('Ctrl Pts',(-1.75490892751252,-6.53548648963005,
118.113847677589));
#37865=CARTESIAN_POINT('Ctrl Pts',(-1.58642799513494,-6.58072699204929,
118.122054932319));
#37866=CARTESIAN_POINT('Ctrl Pts',(-1.41605990795835,-6.61948498648544,
118.13026218705));
#37867=CARTESIAN_POINT('Ctrl Pts',(-1.24434436731198,-6.65160853444781,
118.13846944178));
#37868=CARTESIAN_POINT('Ctrl Pts',(-1.07273069198314,-6.68371302603706,
118.146671827792));
#37869=CARTESIAN_POINT('Ctrl Pts',(-0.899771506820508,-6.70919084581187,
118.154874213804));
#37870=CARTESIAN_POINT('Ctrl Pts',(-0.72601876911571,-6.72794067652887,
118.163076599816));
#37871=CARTESIAN_POINT('Ctrl Pts',(-0.552317892388534,-6.7466849108762,
118.171276537615));
#37872=CARTESIAN_POINT('Ctrl Pts',(-0.377824290307473,-6.75870511405056,
118.179476475413));
#37873=CARTESIAN_POINT('Ctrl Pts',(-0.203097394712037,-6.76395154094566,
118.187676413212));
#37874=CARTESIAN_POINT('Ctrl Pts',(-0.0283949304464053,-6.76919723425487,
118.195875204448));
#37875=CARTESIAN_POINT('Ctrl Pts',(0.146540404253272,-6.76767102608828,
118.204073995684));
#37876=CARTESIAN_POINT('Ctrl Pts',(0.321146783002885,-6.75937524803638,
118.212272786919));
#37877=CARTESIAN_POINT('Ctrl Pts',(0.495760421777843,-6.75107912505116,
118.220471919056));
#37878=CARTESIAN_POINT('Ctrl Pts',(0.670044719306279,-6.73601288834823,
118.228671051192));
#37879=CARTESIAN_POINT('Ctrl Pts',(0.843440522287577,-6.71423093774434,
118.236870183329));
#37880=CARTESIAN_POINT('Ctrl Pts',(1.01687498974217,-6.69244413011605,118.245071143739));
#37881=CARTESIAN_POINT('Ctrl Pts',(1.18942021249064,-6.66393867067187,118.25327210415));
#37882=CARTESIAN_POINT('Ctrl Pts',(1.36052475185444,-6.62882051345422,118.261473064561));
#37883=CARTESIAN_POINT('Ctrl Pts',(1.53178965736135,-6.59366944206931,118.269681711246));
#37884=CARTESIAN_POINT('Ctrl Pts',(1.70161083016143,-6.55189336246376,118.277890357931));
#37885=CARTESIAN_POINT('Ctrl Pts',(1.86944865365989,-6.50364903199191,118.286099004616));
#37886=CARTESIAN_POINT('Ctrl Pts',(2.03736660764926,-6.45538166832167,118.29431157034));
#37887=CARTESIAN_POINT('Ctrl Pts',(2.20329898416183,-6.40064000882376,118.302524136063));
#37888=CARTESIAN_POINT('Ctrl Pts',(2.36672389167267,-6.33962988040988,118.310736701787));
#37889=CARTESIAN_POINT('Ctrl Pts',(2.53037304173894,-6.27853603729601,118.318960536336));
#37890=CARTESIAN_POINT('Ctrl Pts',(2.69150751577272,-6.21115667357201,118.327184370884));
#37891=CARTESIAN_POINT('Ctrl Pts',(2.84962674316229,-6.13774522317881,118.335408205433));
#37892=CARTESIAN_POINT('Ctrl Pts',(2.99490856951235,-6.07029390960862,118.342964362408));
#37893=CARTESIAN_POINT('Ctrl Pts',(3.1376449655099,-5.99775085225321,118.350520519382));
#37894=CARTESIAN_POINT('Ctrl Pts',(3.2774684587162,-5.9203453870632,118.358076676357));
#37895=CARTESIAN_POINT('Ctrl Pts',(3.43745381945471,-5.83177843034095,118.366722394409));
#37896=CARTESIAN_POINT('Ctrl Pts',(3.59399015459903,-5.73664356539932,118.375368112462));
#37897=CARTESIAN_POINT('Ctrl Pts',(3.74653508863061,-5.63522526875897,118.384013830514));
#37898=CARTESIAN_POINT('Ctrl Pts',(3.89888418605455,-5.53393717254313,118.392648449226));
#37899=CARTESIAN_POINT('Ctrl Pts',(4.04725184741961,-5.4263818979817,118.401283067939));
#37900=CARTESIAN_POINT('Ctrl Pts',(4.19112129721432,-5.31288916429061,118.409917686651));
#37901=CARTESIAN_POINT('Ctrl Pts',(4.34007165708638,-5.19538830813057,118.418857246553));
#37902=CARTESIAN_POINT('Ctrl Pts',(4.48419999310274,-5.07152309302713,118.427796806456));
#37903=CARTESIAN_POINT('Ctrl Pts',(4.62296408571115,-4.94170942713398,118.436736366358));
#37904=CARTESIAN_POINT('Ctrl Pts',(4.75662273344032,-4.81667189967356,118.445347019629));
#37905=CARTESIAN_POINT('Ctrl Pts',(4.88530453657023,-4.68611603151257,118.453957672899));
#37906=CARTESIAN_POINT('Ctrl Pts',(5.00855689322294,-4.55045567469336,118.46256832617));
#37907=CARTESIAN_POINT('Ctrl Pts',(5.13169258327398,-4.41492372947812,118.471170828881));
#37908=CARTESIAN_POINT('Ctrl Pts',(5.24940886888443,-4.27429715378923,118.479773331592));
#37909=CARTESIAN_POINT('Ctrl Pts',(5.36128939345573,-4.12902712992045,118.488375834303));
#37910=CARTESIAN_POINT('Ctrl Pts',(5.47304399874879,-3.98392060453924,118.496968655071));
#37911=CARTESIAN_POINT('Ctrl Pts',(5.57897576032858,-3.83418129802877,118.505561475838));
#37912=CARTESIAN_POINT('Ctrl Pts',(5.67870794407446,-3.68029415752405,118.514154296606));
#37913=CARTESIAN_POINT('Ctrl Pts',(5.69046183493653,-3.66215785902308,118.515166999564));
#37914=CARTESIAN_POINT('Ctrl Pts',(5.70212966133994,-3.64396398641442,118.516179702522));
#37915=CARTESIAN_POINT('Ctrl Pts',(5.71371084367568,-3.62571336358281,118.51719240548));
#37916=CARTESIAN_POINT('Ctrl Pts',(5.8120054586408,-3.47081225831558,118.52578766324));
#37917=CARTESIAN_POINT('Ctrl Pts',(5.90393935173546,-3.31200290125589,118.534382921));
#37918=CARTESIAN_POINT('Ctrl Pts',(5.98922837091472,-3.14983055433626,118.54297817876));
#37919=CARTESIAN_POINT('Ctrl Pts',(6.07459725964346,-2.98750633989121,118.551581485614));
#37920=CARTESIAN_POINT('Ctrl Pts',(6.15330871169246,-2.82181311972006,118.560184792469));
#37921=CARTESIAN_POINT('Ctrl Pts',(6.22512598319935,-2.65331782741841,118.568788099323));
#37922=CARTESIAN_POINT('Ctrl Pts',(6.29992082368746,-2.47783666186772,118.577748102263));
#37923=CARTESIAN_POINT('Ctrl Pts',(6.36723749480628,-2.29931647923578,118.586708105203));
#37924=CARTESIAN_POINT('Ctrl Pts',(6.42686576106905,-2.11841579705175,118.595668108143));
#37925=CARTESIAN_POINT('Ctrl Pts',(6.48427686986682,-1.94424154384286,118.604294951348));
#37926=CARTESIAN_POINT('Ctrl Pts',(6.53456098319151,-1.7678609244091,118.612921794553));
#37927=CARTESIAN_POINT('Ctrl Pts',(6.57758255417386,-1.58987318457405,118.621548637758));
#37928=CARTESIAN_POINT('Ctrl Pts',(6.62064524290299,-1.41171533345186,118.630183726044));
#37929=CARTESIAN_POINT('Ctrl Pts',(6.65643147161972,-1.23194759428447,118.63881881433));
#37930=CARTESIAN_POINT('Ctrl Pts',(6.68485711682837,-1.05117759088991,118.647453902616));
#37931=CARTESIAN_POINT('Ctrl Pts',(6.71332497982467,-0.870139107762965,
118.656101815741));
#37932=CARTESIAN_POINT('Ctrl Pts',(6.73441037409266,-0.688095688152995,
118.664749728866));
#37933=CARTESIAN_POINT('Ctrl Pts',(6.74808100361623,-0.505659736021951,
118.673397641991));
#37934=CARTESIAN_POINT('Ctrl Pts',(6.74961464013867,-0.485193199443509,
118.674367806195));
#37935=CARTESIAN_POINT('Ctrl Pts',(6.75105501267373,-0.464721721982968,
118.675337970399));
#37936=CARTESIAN_POINT('Ctrl Pts',(6.75240211649703,-0.444246167261397,
118.676308134604));
#37937=CARTESIAN_POINT('Ctrl Pts',(6.76382234533885,-0.270662278225858,
118.684532814122));
#37938=CARTESIAN_POINT('Ctrl Pts',(6.76855984801392,-0.0964089831302133,
118.692757493641));
#37939=CARTESIAN_POINT('Ctrl Pts',(6.76655092705844,0.077958652659838,118.70098217316));
#37940=CARTESIAN_POINT('Ctrl Pts',(6.76454411770616,0.252143008338005,118.70919820761));
#37941=CARTESIAN_POINT('Ctrl Pts',(6.75580501001684,0.426441109936801,118.71741424206));
#37942=CARTESIAN_POINT('Ctrl Pts',(6.74032171528204,0.600293407008072,118.72563027651));
#37943=CARTESIAN_POINT('Ctrl Pts',(6.72485159391047,0.773997788568004,118.733839320665));
#37944=CARTESIAN_POINT('Ctrl Pts',(6.70264874507641,0.94725676601518,118.74204836482));
#37945=CARTESIAN_POINT('Ctrl Pts',(6.67375332031211,1.11951133072567,118.750257408974));
#37946=CARTESIAN_POINT('Ctrl Pts',(6.64487669393412,1.29165383244077,118.758461112602));
#37947=CARTESIAN_POINT('Ctrl Pts',(6.60931622341778,1.46279287079096,118.76666481623));
#37948=CARTESIAN_POINT('Ctrl Pts',(6.56716383560898,1.63237500479198,118.774868519858));
#37949=CARTESIAN_POINT('Ctrl Pts',(6.52503043162206,1.80188076549141,118.783068528852));
#37950=CARTESIAN_POINT('Ctrl Pts',(6.47631111118444,1.96983067165326,118.791268537846));
#37951=CARTESIAN_POINT('Ctrl Pts',(6.42114881779871,2.13568182547922,118.79946854684));
#37952=CARTESIAN_POINT('Ctrl Pts',(6.36599093530634,2.301519717497,118.807667900144));
#37953=CARTESIAN_POINT('Ctrl Pts',(6.30439121079043,2.46525884885741,118.815867253448));
#37954=CARTESIAN_POINT('Ctrl Pts',(6.23654246216152,2.62637147366025,118.824066606752));
#37955=CARTESIAN_POINT('Ctrl Pts',(6.16869415588639,2.78748304805641,118.832265906599));
#37956=CARTESIAN_POINT('Ctrl Pts',(6.09459704479391,2.94596781916997,118.840465206445));
#37957=CARTESIAN_POINT('Ctrl Pts',(6.01449206460866,3.10131813988174,118.848664506292));
#37958=CARTESIAN_POINT('Ctrl Pts',(5.93437307485473,3.25669562982793,118.856865240115));
#37959=CARTESIAN_POINT('Ctrl Pts',(5.84824428694125,3.40893725855291,118.865065973938));
#37960=CARTESIAN_POINT('Ctrl Pts',(5.75639257376828,3.55756005383822,118.873266707761));
#37961=CARTESIAN_POINT('Ctrl Pts',(5.66450813365637,3.70623580370629,118.881470363521));
#37962=CARTESIAN_POINT('Ctrl Pts',(5.56689689467701,3.8512898468071,118.889674019281));
#37963=CARTESIAN_POINT('Ctrl Pts',(5.46388904065899,3.99226822137073,118.897877675041));
#37964=CARTESIAN_POINT('Ctrl Pts',(5.36076318452232,4.13340809572523,118.906090728616));
#37965=CARTESIAN_POINT('Ctrl Pts',(5.25222857406988,4.27046268395185,118.914303782191));
#37966=CARTESIAN_POINT('Ctrl Pts',(5.13865634582895,4.40301032924883,118.922516835766));
#37967=CARTESIAN_POINT('Ctrl Pts',(5.0250169143524,4.53563640596144,118.930734749189));
#37968=CARTESIAN_POINT('Ctrl Pts',(4.90633416633753,4.6637499611273,118.938952662612));
#37969=CARTESIAN_POINT('Ctrl Pts',(4.78301599943664,4.78696636181342,118.947170576035));
#37970=CARTESIAN_POINT('Ctrl Pts',(4.65950549779279,4.91037493852152,118.955401306631));
#37971=CARTESIAN_POINT('Ctrl Pts',(4.53134539233315,5.02887085370543,118.963632037227));
#37972=CARTESIAN_POINT('Ctrl Pts',(4.3989775666484,5.14210903891819,118.971862767823));
#37973=CARTESIAN_POINT('Ctrl Pts',(4.27741354964925,5.24610476900551,118.979421709499));
#37974=CARTESIAN_POINT('Ctrl Pts',(4.15230118454081,5.34566636734905,118.986980651174));
#37975=CARTESIAN_POINT('Ctrl Pts',(4.02400328533236,5.44055939767543,118.99453959285));
#37976=CARTESIAN_POINT('Ctrl Pts',(3.87836703519418,5.54827639995095,119.003120060086));
#37977=CARTESIAN_POINT('Ctrl Pts',(3.72815140859379,5.65032716849108,119.011700527323));
#37978=CARTESIAN_POINT('Ctrl Pts',(3.57384383489437,5.74629700274773,119.020280994559));
#37979=CARTESIAN_POINT('Ctrl Pts',(3.42736941710198,5.83739509509255,119.028425889283));
#37980=CARTESIAN_POINT('Ctrl Pts',(3.27720854587081,5.92301404249656,119.036570784007));
#37981=CARTESIAN_POINT('Ctrl Pts',(3.12381322269131,6.00283932399818,119.04471567873));
#37982=CARTESIAN_POINT('Ctrl Pts',(3.11560995074811,6.00710821876321,119.045151251243));
#37983=CARTESIAN_POINT('Ctrl Pts',(3.1073974361474,6.01136055409734,119.045586823756));
#37984=CARTESIAN_POINT('Ctrl Pts',(3.09917575053247,6.01559628526645,119.046022396269));
#37985=CARTESIAN_POINT('Ctrl Pts',(3.09917575053267,6.01559628526635,117.045557306694));
#37986=CARTESIAN_POINT('Ctrl Pts',(2.9453982607291,6.09482092814078,117.053708314557));
#37987=CARTESIAN_POINT('Ctrl Pts',(2.78876066226697,6.16805262932651,117.061859322421));
#37988=CARTESIAN_POINT('Ctrl Pts',(2.62978194551124,6.23510512494081,117.070010330285));
#37989=CARTESIAN_POINT('Ctrl Pts',(2.53134751950769,6.27662183895505,117.075057167979));
#37990=CARTESIAN_POINT('Ctrl Pts',(2.43201590677253,6.31577062340739,117.080104005674));
#37991=CARTESIAN_POINT('Ctrl Pts',(2.33191274168623,6.35251697873854,117.085150843369));
#37992=CARTESIAN_POINT('Ctrl Pts',(2.16877389381462,6.41240277822386,117.093375711047));
#37993=CARTESIAN_POINT('Ctrl Pts',(2.00309764348051,6.46608426494995,117.101600578725));
#37994=CARTESIAN_POINT('Ctrl Pts',(1.83539640369543,6.51334085099973,117.109825446402));
#37995=CARTESIAN_POINT('Ctrl Pts',(1.66788409812793,6.56054419721585,117.118041047846));
#37996=CARTESIAN_POINT('Ctrl Pts',(1.4983516880867,6.60133695977287,117.126256649289));
#37997=CARTESIAN_POINT('Ctrl Pts',(1.32733086418371,6.6355468333051,117.134472250733));
#37998=CARTESIAN_POINT('Ctrl Pts',(1.15646835286588,6.66972503903575,117.142680247061));
#37999=CARTESIAN_POINT('Ctrl Pts',(0.984120521212369,6.69733242159352,117.150888243389));
#38000=CARTESIAN_POINT('Ctrl Pts',(0.810833588233664,6.7182466382377,117.159096239717));
#38001=CARTESIAN_POINT('Ctrl Pts',(0.637672259977481,6.73914569549084,117.167298286589));
#38002=CARTESIAN_POINT('Ctrl Pts',(0.463573540954107,6.75336120719183,117.17550033346));
#38003=CARTESIAN_POINT('Ctrl Pts',(0.289093286210853,6.76082199675955,117.183702380331));
#38004=CARTESIAN_POINT('Ctrl Pts',(0.114704463957067,6.76827887666675,117.191900129103));
#38005=CARTESIAN_POINT('Ctrl Pts',(-0.0600651381189869,6.76898807072145,
117.200097877874));
#38006=CARTESIAN_POINT('Ctrl Pts',(-0.234655016416447,6.76293028378015,
117.208295626646));
#38007=CARTESIAN_POINT('Ctrl Pts',(-0.409211595201144,6.75687365224003,
117.216491811862));
#38008=CARTESIAN_POINT('Ctrl Pts',(-0.583588160078158,6.74405261676008,
117.224687997077));
#38009=CARTESIAN_POINT('Ctrl Pts',(-0.757224370010675,6.72450000025741,
117.232884182293));
#38010=CARTESIAN_POINT('Ctrl Pts',(-0.930847734728392,6.70494883021318,
117.241079761173));
#38011=CARTESIAN_POINT('Ctrl Pts',(-1.10373049690652,6.67866711016436,117.249275340054));
#38012=CARTESIAN_POINT('Ctrl Pts',(-1.27531765423223,6.64573952851025,117.257470918934));
#38013=CARTESIAN_POINT('Ctrl Pts',(-1.44692333617855,6.61280839198077,117.265667382612));
#38014=CARTESIAN_POINT('Ctrl Pts',(-1.61723278212875,6.57323003202636,117.273863846291));
#38015=CARTESIAN_POINT('Ctrl Pts',(-1.7857013446595,6.52714023962112,117.282060309969));
#38016=CARTESIAN_POINT('Ctrl Pts',(-1.95421874611441,6.48103708581574,117.290259149797));
#38017=CARTESIAN_POINT('Ctrl Pts',(-2.12089385512129,6.4284188342491,117.298457989625));
#38018=CARTESIAN_POINT('Ctrl Pts',(-2.28519729395325,6.3694711183668,117.306656829453));
#38019=CARTESIAN_POINT('Ctrl Pts',(-2.449672352401,6.31046182991837,117.314864233202));
#38020=CARTESIAN_POINT('Ctrl Pts',(-2.61177045319455,6.2451099899666,117.323071636951));
#38021=CARTESIAN_POINT('Ctrl Pts',(-2.77098138350577,6.17364974486441,117.3312790407));
#38022=CARTESIAN_POINT('Ctrl Pts',(-2.93027759561667,6.1021512218733,117.339490840769));
#38023=CARTESIAN_POINT('Ctrl Pts',(-3.08668323308861,6.02453793029808,117.347702640839));
#38024=CARTESIAN_POINT('Ctrl Pts',(-3.23971291027645,5.94108990497435,117.355914440908));
#38025=CARTESIAN_POINT('Ctrl Pts',(-3.39296786853188,5.85751903249718,117.364138329894));
#38026=CARTESIAN_POINT('Ctrl Pts',(-3.54283662617595,5.76809644417329,117.37236221888));
#38027=CARTESIAN_POINT('Ctrl Pts',(-3.68886190994425,5.67314611211121,117.380586107866));
#38028=CARTESIAN_POINT('Ctrl Pts',(-3.82378674768664,5.58541364677054,117.388184839116));
#38029=CARTESIAN_POINT('Ctrl Pts',(-3.95543040198791,5.4929625013917,117.395783570366));
#38030=CARTESIAN_POINT('Ctrl Pts',(-4.08345817322501,5.39607805239341,117.403382301616));
#38031=CARTESIAN_POINT('Ctrl Pts',(-4.22049288443249,5.29237764145375,117.411515614665));
#38032=CARTESIAN_POINT('Ctrl Pts',(-4.35378887719579,5.18329172566531,117.419648927713));
#38033=CARTESIAN_POINT('Ctrl Pts',(-4.48288915904276,5.06912159922574,117.427782240762));
#38034=CARTESIAN_POINT('Ctrl Pts',(-4.61184316092746,4.95508083580187,117.435906338178));
#38035=CARTESIAN_POINT('Ctrl Pts',(-4.73661064209647,4.83596756979668,117.444030435595));
#38036=CARTESIAN_POINT('Ctrl Pts',(-4.85676435033687,4.71212574591308,117.452154533011));
#38037=CARTESIAN_POINT('Ctrl Pts',(-4.97680748888239,4.58839788565891,117.460271154346));
#38038=CARTESIAN_POINT('Ctrl Pts',(-5.09224505258917,4.4599503924961,117.46838777568));
#38039=CARTESIAN_POINT('Ctrl Pts',(-5.20268363544236,4.32716673927643,117.476504397014));
#38040=CARTESIAN_POINT('Ctrl Pts',(-5.31304407869666,4.19447703566328,117.484615275523));
#38041=CARTESIAN_POINT('Ctrl Pts',(-5.4184123495223,4.05745756245719,117.492726154032));
#38042=CARTESIAN_POINT('Ctrl Pts',(-5.51843265836311,3.91652779833254,117.50083703254));
#38043=CARTESIAN_POINT('Ctrl Pts',(-5.6193170374688,3.77438054927878,117.509017980508));
#38044=CARTESIAN_POINT('Ctrl Pts',(-5.71476035001969,3.6282553980885,117.517198928476));
#38045=CARTESIAN_POINT('Ctrl Pts',(-5.80443930936039,3.47861657903711,117.525379876444));
#38046=CARTESIAN_POINT('Ctrl Pts',(-5.89329220727498,3.33035613075604,117.533485467097));
#38047=CARTESIAN_POINT('Ctrl Pts',(-5.97648632005189,3.17864680254795,117.54159105775));
#38048=CARTESIAN_POINT('Ctrl Pts',(-6.05375118196756,3.02396852279028,117.549696648403));
#38049=CARTESIAN_POINT('Ctrl Pts',(-6.13101408251005,2.86929416955006,117.557802033296));
#38050=CARTESIAN_POINT('Ctrl Pts',(-6.20234786721487,2.71165134378101,117.565907418188));
#38051=CARTESIAN_POINT('Ctrl Pts',(-6.2675286300987,2.55154342916069,117.57401280308));
#38052=CARTESIAN_POINT('Ctrl Pts',(-6.33272028813418,2.39140875204278,117.582119542811));
#38053=CARTESIAN_POINT('Ctrl Pts',(-6.39175673831599,2.22880850653348,117.590226282542));
#38054=CARTESIAN_POINT('Ctrl Pts',(-6.44446273376663,2.06426477785508,117.598333022273));
#38055=CARTESIAN_POINT('Ctrl Pts',(-6.49801711294893,1.89707246581607,117.606570252397));
#38056=CARTESIAN_POINT('Ctrl Pts',(-6.54503536796367,1.72787394132357,117.614807482522));
#38057=CARTESIAN_POINT('Ctrl Pts',(-6.58538694221708,1.55723081824014,117.623044712646));
#38058=CARTESIAN_POINT('Ctrl Pts',(-6.62515362267665,1.38906115760513,117.631162544585));
#38059=CARTESIAN_POINT('Ctrl Pts',(-6.65844556932252,1.21948886721027,117.639280376523));
#38060=CARTESIAN_POINT('Ctrl Pts',(-6.68518986990649,1.04905929446319,117.647398208461));
#38061=CARTESIAN_POINT('Ctrl Pts',(-6.71252420875555,0.874869669397403,
117.655695137679));
#38062=CARTESIAN_POINT('Ctrl Pts',(-6.73301859881323,0.699784906238783,
117.663992066897));
#38063=CARTESIAN_POINT('Ctrl Pts',(-6.74665135838064,0.524389596064545,
117.672288996114));
#38064=CARTESIAN_POINT('Ctrl Pts',(-6.76028411794805,0.34899428589018,117.680585925332));
#38065=CARTESIAN_POINT('Ctrl Pts',(-6.76705529179801,0.173288834536322,
117.68888285455));
#38066=CARTESIAN_POINT('Ctrl Pts',(-6.76699965976028,-0.00214588076117313,
117.697179783767));
#38067=CARTESIAN_POINT('',(-6.76699928917358,0.00310166475318471,117.302820216236));
#38068=CARTESIAN_POINT('Ctrl Pts',(3.09917575053275,6.01559628526631,116.651505798254));
#38069=CARTESIAN_POINT('Ctrl Pts',(2.94434967243014,6.0953611504686,116.659725420501));
#38070=CARTESIAN_POINT('Ctrl Pts',(2.78626342730763,6.16923703737558,116.667945042748));
#38071=CARTESIAN_POINT('Ctrl Pts',(2.62540469763848,6.2369495086635,116.676164664995));
#38072=CARTESIAN_POINT('Ctrl Pts',(2.46469145438008,6.30460073836116,116.684376853121));
#38073=CARTESIAN_POINT('Ctrl Pts',(2.30121104862397,6.36609951607871,116.692589041246));
#38074=CARTESIAN_POINT('Ctrl Pts',(2.13547527859082,6.42121751185299,116.700801229372));
#38075=CARTESIAN_POINT('Ctrl Pts',(1.96985624995048,6.47629668347002,116.709007632975));
#38076=CARTESIAN_POINT('Ctrl Pts',(1.8019853599386,6.52500391289286,116.717214036578));
#38077=CARTESIAN_POINT('Ctrl Pts',(1.63239397125315,6.56715912115858,116.725420440181));
#38078=CARTESIAN_POINT('Ctrl Pts',(1.46288812002016,6.6092930674419,116.733622704689));
#38079=CARTESIAN_POINT('Ctrl Pts',(1.2916638457297,6.64488148983721,116.741824969197));
#38080=CARTESIAN_POINT('Ctrl Pts',(1.11926733503408,6.67379424560914,116.750027233705));
#38081=CARTESIAN_POINT('Ctrl Pts',(0.94277778271374,6.70339344864375,116.758424236552));
#38082=CARTESIAN_POINT('Ctrl Pts',(0.765060007341705,6.72599593777454,116.766821239399));
#38083=CARTESIAN_POINT('Ctrl Pts',(0.586711333395185,6.74151754512778,116.775218242245));
#38084=CARTESIAN_POINT('Ctrl Pts',(0.41253453544973,6.75667607593112,116.783418825046));
#38085=CARTESIAN_POINT('Ctrl Pts',(0.237756399157399,6.76508129044165,116.791619407847));
#38086=CARTESIAN_POINT('Ctrl Pts',(0.0629384146720956,6.76670730532647,
116.799819990648));
#38087=CARTESIAN_POINT('Ctrl Pts',(-0.111902228408066,6.76833353096313,
116.808021636347));
#38088=CARTESIAN_POINT('Ctrl Pts',(-0.28678237158857,6.76317880280661,116.816223282046));
#38089=CARTESIAN_POINT('Ctrl Pts',(-0.461140661102264,6.75126938365506,
116.824424927745));
#38090=CARTESIAN_POINT('Ctrl Pts',(-0.635553147909284,6.73935626259587,
116.832629122833));
#38091=CARTESIAN_POINT('Ctrl Pts',(-0.809443100514926,6.72068429234751,
116.84083331792));
#38092=CARTESIAN_POINT('Ctrl Pts',(-0.982254361380472,6.69533161012575,
116.849037513008));
#38093=CARTESIAN_POINT('Ctrl Pts',(-1.16220527056132,6.668931489016,116.857580662092));
#38094=CARTESIAN_POINT('Ctrl Pts',(-1.34098602962433,6.63528693847101,116.866123811177));
#38095=CARTESIAN_POINT('Ctrl Pts',(-1.51798141790123,6.59454482242001,116.874666960261));
#38096=CARTESIAN_POINT('Ctrl Pts',(-1.68824379914598,6.55535256004908,116.882885123009));
#38097=CARTESIAN_POINT('Ctrl Pts',(-1.85685381083841,6.50959291716969,116.891103285757));
#38098=CARTESIAN_POINT('Ctrl Pts',(-2.02328052428725,6.45744724485148,116.899321448505));
#38099=CARTESIAN_POINT('Ctrl Pts',(-2.18982705907041,6.40526402949761,116.907545528039));
#38100=CARTESIAN_POINT('Ctrl Pts',(-2.35418682673733,6.34668574115767,116.915769607572));
#38101=CARTESIAN_POINT('Ctrl Pts',(-2.51584920345394,6.28194172095541,116.923993687106));
#38102=CARTESIAN_POINT('Ctrl Pts',(-2.67772702715645,6.21711141658307,116.932228726847));
#38103=CARTESIAN_POINT('Ctrl Pts',(-2.83689995803201,6.14609912122177,116.940463766588));
#38104=CARTESIAN_POINT('Ctrl Pts',(-2.9928815796825,6.06918024530473,116.948698806329));
#38105=CARTESIAN_POINT('Ctrl Pts',(-3.01091674181233,6.06028660525067,116.94965097156));
#38106=CARTESIAN_POINT('Ctrl Pts',(-3.02890927166878,6.0513140488267,116.950603136792));
#38107=CARTESIAN_POINT('Ctrl Pts',(-3.0468584428216,6.04226303874688,116.951555302023));
#38108=CARTESIAN_POINT('Ctrl Pts',(-3.20059617020903,5.96473958608241,116.95971076043));
#38109=CARTESIAN_POINT('Ctrl Pts',(-3.35162399650535,5.88121836395444,116.967866218837));
#38110=CARTESIAN_POINT('Ctrl Pts',(-3.49943530889714,5.79191173265305,116.976021677244));
#38111=CARTESIAN_POINT('Ctrl Pts',(-3.64706671549235,5.70271379926106,116.984167209385));
#38112=CARTESIAN_POINT('Ctrl Pts',(-3.79148909161224,5.60774466026573,116.992312741527));
#38113=CARTESIAN_POINT('Ctrl Pts',(-3.93221707123081,5.50726410341115,117.000458273669));
#38114=CARTESIAN_POINT('Ctrl Pts',(-4.0728033586708,5.40688471555682,117.00859560447));
#38115=CARTESIAN_POINT('Ctrl Pts',(-4.20970235965384,5.30100516807636,117.01673293527));
#38116=CARTESIAN_POINT('Ctrl Pts',(-4.3424545479687,5.1899303944105,117.024870266071));
#38117=CARTESIAN_POINT('Ctrl Pts',(-4.47510097282572,5.07894411384063,117.033001113873));
#38118=CARTESIAN_POINT('Ctrl Pts',(-4.60360688419332,4.96277108186089,117.041131961675));
#38119=CARTESIAN_POINT('Ctrl Pts',(-4.72754293730218,4.84175864495168,117.049262809477));
#38120=CARTESIAN_POINT('Ctrl Pts',(-4.85140628566751,4.72081719770179,117.057388887471));
#38121=CARTESIAN_POINT('Ctrl Pts',(-4.97070485371655,4.59504225393221,117.065514965465));
#38122=CARTESIAN_POINT('Ctrl Pts',(-5.08504352387437,4.46482041747519,117.073641043459));
#38123=CARTESIAN_POINT('Ctrl Pts',(-5.1997876180731,4.33413683817055,117.081795935041));
#38124=CARTESIAN_POINT('Ctrl Pts',(-5.30953629481107,4.1989750158833,117.089950826623));
#38125=CARTESIAN_POINT('Ctrl Pts',(-5.41392822995811,4.05976232319858,117.098105718205));
#38126=CARTESIAN_POINT('Ctrl Pts',(-5.51791307305772,3.92109251134091,117.106228808561));
#38127=CARTESIAN_POINT('Ctrl Pts',(-5.61658267113772,3.77840367128628,117.114351898918));
#38128=CARTESIAN_POINT('Ctrl Pts',(-5.70962111670077,3.63215028650036,117.122474989274));
#38129=CARTESIAN_POINT('Ctrl Pts',(-5.80266686806748,3.48588541723072,117.130598717492));
#38130=CARTESIAN_POINT('Ctrl Pts',(-5.89008038974256,3.33605575433806,117.138722445711));
#38131=CARTESIAN_POINT('Ctrl Pts',(-5.9715899829251,3.18314342683905,117.146846173929));
#38132=CARTESIAN_POINT('Ctrl Pts',(-6.05312148371636,3.03019000057718,117.15497208559));
#38133=CARTESIAN_POINT('Ctrl Pts',(-6.12874572435242,2.87415258262508,117.16309799725));
#38134=CARTESIAN_POINT('Ctrl Pts',(-6.19823772506012,2.71553643018125,117.17122390891));
#38135=CARTESIAN_POINT('Ctrl Pts',(-6.2681741343358,2.55590591095495,117.17940178662));
#38136=CARTESIAN_POINT('Ctrl Pts',(-6.33189944809649,2.39366390423532,117.187579664331));
#38137=CARTESIAN_POINT('Ctrl Pts',(-6.38923443824757,2.22934346683306,117.195757542041));
#38138=CARTESIAN_POINT('Ctrl Pts',(-6.44629578092607,2.06580729523899,117.203896388514));
#38139=CARTESIAN_POINT('Ctrl Pts',(-6.49702761724099,1.90021285710961,117.212035234988));
#38140=CARTESIAN_POINT('Ctrl Pts',(-6.54130415551225,1.73309807716651,117.220174081461));
#38141=CARTESIAN_POINT('Ctrl Pts',(-6.5858991974032,1.56478115576442,117.228371474789));
#38142=CARTESIAN_POINT('Ctrl Pts',(-6.6239456360603,1.39492230552711,117.236568868118));
#38143=CARTESIAN_POINT('Ctrl Pts',(-6.65536785607931,1.22407830642747,117.244766261446));
#38144=CARTESIAN_POINT('Ctrl Pts',(-6.68679007609832,1.05323430732783,117.252963654774));
#38145=CARTESIAN_POINT('Ctrl Pts',(-6.71158808479465,0.881405536510773,
117.261161048103));
#38146=CARTESIAN_POINT('Ctrl Pts',(-6.72973958167842,0.70915031043549,117.269358441431));
#38147=CARTESIAN_POINT('Ctrl Pts',(-6.75443772965151,0.474768259743667,
117.280512366351));
#38148=CARTESIAN_POINT('Ctrl Pts',(-6.76689111546283,0.239107568829402,
117.29166629127));
#38149=CARTESIAN_POINT('Ctrl Pts',(-6.76699928917314,0.00310166572580796,
117.30282021619));
#38150=CARTESIAN_POINT('Ctrl Pts',(-6.76699928917358,0.00310166475299538,
117.302820216236));
#38151=CARTESIAN_POINT('Ctrl Pts',(-6.76707794204855,-0.168497779856733,
117.310930213894));
#38152=CARTESIAN_POINT('Ctrl Pts',(-6.76062520672312,-0.340352238830547,
117.319040211552));
#38153=CARTESIAN_POINT('Ctrl Pts',(-6.74760921640779,-0.5119168513037,117.327150209209));
#38154=CARTESIAN_POINT('Ctrl Pts',(-6.73460661988539,-0.68330491932353,
117.335251861468));
#38155=CARTESIAN_POINT('Ctrl Pts',(-6.71505423919447,-0.854403369158645,
117.343353513727));
#38156=CARTESIAN_POINT('Ctrl Pts',(-6.68897219997428,-1.02466575426877,
117.351455165986));
#38157=CARTESIAN_POINT('Ctrl Pts',(-6.6629113960377,-1.19478951639763,117.359550222101));
#38158=CARTESIAN_POINT('Ctrl Pts',(-6.63033157275093,-1.36407820561675,
117.367645278217));
#38159=CARTESIAN_POINT('Ctrl Pts',(-6.59130478648699,-1.53198897242564,
117.375740334332));
#38160=CARTESIAN_POINT('Ctrl Pts',(-6.55230139537651,-1.6997990827743,117.383830537752));
#38161=CARTESIAN_POINT('Ctrl Pts',(-6.50685881998188,-1.86623255659433,
117.391920741173));
#38162=CARTESIAN_POINT('Ctrl Pts',(-6.45510045951788,-2.03075529238065,
117.400010944593));
#38163=CARTESIAN_POINT('Ctrl Pts',(-6.40335638943706,-2.19523260375799,
117.408098914324));
#38164=CARTESIAN_POINT('Ctrl Pts',(-6.34530011202132,-2.35779987388169,
117.416186884055));
#38165=CARTESIAN_POINT('Ctrl Pts',(-6.28110532062709,-2.51793664558703,
117.424274853786));
#38166=CARTESIAN_POINT('Ctrl Pts',(-6.21691802384008,-2.67805472166022,
117.432361879263));
#38167=CARTESIAN_POINT('Ctrl Pts',(-6.14659377637887,-2.83574252080221,
117.44044890474));
#38168=CARTESIAN_POINT('Ctrl Pts',(-6.07035494762533,-2.99049825444535,
117.448535930218));
#38169=CARTESIAN_POINT('Ctrl Pts',(-5.99411020078692,-3.14526600109525,
117.456623583455));
#38170=CARTESIAN_POINT('Ctrl Pts',(-5.91195012196213,-3.29710089746528,
117.464711236693));
#38171=CARTESIAN_POINT('Ctrl Pts',(-5.82414364746011,-3.44552460065954,
117.472798889931));
#38172=CARTESIAN_POINT('Ctrl Pts',(-5.73631328792009,-3.59398867793568,
117.480888743164));
#38173=CARTESIAN_POINT('Ctrl Pts',(-5.64283366346503,-3.73903939694189,
117.488978596398));
#38174=CARTESIAN_POINT('Ctrl Pts',(-5.54401768793729,-3.88022639492059,
117.497068449632));
#38175=CARTESIAN_POINT('Ctrl Pts',(-5.4451020877245,-4.02155573537107,117.505166458926));
#38176=CARTESIAN_POINT('Ctrl Pts',(-5.34083960372453,-4.15901327203359,
117.51326446822));
#38177=CARTESIAN_POINT('Ctrl Pts',(-5.23158467127832,-4.29218019510431,
117.521362477515));
#38178=CARTESIAN_POINT('Ctrl Pts',(-5.1222704713336,-4.4254193572057,117.529464879734));
#38179=CARTESIAN_POINT('Ctrl Pts',(-5.00795867227044,-4.55436299281459,
117.537567281954));
#38180=CARTESIAN_POINT('Ctrl Pts',(-4.88904112237404,-4.67862863494589,
117.545669684173));
#38181=CARTESIAN_POINT('Ctrl Pts',(-4.76995697730049,-4.80306836455782,
117.553783437292));
#38182=CARTESIAN_POINT('Ctrl Pts',(-4.64625445853697,-4.92281675420357,
117.561897190411));
#38183=CARTESIAN_POINT('Ctrl Pts',(-4.51835980497909,-5.03753051333184,
117.57001094353));
#38184=CARTESIAN_POINT('Ctrl Pts',(-4.42824635666586,-5.11835681933018,
117.575727822633));
#38185=CARTESIAN_POINT('Ctrl Pts',(-4.33605242085457,-5.19668454010475,
117.581444701736));
#38186=CARTESIAN_POINT('Ctrl Pts',(-4.24193560225691,-5.27240659910684,
117.587161580839));
#38187=CARTESIAN_POINT('Ctrl Pts',(-4.10650788809726,-5.38136550267915,
117.595387781858));
#38188=CARTESIAN_POINT('Ctrl Pts',(-3.96669008959762,-5.48525542608483,
117.603613982876));
#38189=CARTESIAN_POINT('Ctrl Pts',(-3.82289739792679,-5.58370347394313,
117.611840183895));
#38190=CARTESIAN_POINT('Ctrl Pts',(-3.67926622703936,-5.68204093616854,
117.620057144511));
#38191=CARTESIAN_POINT('Ctrl Pts',(-3.53166934715663,-5.77494849432802,
117.628274105127));
#38192=CARTESIAN_POINT('Ctrl Pts',(-3.38055564291473,-5.86209284685576,
117.636491065743));
#38193=CARTESIAN_POINT('Ctrl Pts',(-3.22958135334985,-5.94915680163384,
117.644700445544));
#38194=CARTESIAN_POINT('Ctrl Pts',(-3.07509700980742,-6.03046796179911,
117.652909825346));
#38195=CARTESIAN_POINT('Ctrl Pts',(-2.917581228281,-6.10573572768936,117.661119205147));
#38196=CARTESIAN_POINT('Ctrl Pts',(-2.760179163344,-6.18094915493782,117.669322658288));
#38197=CARTESIAN_POINT('Ctrl Pts',(-2.59975034183862,-6.25012772416892,
117.677526111428));
#38198=CARTESIAN_POINT('Ctrl Pts',(-2.43679886133955,-6.31302624019371,
117.685729564568));
#38199=CARTESIAN_POINT('Ctrl Pts',(-2.27393233400521,-6.37589196469076,
117.693928740918));
#38200=CARTESIAN_POINT('Ctrl Pts',(-2.10854610149869,-6.4324840296236,117.702127917269));
#38201=CARTESIAN_POINT('Ctrl Pts',(-1.94116524725917,-6.48260491491139,
117.710327093619));
#38202=CARTESIAN_POINT('Ctrl Pts',(-1.77381588825272,-6.53271636919841,
117.71852472717));
#38203=CARTESIAN_POINT('Ctrl Pts',(-1.60447299653246,-6.57635896053857,
117.726722360721));
#38204=CARTESIAN_POINT('Ctrl Pts',(-1.43367816021121,-6.61338460494575,
117.734919994273));
#38205=CARTESIAN_POINT('Ctrl Pts',(-1.26289562530995,-6.65040758259782,
117.743117037393));
#38206=CARTESIAN_POINT('Ctrl Pts',(-1.09066170442501,-6.68081448560249,
117.751314080514));
#38207=CARTESIAN_POINT('Ctrl Pts',(-0.917529506141373,-6.70450808078863,
117.759511123635));
#38208=CARTESIAN_POINT('Ctrl Pts',(-0.744378311137273,-6.72820427572575,
117.767709066166));
#38209=CARTESIAN_POINT('Ctrl Pts',(-0.570328997811365,-6.74518564666166,
117.775907008697));
#38210=CARTESIAN_POINT('Ctrl Pts',(-0.395941200302829,-6.75540669137712,
117.784104951228));
#38211=CARTESIAN_POINT('Ctrl Pts',(-0.221502573495327,-6.76563071524907,
117.792305283237));
#38212=CARTESIAN_POINT('Ctrl Pts',(-0.0467256239640609,-6.76909046701836,
117.800505615245));
#38213=CARTESIAN_POINT('Ctrl Pts',(0.127828546347631,-6.76579255244636,
117.808705947253));
#38214=CARTESIAN_POINT('Ctrl Pts',(0.302564649283056,-6.76249120055602,
117.816914826224));
#38215=CARTESIAN_POINT('Ctrl Pts',(0.477077150016872,-6.75241811763111,
117.825123705195));
#38216=CARTESIAN_POINT('Ctrl Pts',(0.650807598446602,-6.73563200225518,
117.833332584166));
#38217=CARTESIAN_POINT('Ctrl Pts',(0.824631309410862,-6.71883687570316,
117.841545869853));
#38218=CARTESIAN_POINT('Ctrl Pts',(0.99767177606956,-6.69532158082911,117.84975915554));
#38219=CARTESIAN_POINT('Ctrl Pts',(1.1693793964943,-6.66519623319934,117.857972441228));
#38220=CARTESIAN_POINT('Ctrl Pts',(1.34133820400521,-6.63502681589886,117.86619774194));
#38221=CARTESIAN_POINT('Ctrl Pts',(1.51195991815939,-6.5982280972073,117.874423042652));
#38222=CARTESIAN_POINT('Ctrl Pts',(1.68070753585745,-6.55496080681738,117.882648343364));
#38223=CARTESIAN_POINT('Ctrl Pts',(1.83331940040885,-6.51583076189842,117.890087135658));
#38224=CARTESIAN_POINT('Ctrl Pts',(1.98439845459551,-6.47141076516683,117.897525927952));
#38225=CARTESIAN_POINT('Ctrl Pts',(2.13356148950366,-6.42185365533247,117.904964720246));
#38226=CARTESIAN_POINT('Ctrl Pts',(2.29703695419795,-6.36754146220723,117.913117276459));
#38227=CARTESIAN_POINT('Ctrl Pts',(2.45869289501725,-6.30689806659958,117.921269832673));
#38228=CARTESIAN_POINT('Ctrl Pts',(2.61799751028861,-6.24006234232661,117.929422388886));
#38229=CARTESIAN_POINT('Ctrl Pts',(2.77711756732243,-6.17330404885158,117.937565500166));
#38230=CARTESIAN_POINT('Ctrl Pts',(2.93389138767401,-6.10036784715035,117.945708611447));
#38231=CARTESIAN_POINT('Ctrl Pts',(3.08780156878072,-6.02144255738069,117.953851722727));
#38232=CARTESIAN_POINT('Ctrl Pts',(3.24156579893055,-5.94259211140292,117.961987112004));
#38233=CARTESIAN_POINT('Ctrl Pts',(3.39247147310079,-5.85776404991919,117.970122501282));
#38234=CARTESIAN_POINT('Ctrl Pts',(3.54002045463034,-5.76719552129099,117.978257890559));
#38235=CARTESIAN_POINT('Ctrl Pts',(3.68746052104472,-5.67669384694822,117.986387274597));
#38236=CARTESIAN_POINT('Ctrl Pts',(3.83154851828465,-5.58046033329277,117.994516658636));
#38237=CARTESIAN_POINT('Ctrl Pts',(3.97181025635086,-5.47877835722035,118.002646042675));
#38238=CARTESIAN_POINT('Ctrl Pts',(4.11199792014433,-5.37715008088481,118.010771133467));
#38239=CARTESIAN_POINT('Ctrl Pts',(4.24836305376973,-5.27007928670352,118.018896224259));
#38240=CARTESIAN_POINT('Ctrl Pts',(4.38045986071102,-5.15789302028451,118.027021315051));
#38241=CARTESIAN_POINT('Ctrl Pts',(4.51306090980176,-5.04527851456564,118.035177421076));
#38242=CARTESIAN_POINT('Ctrl Pts',(4.64136066852364,-4.92750960717487,118.043333527101));
#38243=CARTESIAN_POINT('Ctrl Pts',(4.76494082448019,-4.80495868236159,118.051489633126));
#38244=CARTESIAN_POINT('Ctrl Pts',(4.88802359265873,-4.68290100285711,118.0596129123));
#38245=CARTESIAN_POINT('Ctrl Pts',(5.00642443226679,-4.55610000262943,118.067736191473));
#38246=CARTESIAN_POINT('Ctrl Pts',(5.11976644642777,-4.42496107712061,118.075859470647));
#38247=CARTESIAN_POINT('Ctrl Pts',(5.23312355303523,-4.29380468935626,118.083983831503));
#38248=CARTESIAN_POINT('Ctrl Pts',(5.34142025322042,-4.15830950258001,118.09210819236));
#38249=CARTESIAN_POINT('Ctrl Pts',(5.4443195577944,-4.0189144744094,118.100232553217));
#38250=CARTESIAN_POINT('Ctrl Pts',(5.54725214140282,-3.87947436399103,118.108359541602));
#38251=CARTESIAN_POINT('Ctrl Pts',(5.64478363622508,-3.73613219477519,118.116486529987));
#38252=CARTESIAN_POINT('Ctrl Pts',(5.73662007644422,-3.58935636271145,118.124613518373));
#38253=CARTESIAN_POINT('Ctrl Pts',(5.82905022879375,-3.44163164160391,118.132793046813));
#38254=CARTESIAN_POINT('Ctrl Pts',(5.91571123614408,-3.29042902584766,118.140972575253));
#38255=CARTESIAN_POINT('Ctrl Pts',(5.99635052252058,-3.13625085270092,118.149152103693));
#38256=CARTESIAN_POINT('Ctrl Pts',(6.07661005250048,-2.98279875427651,118.157293112097));
#38257=CARTESIAN_POINT('Ctrl Pts',(6.15090435722253,-2.82639942147593,118.165434120501));
#38258=CARTESIAN_POINT('Ctrl Pts',(6.21903309158284,-2.66756750726155,118.173575128904));
#38259=CARTESIAN_POINT('Ctrl Pts',(6.28764536333751,-2.50760829821833,118.181773917362));
#38260=CARTESIAN_POINT('Ctrl Pts',(6.35000408858973,-2.34518220323418,118.189972705821));
#38261=CARTESIAN_POINT('Ctrl Pts',(6.40595601871127,-2.18082931160071,118.198171494279));
#38262=CARTESIAN_POINT('Ctrl Pts',(6.46190794883286,-2.01647641996712,118.206370282737));
#38263=CARTESIAN_POINT('Ctrl Pts',(6.5114530398635,-1.85019710608718,118.214569071196));
#38264=CARTESIAN_POINT('Ctrl Pts',(6.55449059770862,-1.68254034262164,118.222767859654));
#38265=CARTESIAN_POINT('Ctrl Pts',(6.59770800392675,-1.51418296328373,118.231000909786));
#38266=CARTESIAN_POINT('Ctrl Pts',(6.63449783408622,-1.34391328261386,118.239233959918));
#38267=CARTESIAN_POINT('Ctrl Pts',(6.66468970190499,-1.17226284480979,118.24746701005));
#38268=CARTESIAN_POINT('Ctrl Pts',(6.69484561585011,-1.00081681629202,118.255690255885));
#38269=CARTESIAN_POINT('Ctrl Pts',(6.71841915156091,-0.827993654093565,
118.26391350172));
#38270=CARTESIAN_POINT('Ctrl Pts',(6.7352898103742,-0.654339491601587,118.272136747554));
#38271=CARTESIAN_POINT('Ctrl Pts',(6.75214375552496,-0.480857367267884,
118.280351846668));
#38272=CARTESIAN_POINT('Ctrl Pts',(6.76230801402065,-0.306546236240227,
118.288566945781));
#38273=CARTESIAN_POINT('Ctrl Pts',(6.76571319567667,-0.13196194090165,118.296782044895));
#38274=CARTESIAN_POINT('Ctrl Pts',(6.76911568514746,0.0424843256004356,
118.304990649034));
#38275=CARTESIAN_POINT('Ctrl Pts',(6.76576973465029,0.217202969746779,118.313199253173));
#38276=CARTESIAN_POINT('Ctrl Pts',(6.75565779671617,0.391633417455661,118.321407857312));
#38277=CARTESIAN_POINT('Ctrl Pts',(6.74555183075505,0.565960848914752,118.329611613561));
#38278=CARTESIAN_POINT('Ctrl Pts',(6.72868785840712,0.740000066384756,118.337815369809));
#38279=CARTESIAN_POINT('Ctrl Pts',(6.70510041546822,0.913190789751989,118.346019126058));
#38280=CARTESIAN_POINT('Ctrl Pts',(6.68151995145901,1.08633027035064,118.354220455023));
#38281=CARTESIAN_POINT('Ctrl Pts',(6.65122002393255,1.25862140194925,118.362421783987));
#38282=CARTESIAN_POINT('Ctrl Pts',(6.61428702359496,1.42950906590458,118.370623112951));
#38283=CARTESIAN_POINT('Ctrl Pts',(6.57735911667073,1.60037316281947,118.378823310874));
#38284=CARTESIAN_POINT('Ctrl Pts',(6.53380003370326,1.76983382733277,118.387023508797));
#38285=CARTESIAN_POINT('Ctrl Pts',(6.48374728705282,1.93734615328164,118.395223706719));
#38286=CARTESIAN_POINT('Ctrl Pts',(6.43369237257765,2.10486573432414,118.403424259799));
#38287=CARTESIAN_POINT('Ctrl Pts',(6.37714333663196,2.27043646536461,118.411624812879));
#38288=CARTESIAN_POINT('Ctrl Pts',(6.31428758543787,2.43352856740683,118.419825365959));
#38289=CARTESIAN_POINT('Ctrl Pts',(6.25141772121773,2.59665728858164,118.428027760312));
#38290=CARTESIAN_POINT('Ctrl Pts',(6.18223845019751,2.757305938066,118.436230154665));
#38291=CARTESIAN_POINT('Ctrl Pts',(6.10698536066305,2.9149646318004,118.444432549019));
#38292=CARTESIAN_POINT('Ctrl Pts',(6.03166189626131,3.07277076412789,118.452642614053));
#38293=CARTESIAN_POINT('Ctrl Pts',(5.95025341953817,3.22758103050455,118.460852679086));
#38294=CARTESIAN_POINT('Ctrl Pts',(5.86304198135088,3.37890925076675,118.46906274412));
#38295=CARTESIAN_POINT('Ctrl Pts',(5.77578880531617,3.53030989403104,118.477276738346));
#38296=CARTESIAN_POINT('Ctrl Pts',(5.68272732123574,3.67822486547193,118.485490732571));
#38297=CARTESIAN_POINT('Ctrl Pts',(5.58418294253159,3.82219699444433,118.493704726796));
#38298=CARTESIAN_POINT('Ctrl Pts',(5.48550421501832,3.96636540537952,118.501929919431));
#38299=CARTESIAN_POINT('Ctrl Pts',(5.38132786770703,4.10657994334918,118.510155112067));
#38300=CARTESIAN_POINT('Ctrl Pts',(5.27202038230147,4.24241559593092,118.518380304702));
#38301=CARTESIAN_POINT('Ctrl Pts',(5.1737203947933,4.36457230736204,118.525777202822));
#38302=CARTESIAN_POINT('Ctrl Pts',(5.07127131958762,4.48318797613906,118.533174100942));
#38303=CARTESIAN_POINT('Ctrl Pts',(4.96496457235056,4.59797953402403,118.540570999062));
#38304=CARTESIAN_POINT('Ctrl Pts',(4.84067184494065,4.73219261253483,118.549219374312));
#38305=CARTESIAN_POINT('Ctrl Pts',(4.71082313055442,4.86148250034786,118.557867749561));
#38306=CARTESIAN_POINT('Ctrl Pts',(4.5758248450852,4.98539025424299,118.566516124811));
#38307=CARTESIAN_POINT('Ctrl Pts',(4.44106290500398,5.1090810792633,118.575149359102));
#38308=CARTESIAN_POINT('Ctrl Pts',(4.30116960500453,5.2274083646177,118.583782593392));
#38309=CARTESIAN_POINT('Ctrl Pts',(4.15658856369466,5.33994948591864,118.592415827682));
#38310=CARTESIAN_POINT('Ctrl Pts',(4.01216266249406,5.45236984697538,118.601039798234));
#38311=CARTESIAN_POINT('Ctrl Pts',(3.86305928735499,5.55901623499744,118.609663768786));
#38312=CARTESIAN_POINT('Ctrl Pts',(3.70975685993916,5.65950466384951,118.618287739338));
#38313=CARTESIAN_POINT('Ctrl Pts',(3.55665871294202,5.75985918863584,118.626900218172));
#38314=CARTESIAN_POINT('Ctrl Pts',(3.39937293016326,5.85407195712336,118.635512697005));
#38315=CARTESIAN_POINT('Ctrl Pts',(3.23840883319496,5.94180084057728,118.644125175839));
#38316=CARTESIAN_POINT('Ctrl Pts',(3.1922953569385,5.96693367367704,118.646592504552));
#38317=CARTESIAN_POINT('Ctrl Pts',(3.14588018611451,5.99153462166168,118.649059833265));
#38318=CARTESIAN_POINT('Ctrl Pts',(3.09917575053251,6.01559628526643,118.651527161978));
#38319=CARTESIAN_POINT('Origin',(0.,0.,-3.69717978381041));
#38320=CARTESIAN_POINT('',(3.09917575053254,6.01559628526642,121.045781922714));
#38321=CARTESIAN_POINT('',(3.09917575053273,6.01559628526632,120.651392015122));
#38322=CARTESIAN_POINT('',(3.09917575053259,6.01559628526639,-3.69717978381041));
#38323=CARTESIAN_POINT('',(-6.76699734236938,0.00599736322975646,119.69717978384));
#38324=CARTESIAN_POINT('Ctrl Pts',(-6.76699734236938,0.00599736322994578,
119.69717978384));
#38325=CARTESIAN_POINT('Ctrl Pts',(-6.76714983230376,-0.166061413446056,
119.705282912405));
#38326=CARTESIAN_POINT('Ctrl Pts',(-6.76073597240442,-0.338315227567415,
119.713386040971));
#38327=CARTESIAN_POINT('Ctrl Pts',(-6.74773798144884,-0.510216751697474,
119.721489169537));
#38328=CARTESIAN_POINT('Ctrl Pts',(-6.73474953927967,-0.681991990854606,
119.729586345257));
#38329=CARTESIAN_POINT('Ctrl Pts',(-6.71518662383408,-0.853415088825623,
119.737683520976));
#38330=CARTESIAN_POINT('Ctrl Pts',(-6.6890835203219,-1.02393879609966,119.745780696695));
#38331=CARTESIAN_POINT('Ctrl Pts',(-6.66175525810802,-1.20246609588577,
119.754257916316));
#38332=CARTESIAN_POINT('Ctrl Pts',(-6.6272580405859,-1.38000712446736,119.762735135937));
#38333=CARTESIAN_POINT('Ctrl Pts',(-6.58569224159668,-1.55593916943217,
119.771212355557));
#38334=CARTESIAN_POINT('Ctrl Pts',(-6.54601773545304,-1.72386609898865,
119.779303851693));
#38335=CARTESIAN_POINT('Ctrl Pts',(-6.4999037588229,-1.89032682745913,119.78739534783));
#38336=CARTESIAN_POINT('Ctrl Pts',(-6.44748993765559,-2.05479013620123,
119.795486843966));
#38337=CARTESIAN_POINT('Ctrl Pts',(-6.39507803907303,-2.21924741228552,
119.803578043299));
#38338=CARTESIAN_POINT('Ctrl Pts',(-6.33636686756971,-2.38170706249172,
119.811669242632));
#38339=CARTESIAN_POINT('Ctrl Pts',(-6.27154580749815,-2.54165343515838,
119.819760441965));
#38340=CARTESIAN_POINT('Ctrl Pts',(-6.20671455163083,-2.70162496601509,
119.827852913974));
#38341=CARTESIAN_POINT('Ctrl Pts',(-6.1357716327652,-2.85908209014954,119.835945385983));
#38342=CARTESIAN_POINT('Ctrl Pts',(-6.05895438609993,-3.01352961610807,
119.844037857993));
#38343=CARTESIAN_POINT('Ctrl Pts',(-5.98211015451093,-3.1680313975221,119.852133172784));
#38344=CARTESIAN_POINT('Ctrl Pts',(-5.89938765153777,-3.31952114582841,
119.860228487576));
#38345=CARTESIAN_POINT('Ctrl Pts',(-5.81106986251145,-3.46752881069663,
119.868323802368));
#38346=CARTESIAN_POINT('Ctrl Pts',(-5.72265967848526,-3.61569131603728,
119.876427586197));
#38347=CARTESIAN_POINT('Ctrl Pts',(-5.62864271045665,-3.76036414767746,
119.884531370026));
#38348=CARTESIAN_POINT('Ctrl Pts',(-5.52934532477899,-3.90110616099393,
119.892635153854));
#38349=CARTESIAN_POINT('Ctrl Pts',(-5.42998710218725,-4.04193440326508,
119.90074390266));
#38350=CARTESIAN_POINT('Ctrl Pts',(-5.32534224098506,-4.17882673761837,
119.908852651465));
#38351=CARTESIAN_POINT('Ctrl Pts',(-5.21577671797108,-4.31137590894959,
119.91696140027));
#38352=CARTESIAN_POINT('Ctrl Pts',(-5.1060677038644,-4.44409867161598,119.925080768596));
#38353=CARTESIAN_POINT('Ctrl Pts',(-4.99142540805335,-4.57246664243129,
119.933200136921));
#38354=CARTESIAN_POINT('Ctrl Pts',(-4.87225238205238,-4.69610963730458,
119.941319505246));
#38355=CARTESIAN_POINT('Ctrl Pts',(-4.83353055095133,-4.73628385562368,
119.943957659361));
#38356=CARTESIAN_POINT('Ctrl Pts',(-4.79433065211497,-4.77595955988454,
119.946595813475));
#38357=CARTESIAN_POINT('Ctrl Pts',(-4.75466721334804,-4.81512499217966,
119.94923396759));
#38358=CARTESIAN_POINT('Ctrl Pts',(-4.63212092974246,-4.93613260833156,
119.957384949765));
#38359=CARTESIAN_POINT('Ctrl Pts',(-4.50475960522731,-5.05264900334892,
119.965535931939));
#38360=CARTESIAN_POINT('Ctrl Pts',(-4.37294796614193,-5.16426326647036,
119.973686914113));
#38361=CARTESIAN_POINT('Ctrl Pts',(-4.24128943849203,-5.27574787928046,
119.981828428166));
#38362=CARTESIAN_POINT('Ctrl Pts',(-4.10519116268699,-5.38234146119476,
119.989969942219));
#38363=CARTESIAN_POINT('Ctrl Pts',(-3.96505585930834,-5.48366857428169,
119.998111456272));
#38364=CARTESIAN_POINT('Ctrl Pts',(-3.82505384646506,-5.5848993094765,120.006245226475));
#38365=CARTESIAN_POINT('Ctrl Pts',(-3.6810227449162,-5.68087333568657,120.014378996678));
#38366=CARTESIAN_POINT('Ctrl Pts',(-3.53339961980484,-5.77125429406494,
120.022512766881));
#38367=CARTESIAN_POINT('Ctrl Pts',(-3.38588585913341,-5.86156829502803,
120.030640511299));
#38368=CARTESIAN_POINT('Ctrl Pts',(-3.2347856841373,-5.94629728845039,120.038768255717));
#38369=CARTESIAN_POINT('Ctrl Pts',(-3.08056650962285,-6.02514721644128,
120.046896000135));
#38370=CARTESIAN_POINT('Ctrl Pts',(-2.92642916271588,-6.1039553072159,120.055019432029));
#38371=CARTESIAN_POINT('Ctrl Pts',(-2.76917643698794,-6.17689037877921,
120.063142863923));
#38372=CARTESIAN_POINT('Ctrl Pts',(-2.60930179761763,-6.24370347862144,
120.071266295817));
#38373=CARTESIAN_POINT('Ctrl Pts',(-2.44841297641819,-6.31094041448966,
120.079441259568));
#38374=CARTESIAN_POINT('Ctrl Pts',(-2.28486918504337,-6.37197724877038,
120.087616223319));
#38375=CARTESIAN_POINT('Ctrl Pts',(-2.11919581083928,-6.42660860137921,
120.09579118707));
#38376=CARTESIAN_POINT('Ctrl Pts',(-1.95460412294866,-6.48088326428647,
120.103912776243));
#38377=CARTESIAN_POINT('Ctrl Pts',(-1.78791093746152,-6.52883574899776,
120.112034365416));
#38378=CARTESIAN_POINT('Ctrl Pts',(-1.61964834893434,-6.57031416492349,
120.120155954589));
#38379=CARTESIAN_POINT('Ctrl Pts',(-1.45136354629416,-6.61179805685092,
120.128278615978));
#38380=CARTESIAN_POINT('Ctrl Pts',(-1.28150928330525,-6.64680608995604,
120.136401277368));
#38381=CARTESIAN_POINT('Ctrl Pts',(-1.11062945811912,-6.67523716483228,
120.144523938757));
#38382=CARTESIAN_POINT('Ctrl Pts',(-0.93969453271823,-6.70367740731112,
120.152649219299));
#38383=CARTESIAN_POINT('Ctrl Pts',(-0.767733747445996,-6.72553640847876,
120.160774499841));
#38384=CARTESIAN_POINT('Ctrl Pts',(-0.595297713324265,-6.74076476614567,
120.168899780384));
#38385=CARTESIAN_POINT('Ctrl Pts',(-0.420983024390873,-6.75615903360951,
120.177113584172));
#38386=CARTESIAN_POINT('Ctrl Pts',(-0.246183053081737,-6.76477729835143,
120.185327387959));
#38387=CARTESIAN_POINT('Ctrl Pts',(-0.071467321751315,-6.76662260081953,
120.193541191747));
#38388=CARTESIAN_POINT('Ctrl Pts',(0.101664509346737,-6.76845117454211,
120.201680532602));
#38389=CARTESIAN_POINT('Ctrl Pts',(0.274713258622926,-6.76362915725161,
120.209819873457));
#38390=CARTESIAN_POINT('Ctrl Pts',(0.447129601000251,-6.75221179465732,
120.217959214313));
#38391=CARTESIAN_POINT('Ctrl Pts',(0.621911975230568,-6.74063775408689,
120.226210249567));
#38392=CARTESIAN_POINT('Ctrl Pts',(0.79604406955542,-6.7222860837576,120.234461284821));
#38393=CARTESIAN_POINT('Ctrl Pts',(0.968964403150727,-6.69726787469538,
120.242712320075));
#38394=CARTESIAN_POINT('Ctrl Pts',(1.14188473674603,-6.67224966563316,120.250963355329));
#38395=CARTESIAN_POINT('Ctrl Pts',(1.3135929442763,-6.64056505344879,120.259214390583));
#38396=CARTESIAN_POINT('Ctrl Pts',(1.48354396519664,-6.60237732209608,120.267465425837));
#38397=CARTESIAN_POINT('Ctrl Pts',(1.65309821112369,-6.56427874547025,120.275697197868));
#38398=CARTESIAN_POINT('Ctrl Pts',(1.82143282316018,-6.51958861638674,120.283928969899));
#38399=CARTESIAN_POINT('Ctrl Pts',(1.98799707482147,-6.46839675889639,120.29216074193));
#38400=CARTESIAN_POINT('Ctrl Pts',(2.15436243212074,-6.41726602959972,120.300382684402));
#38401=CARTESIAN_POINT('Ctrl Pts',(2.31896129935446,-6.35964913546916,120.308604626875));
#38402=CARTESIAN_POINT('Ctrl Pts',(2.48125262780259,-6.29568696783939,120.316826569347));
#38403=CARTESIAN_POINT('Ctrl Pts',(2.64338268068096,-6.231788362047,120.325040341337));
#38404=CARTESIAN_POINT('Ctrl Pts',(2.80320943040884,-6.16155717072647,120.333254113327));
#38405=CARTESIAN_POINT('Ctrl Pts',(2.96020640973506,-6.08518422167838,120.341467885317));
#38406=CARTESIAN_POINT('Ctrl Pts',(3.11707881900236,-6.00887187113863,120.349675140047));
#38407=CARTESIAN_POINT('Ctrl Pts',(3.27112560925306,-5.9264276252834,120.357882394778));
#38408=CARTESIAN_POINT('Ctrl Pts',(3.42183966365579,-5.83809063960402,120.366089649508));
#38409=CARTESIAN_POINT('Ctrl Pts',(3.57246431127022,-5.74980605730671,120.37429203552));
#38410=CARTESIAN_POINT('Ctrl Pts',(3.71975985325519,-5.65563587973298,120.382494421532));
#38411=CARTESIAN_POINT('Ctrl Pts',(3.86324311071821,-5.55586551920475,120.390696807544));
#38412=CARTESIAN_POINT('Ctrl Pts',(4.00668354190892,-5.45612493770931,120.398896745343));
#38413=CARTESIAN_POINT('Ctrl Pts',(4.14631365914936,-5.35078770397324,120.407096683141));
#38414=CARTESIAN_POINT('Ctrl Pts',(4.28167845510226,-5.24018306999986,120.41529662094));
#38415=CARTESIAN_POINT('Ctrl Pts',(4.41702432356284,-5.12959390140908,120.423495412176));
#38416=CARTESIAN_POINT('Ctrl Pts',(4.54810578057691,-5.01373902552941,120.431694203412));
#38417=CARTESIAN_POINT('Ctrl Pts',(4.67450015677126,-4.89298858412172,120.439892994648));
#38418=CARTESIAN_POINT('Ctrl Pts',(4.80089978836559,-4.77223312198537,120.448092126784));
#38419=CARTESIAN_POINT('Ctrl Pts',(4.92261169164524,-4.64658193634217,120.45629125892));
#38420=CARTESIAN_POINT('Ctrl Pts',(5.03924935587985,-4.51644272954552,120.464490391057));
#38421=CARTESIAN_POINT('Ctrl Pts',(5.15591302843692,-4.38627450379964,120.472691351468));
#38422=CARTESIAN_POINT('Ctrl Pts',(5.26749996920537,-4.25161653054213,120.480892311879));
#38423=CARTESIAN_POINT('Ctrl Pts',(5.37366329560932,-4.11291037896782,120.48909327229));
#38424=CARTESIAN_POINT('Ctrl Pts',(5.47992612260608,-3.97407422633969,120.497301918975));
#38425=CARTESIAN_POINT('Ctrl Pts',(5.58075496111583,-3.83118259998144,120.50551056566));
#38426=CARTESIAN_POINT('Ctrl Pts',(5.67584516562826,-3.68470767576131,120.513719212345));
#38427=CARTESIAN_POINT('Ctrl Pts',(5.77098076887493,-3.53816282029861,120.521931778069));
#38428=CARTESIAN_POINT('Ctrl Pts',(5.86037209218311,-3.388031563803,120.530144343792));
#38429=CARTESIAN_POINT('Ctrl Pts',(5.94376004726729,-3.23481150927055,120.538356909516));
#38430=CARTESIAN_POINT('Ctrl Pts',(6.0272624226589,-3.08138121471329,120.546580744064));
#38431=CARTESIAN_POINT('Ctrl Pts',(6.10474480772534,-2.92485397305057,120.554804578613));
#38432=CARTESIAN_POINT('Ctrl Pts',(6.17599542743257,-2.7657493524056,120.563028413162));
#38433=CARTESIAN_POINT('Ctrl Pts',(6.24146134407012,-2.6195621350229,120.570584570136));
#38434=CARTESIAN_POINT('Ctrl Pts',(6.30166679179529,-2.47119947808256,120.57814072711));
#38435=CARTESIAN_POINT('Ctrl Pts',(6.35648468855408,-2.32107548437736,120.585696884084));
#38436=CARTESIAN_POINT('Ctrl Pts',(6.41920705936011,-2.1493043410682,120.594342602137));
#38437=CARTESIAN_POINT('Ctrl Pts',(6.47501881650106,-1.97483567765751,120.602988320189));
#38438=CARTESIAN_POINT('Ctrl Pts',(6.52369697497116,-1.79823991134447,120.611634038242));
#38439=CARTESIAN_POINT('Ctrl Pts',(6.57231264060621,-1.62187085800584,120.620268656954));
#38440=CARTESIAN_POINT('Ctrl Pts',(6.6138128886129,-1.44338043966331,120.628903275666));
#38441=CARTESIAN_POINT('Ctrl Pts',(6.64802372784018,-1.26335644775096,120.637537894379));
#38442=CARTESIAN_POINT('Ctrl Pts',(6.68344276101051,-1.07697470778149,120.646477454281));
#38443=CARTESIAN_POINT('Ctrl Pts',(6.71104798408059,-0.888949389233346,
120.655417014183));
#38444=CARTESIAN_POINT('Ctrl Pts',(6.73070270760108,-0.69995004242549,120.664356574086));
#38445=CARTESIAN_POINT('Ctrl Pts',(6.74963428938018,-0.517904409142569,
120.672967227356));
#38446=CARTESIAN_POINT('Ctrl Pts',(6.76118988786407,-0.334955483724732,
120.681577880627));
#38447=CARTESIAN_POINT('Ctrl Pts',(6.76529912985488,-0.151712503060123,
120.690188533897));
#38448=CARTESIAN_POINT('Ctrl Pts',(6.76940448217319,0.0313570258617701,
120.698791036608));
#38449=CARTESIAN_POINT('Ctrl Pts',(6.76607752394736,0.214719751179746,120.707393539319));
#38450=CARTESIAN_POINT('Ctrl Pts',(6.75529972530593,0.397762015885989,120.71599604203));
#38451=CARTESIAN_POINT('Ctrl Pts',(6.7445340568598,0.580598270209753,120.724588862798));
#38452=CARTESIAN_POINT('Ctrl Pts',(6.72633429525022,0.763114479634569,120.733181683565));
#38453=CARTESIAN_POINT('Ctrl Pts',(6.70073396604544,0.944697473419382,120.741774504333));
#38454=CARTESIAN_POINT('Ctrl Pts',(6.69771685096488,0.966097854037087,120.742787207291));
#38455=CARTESIAN_POINT('Ctrl Pts',(6.69459700377117,0.987485273873215,120.74379991025));
#38456=CARTESIAN_POINT('Ctrl Pts',(6.69137452704879,1.00885873082541,120.744812613208));
#38457=CARTESIAN_POINT('Ctrl Pts',(6.66402394233424,1.19026470994503,120.753407870968));
#38458=CARTESIAN_POINT('Ctrl Pts',(6.6293082112977,1.37045092087214,120.762003128728));
#38459=CARTESIAN_POINT('Ctrl Pts',(6.58737030967475,1.54881935783862,120.770598386488));
#38460=CARTESIAN_POINT('Ctrl Pts',(6.54539313498565,1.72735482928111,120.779201693343));
#38461=CARTESIAN_POINT('Ctrl Pts',(6.49618035987755,1.90406883172741,120.787805000197));
#38462=CARTESIAN_POINT('Ctrl Pts',(6.43992496467969,2.07837808141235,120.796408307052));
#38463=CARTESIAN_POINT('Ctrl Pts',(6.38133720128924,2.25991425303447,120.805368309992));
#38464=CARTESIAN_POINT('Ctrl Pts',(6.31511052490924,2.43884166052911,120.814328312932));
#38465=CARTESIAN_POINT('Ctrl Pts',(6.24151798084411,2.61452525227807,120.823288315872));
#38466=CARTESIAN_POINT('Ctrl Pts',(6.17066182790065,2.7836764020957,120.831915159076));
#38467=CARTESIAN_POINT('Ctrl Pts',(6.0929778672566,2.94982036745001,120.840542002281));
#38468=CARTESIAN_POINT('Ctrl Pts',(6.00875667309165,3.11241582112297,120.849168845486));
#38469=CARTESIAN_POINT('Ctrl Pts',(5.92445498475476,3.27516667494829,120.857803933772));
#38470=CARTESIAN_POINT('Ctrl Pts',(5.83360373987583,3.43436198114582,120.866439022058));
#38471=CARTESIAN_POINT('Ctrl Pts',(5.73653783237106,3.5894878043776,120.875074110344));
#38472=CARTESIAN_POINT('Ctrl Pts',(5.63932776251445,3.74484402058756,120.883722023469));
#38473=CARTESIAN_POINT('Ctrl Pts',(5.53588475378216,3.89611842165814,120.892369936595));
#38474=CARTESIAN_POINT('Ctrl Pts',(5.426585965883,4.04282744559815,120.90101784972));
#38475=CARTESIAN_POINT('Ctrl Pts',(5.41432430575596,4.05928596470618,120.901988013924));
#38476=CARTESIAN_POINT('Ctrl Pts',(5.4019889884601,4.07568706251909,120.902958178127));
#38477=CARTESIAN_POINT('Ctrl Pts',(5.38958057669206,4.09203008387569,120.903928342331));
#38478=CARTESIAN_POINT('Ctrl Pts',(5.28437976957529,4.23058923790611,120.912153573666));
#38479=CARTESIAN_POINT('Ctrl Pts',(5.17369361909269,4.36527153031135,120.920378805));
#38480=CARTESIAN_POINT('Ctrl Pts',(5.05783804477281,4.4956160103871,120.928604036335));
#38481=CARTESIAN_POINT('Ctrl Pts',(4.94210130662626,4.62582679262985,120.936820830829));
#38482=CARTESIAN_POINT('Ctrl Pts',(4.82120593882783,4.75170835624018,120.945037625322));
#38483=CARTESIAN_POINT('Ctrl Pts',(4.69550995806903,4.87283031037143,120.953254419816));
#38484=CARTESIAN_POINT('Ctrl Pts',(4.56994151436316,4.99382936847227,120.961462877164));
#38485=CARTESIAN_POINT('Ctrl Pts',(4.43958242156076,5.11007819399288,120.969671334512));
#38486=CARTESIAN_POINT('Ctrl Pts',(4.30482944885586,5.22118113229788,120.977879791859));
#38487=CARTESIAN_POINT('Ctrl Pts',(4.17015618308229,5.33221835276307,120.986083393871));
#38488=CARTESIAN_POINT('Ctrl Pts',(4.0310944877603,5.43811551941107,120.994286995883));
#38489=CARTESIAN_POINT('Ctrl Pts',(3.88807664071038,5.53851505694101,121.002490597895));
#38490=CARTESIAN_POINT('Ctrl Pts',(3.74511689813727,5.63887380471834,121.010690866994));
#38491=CARTESIAN_POINT('Ctrl Pts',(3.59820449732004,5.73373916572205,121.018891136093));
#38492=CARTESIAN_POINT('Ctrl Pts',(3.4478033825354,5.82279493330973,121.027091405192));
#38493=CARTESIAN_POINT('Ctrl Pts',(3.33353580435362,5.89045524885949,121.033321577699));
#38494=CARTESIAN_POINT('Ctrl Pts',(3.21725514951042,5.95476294596038,121.039551750207));
#38495=CARTESIAN_POINT('Ctrl Pts',(3.09917575053254,6.01559628526642,121.045781922714));
#38496=CARTESIAN_POINT('Ctrl Pts',(3.09917575053247,6.01559628526645,119.046022396269));
#38497=CARTESIAN_POINT('Ctrl Pts',(2.94562386889167,6.09470469704523,119.054157343536));
#38498=CARTESIAN_POINT('Ctrl Pts',(2.78887073773776,6.16801775510825,119.062292290804));
#38499=CARTESIAN_POINT('Ctrl Pts',(2.62939800615144,6.23526704522323,119.070427238072));
#38500=CARTESIAN_POINT('Ctrl Pts',(2.47004920856827,6.30246407264947,119.078555863277));
#38501=CARTESIAN_POINT('Ctrl Pts',(2.30798535432348,6.36360657381629,119.086684488482));
#38502=CARTESIAN_POINT('Ctrl Pts',(2.14371192052861,6.41847241964812,119.094813113687));
#38503=CARTESIAN_POINT('Ctrl Pts',(1.97953161228569,6.47330716238519,119.102937130827));
#38504=CARTESIAN_POINT('Ctrl Pts',(1.81314456505499,6.52187222037921,119.111061147967));
#38505=CARTESIAN_POINT('Ctrl Pts',(1.64507542085962,6.56399389546361,119.119185165107));
#38506=CARTESIAN_POINT('Ctrl Pts',(1.47704468740609,6.60610594400535,119.127307325573));
#38507=CARTESIAN_POINT('Ctrl Pts',(1.30733297539201,6.64177744705332,119.13542948604));
#38508=CARTESIAN_POINT('Ctrl Pts',(1.13647944425169,6.67088475936988,119.143551646506));
#38509=CARTESIAN_POINT('Ctrl Pts',(0.965641992742876,6.6999893322941,119.151673042567));
#38510=CARTESIAN_POINT('Ctrl Pts',(0.793663296563194,6.72253088196121,119.159794438628));
#38511=CARTESIAN_POINT('Ctrl Pts',(0.621091916664614,6.73843704660464,119.167915834689));
#38512=CARTESIAN_POINT('Ctrl Pts',(0.448503918134599,6.75434474301242,119.176038012841));
#38513=CARTESIAN_POINT('Ctrl Pts',(0.275323486650185,6.76361574810797,119.184160190993));
#38514=CARTESIAN_POINT('Ctrl Pts',(0.102103459539556,6.76622966529736,119.192282369145));
#38515=CARTESIAN_POINT('Ctrl Pts',(-0.0711662339817113,6.76884433196063,
119.200406876123));
#38516=CARTESIAN_POINT('Ctrl Pts',(-0.244475179974578,6.76479810455379,
119.208531383102));
#38517=CARTESIAN_POINT('Ctrl Pts',(-0.417271432542778,6.75412270776773,
119.216655890081));
#38518=CARTESIAN_POINT('Ctrl Pts',(-0.590252249292328,6.74343590855923,
119.224789074869));
#38519=CARTESIAN_POINT('Ctrl Pts',(-0.762718913032112,6.72610581803722,
119.232922259657));
#38520=CARTESIAN_POINT('Ctrl Pts',(-0.934124560177369,6.70221607426032,
119.241055444445));
#38521=CARTESIAN_POINT('Ctrl Pts',(-1.1056239568358,6.67831326410034,119.249193077641));
#38522=CARTESIAN_POINT('Ctrl Pts',(-1.27606082085335,6.64784371569736,119.257330710836));
#38523=CARTESIAN_POINT('Ctrl Pts',(-1.44489964802669,6.61094199090662,119.265468344032));
#38524=CARTESIAN_POINT('Ctrl Pts',(-1.61399553029689,6.57398408368083,119.273618366676));
#38525=CARTESIAN_POINT('Ctrl Pts',(-1.78148816028607,6.53057452402652,119.281768389321));
#38526=CARTESIAN_POINT('Ctrl Pts',(-1.94685714723015,6.48089779646917,119.289918411966));
#38527=CARTESIAN_POINT('Ctrl Pts',(-2.10142186223526,6.43446666461561,119.297535958343));
#38528=CARTESIAN_POINT('Ctrl Pts',(-2.25413131420236,6.38256110597155,119.30515350472));
#38529=CARTESIAN_POINT('Ctrl Pts',(-2.40457833917693,6.32536892289779,119.312771051097));
#38530=CARTESIAN_POINT('Ctrl Pts',(-2.56701999842782,6.26361699981222,119.320995918775));
#38531=CARTESIAN_POINT('Ctrl Pts',(-2.72730940645269,6.19551687046572,119.329220786452));
#38532=CARTESIAN_POINT('Ctrl Pts',(-2.88491503761136,6.12123796513123,119.33744565413));
#38533=CARTESIAN_POINT('Ctrl Pts',(-3.04234310838568,6.04704274329765,119.345661255573));
#38534=CARTESIAN_POINT('Ctrl Pts',(-3.19709310142715,5.96668275832247,119.353876857017));
#38535=CARTESIAN_POINT('Ctrl Pts',(-3.34865059400865,5.88037653549886,119.36209245846));
#38536=CARTESIAN_POINT('Ctrl Pts',(-3.50006779105231,5.79415020564354,119.370300454789));
#38537=CARTESIAN_POINT('Ctrl Pts',(-3.64829806332022,5.70198877645099,119.378508451117));
#38538=CARTESIAN_POINT('Ctrl Pts',(-3.79284877840813,5.60415802276559,119.386716447445));
#38539=CARTESIAN_POINT('Ctrl Pts',(-3.93729471783775,5.50639818039747,119.394918494316));
#38540=CARTESIAN_POINT('Ctrl Pts',(-4.07806611648757,5.40297739882671,119.403120541188));
#38541=CARTESIAN_POINT('Ctrl Pts',(-4.21469661531684,5.29420640330889,119.411322588059));
#38542=CARTESIAN_POINT('Ctrl Pts',(-4.351255515978,5.1854924068073,119.419520336831));
#38543=CARTESIAN_POINT('Ctrl Pts',(-4.48367755967624,5.0714340046226,119.427718085602));
#38544=CARTESIAN_POINT('Ctrl Pts',(-4.61152689545234,4.95238414226116,119.435915834374));
#38545=CARTESIAN_POINT('Ctrl Pts',(-4.7393518465354,4.83335698626992,119.444112019589));
#38546=CARTESIAN_POINT('Ctrl Pts',(-4.86260556037688,4.70934050610102,119.452308204805));
#38547=CARTESIAN_POINT('Ctrl Pts',(-4.9808864818079,4.58072689159082,119.460504390021));
#38548=CARTESIAN_POINT('Ctrl Pts',(-5.0991586530833,4.45212279162556,119.468699968901));
#38549=CARTESIAN_POINT('Ctrl Pts',(-5.21245852102895,4.3189224981175,119.476895547781));
#38550=CARTESIAN_POINT('Ctrl Pts',(-5.32042256883231,4.18155386059534,119.485091126662));
#38551=CARTESIAN_POINT('Ctrl Pts',(-5.42839827247901,4.04417039269816,119.49328759034));
#38552=CARTESIAN_POINT('Ctrl Pts',(-5.53103678652313,3.90261796639809,119.501484054019));
#38553=CARTESIAN_POINT('Ctrl Pts',(-5.6280159196581,3.7573562258688,119.509680517697));
#38554=CARTESIAN_POINT('Ctrl Pts',(-5.72502316697936,3.6120523740574,119.517879357525));
#38555=CARTESIAN_POINT('Ctrl Pts',(-5.81636756623627,3.46303736446124,119.526078197353));
#38556=CARTESIAN_POINT('Ctrl Pts',(-5.90177113624453,3.31079846191081,119.534277037181));
#38557=CARTESIAN_POINT('Ctrl Pts',(-5.98726391271099,3.15840054149617,119.54248444093));
#38558=CARTESIAN_POINT('Ctrl Pts',(-6.0668032866236,3.00277231377503,119.550691844679));
#38559=CARTESIAN_POINT('Ctrl Pts',(-6.14015755615572,2.84442510634114,119.558899248428));
#38560=CARTESIAN_POINT('Ctrl Pts',(-6.21355111811655,2.68599307976314,119.567111048497));
#38561=CARTESIAN_POINT('Ctrl Pts',(-6.28075283303179,2.52483950091763,119.575322848566));
#38562=CARTESIAN_POINT('Ctrl Pts',(-6.34157983285418,2.36149406595426,119.583534648635));
#38563=CARTESIAN_POINT('Ctrl Pts',(-6.40249637851955,2.19790816368667,119.591758537622));
#38564=CARTESIAN_POINT('Ctrl Pts',(-6.45701934238125,2.03212429766803,119.599982426608));
#38565=CARTESIAN_POINT('Ctrl Pts',(-6.50501589122862,1.86468690531767,119.608206315594));
#38566=CARTESIAN_POINT('Ctrl Pts',(-6.54936387260667,1.70997764941767,119.615805046844));
#38567=CARTESIAN_POINT('Ctrl Pts',(-6.58814047872425,1.55385705238916,119.623403778094));
#38568=CARTESIAN_POINT('Ctrl Pts',(-6.6212801170397,1.39676004084263,119.631002509344));
#38569=CARTESIAN_POINT('Ctrl Pts',(-6.67106662401678,1.16074927370662,119.642418273233));
#38570=CARTESIAN_POINT('Ctrl Pts',(-6.7082475624925,0.921995435047206,119.653834037122));
#38571=CARTESIAN_POINT('Ctrl Pts',(-6.73258355588105,0.681621348756109,
119.665249801012));
#38572=CARTESIAN_POINT('Ctrl Pts',(-6.75527287852273,0.457511935530984,
119.675893128611));
#38573=CARTESIAN_POINT('Ctrl Pts',(-6.76679704929885,0.231993769023563,
119.686536456211));
#38574=CARTESIAN_POINT('Ctrl Pts',(-6.76699734236883,0.00599736385734007,
119.69717978381));
#38575=CARTESIAN_POINT('',(-6.76734675747272,0.000426170603140981,119.303420271511));
#38576=CARTESIAN_POINT('Ctrl Pts',(3.09917575053251,6.01559628526643,118.651527161978));
#38577=CARTESIAN_POINT('Ctrl Pts',(2.9364285471412,6.09944203592837,118.660124864592));
#38578=CARTESIAN_POINT('Ctrl Pts',(2.77016691089095,6.17673605197334,118.668722567206));
#38579=CARTESIAN_POINT('Ctrl Pts',(2.60093428501794,6.24719375760175,118.677320269819));
#38580=CARTESIAN_POINT('Ctrl Pts',(2.45558957732084,6.30770605289198,118.684704369468));
#38581=CARTESIAN_POINT('Ctrl Pts',(2.30805396901044,6.36317642841517,118.692088469117));
#38582=CARTESIAN_POINT('Ctrl Pts',(2.15868605499137,6.41345176297334,118.699472568766));
#38583=CARTESIAN_POINT('Ctrl Pts',(1.98480833998704,6.4719767839021,118.708068326314));
#38584=CARTESIAN_POINT('Ctrl Pts',(1.80865124904983,6.52339225558145,118.716664083861));
#38585=CARTESIAN_POINT('Ctrl Pts',(1.63081208939963,6.56755212610209,118.725259841409));
#38586=CARTESIAN_POINT('Ctrl Pts',(1.4528069997693,6.61175319928277,118.73386361909));
#38587=CARTESIAN_POINT('Ctrl Pts',(1.27311700509798,6.6486850851154,118.742467396772));
#38588=CARTESIAN_POINT('Ctrl Pts',(1.09234916559985,6.67825293773853,118.751071174453));
#38589=CARTESIAN_POINT('Ctrl Pts',(0.90447699193578,6.70898283282556,118.760013088121));
#38590=CARTESIAN_POINT('Ctrl Pts',(0.715440913483375,6.73175811563873,118.768955001789));
#38591=CARTESIAN_POINT('Ctrl Pts',(0.525926353928126,6.74653173639937,118.777896915457));
#38592=CARTESIAN_POINT('Ctrl Pts',(0.343081773831211,6.76078539844428,118.786524117788));
#38593=CARTESIAN_POINT('Ctrl Pts',(0.159792117190445,6.76759107506568,118.795151320119));
#38594=CARTESIAN_POINT('Ctrl Pts',(-0.0233282844672006,6.76695978938429,
118.80377852245));
#38595=CARTESIAN_POINT('Ctrl Pts',(-0.206623080280642,6.7663279024999,118.81241394087));
#38596=CARTESIAN_POINT('Ctrl Pts',(-0.389747994752091,6.75824492624368,
118.82104935929));
#38597=CARTESIAN_POINT('Ctrl Pts',(-0.572092798571519,6.74277382312521,
118.829684777711));
#38598=CARTESIAN_POINT('Ctrl Pts',(-0.754706990862874,6.72727986365581,
118.838332953732));
#38599=CARTESIAN_POINT('Ctrl Pts',(-0.936538466375629,6.70437599947752,
118.846981129753));
#38600=CARTESIAN_POINT('Ctrl Pts',(-1.11698469582036,6.6741766675226,118.855629305774));
#38601=CARTESIAN_POINT('Ctrl Pts',(-1.13607522269945,6.67098169270828,118.856544250006));
#38602=CARTESIAN_POINT('Ctrl Pts',(-1.15515025678087,6.66770510744618,118.857459194238));
#38603=CARTESIAN_POINT('Ctrl Pts',(-1.17420909350834,6.66434708015139,118.85837413847));
#38604=CARTESIAN_POINT('Ctrl Pts',(-1.34556144845317,6.63415605154042,118.866600131011));
#38605=CARTESIAN_POINT('Ctrl Pts',(-1.51597355623133,6.59731248824598,118.874826123552));
#38606=CARTESIAN_POINT('Ctrl Pts',(-1.68489097720878,6.55388673955543,118.883052116094));
#38607=CARTESIAN_POINT('Ctrl Pts',(-1.85363131010308,6.51050651714955,118.891269484745));
#38608=CARTESIAN_POINT('Ctrl Pts',(-2.02087973248993,6.46055793941455,118.899486853396));
#38609=CARTESIAN_POINT('Ctrl Pts',(-2.18608979098266,6.40416274197973,118.907704222048));
#38610=CARTESIAN_POINT('Ctrl Pts',(-2.3511597059005,6.3478153831853,118.91591462011));
#38611=CARTESIAN_POINT('Ctrl Pts',(-2.5141943634725,6.28503241105296,118.924125018173));
#38612=CARTESIAN_POINT('Ctrl Pts',(-2.67466023208142,6.21598597512271,118.932335416235));
#38613=CARTESIAN_POINT('Ctrl Pts',(-2.8350220809772,6.14698429756083,118.940540492024));
#38614=CARTESIAN_POINT('Ctrl Pts',(-2.99281812989276,6.07172738493515,118.948745567813));
#38615=CARTESIAN_POINT('Ctrl Pts',(-3.14753258526244,5.99043634677067,118.956950643601));
#38616=CARTESIAN_POINT('Ctrl Pts',(-3.30217769187314,5.90918174626549,118.965152041571));
#38617=CARTESIAN_POINT('Ctrl Pts',(-3.45374364035245,5.82189857511661,118.97335343954));
#38618=CARTESIAN_POINT('Ctrl Pts',(-3.60173702516266,5.72885498171951,118.98155483751));
#38619=CARTESIAN_POINT('Ctrl Pts',(-3.74971881790022,5.63581867627042,118.989755593077));
#38620=CARTESIAN_POINT('Ctrl Pts',(-3.89412829664089,5.53702303048263,118.997956348645));
#38621=CARTESIAN_POINT('Ctrl Pts',(-4.03449864668078,5.43278102539859,119.006157104213));
#38622=CARTESIAN_POINT('Ctrl Pts',(-4.17486828370632,5.32853954981417,119.014357818125));
#38623=CARTESIAN_POINT('Ctrl Pts',(-4.31119854454766,5.21885198284553,119.022558532036));
#38624=CARTESIAN_POINT('Ctrl Pts',(-4.44305359015752,5.10407325525295,119.030759245948));
#38625=CARTESIAN_POINT('Ctrl Pts',(-4.57493186142344,4.98927430991869,119.038961404378));
#38626=CARTESIAN_POINT('Ctrl Pts',(-4.7023330766182,4.86938265257377,119.047163562807));
#38627=CARTESIAN_POINT('Ctrl Pts',(-4.82485629627255,4.7447919575382,119.055365721237));
#38628=CARTESIAN_POINT('Ctrl Pts',(-4.94742330231965,4.62015673725164,119.06357081089));
#38629=CARTESIAN_POINT('Ctrl Pts',(-5.06510858903167,4.49081938935732,119.071775900543));
#38630=CARTESIAN_POINT('Ctrl Pts',(-5.17754970096221,4.35720875034306,119.079980990196));
#38631=CARTESIAN_POINT('Ctrl Pts',(-5.29011926356815,4.22344547697179,119.088195453194));
#38632=CARTESIAN_POINT('Ctrl Pts',(-5.397432451742,4.08539943411786,119.096409916192));
#38633=CARTESIAN_POINT('Ctrl Pts',(-5.49916793506262,3.9435315419024,119.104624379189));
#38634=CARTESIAN_POINT('Ctrl Pts',(-5.60096369344182,3.80157959744446,119.112843708997));
#38635=CARTESIAN_POINT('Ctrl Pts',(-5.6971749625305,3.65580158855592,119.121063038804));
#38636=CARTESIAN_POINT('Ctrl Pts',(-5.78752511743648,3.50668533162613,119.129282368612));
#38637=CARTESIAN_POINT('Ctrl Pts',(-5.87801526442972,3.3573380280969,119.137514433772));
#38638=CARTESIAN_POINT('Ctrl Pts',(-5.96262597540469,3.20464245327407,119.145746498933));
#38639=CARTESIAN_POINT('Ctrl Pts',(-6.04112714443894,3.0491100053496,119.153978564094));
#38640=CARTESIAN_POINT('Ctrl Pts',(-6.11168963186089,2.90930627331108,119.161378135355));
#38641=CARTESIAN_POINT('Ctrl Pts',(-6.17731636364992,2.76721088265161,119.168777706616));
#38642=CARTESIAN_POINT('Ctrl Pts',(-6.23787435940597,2.62320652566006,119.176177277877));
#38643=CARTESIAN_POINT('Ctrl Pts',(-6.31224016700351,2.44636777511126,119.185264023333));
#38644=CARTESIAN_POINT('Ctrl Pts',(-6.3791586711013,2.26618310769137,119.194350768788));
#38645=CARTESIAN_POINT('Ctrl Pts',(-6.4383458134576,2.08326479025903,119.203437514243));
#38646=CARTESIAN_POINT('Ctrl Pts',(-6.49727338773895,1.9011486699533,119.212484409337));
#38647=CARTESIAN_POINT('Ctrl Pts',(-6.54853714765832,1.71632302445248,119.22153130443));
#38648=CARTESIAN_POINT('Ctrl Pts',(-6.59190212197188,1.52941669088011,119.230578199524));
#38649=CARTESIAN_POINT('Ctrl Pts',(-6.63514767601595,1.34302506774115,119.239600180902));
#38650=CARTESIAN_POINT('Ctrl Pts',(-6.67053776868456,1.15456440198809,119.24862216228));
#38651=CARTESIAN_POINT('Ctrl Pts',(-6.69788636448025,0.964679868406895,
119.257644143657));
#38652=CARTESIAN_POINT('Ctrl Pts',(-6.7251110861169,0.775655407755472,119.266625260401));
#38653=CARTESIAN_POINT('Ctrl Pts',(-6.74436689747264,0.585220162905082,
119.275606377145));
#38654=CARTESIAN_POINT('Ctrl Pts',(-6.75551850612324,0.394028823090993,
119.284587493889));
#38655=CARTESIAN_POINT('Ctrl Pts',(-6.76306486476055,0.264648527943292,
119.290665067989));
#38656=CARTESIAN_POINT('Ctrl Pts',(-6.76690105714519,0.134922369537897,
119.29674264209));
#38657=CARTESIAN_POINT('Ctrl Pts',(-6.76699811026943,0.00505723343474368,
119.30282021619));
#38658=CARTESIAN_POINT('Ctrl Pts',(-6.767,6.83169908337797E-12,119.30282021619));
#38659=CARTESIAN_POINT('Ctrl Pts',(-6.76700000000019,-0.186007249408865,
119.311569727996));
#38660=CARTESIAN_POINT('Ctrl Pts',(-6.75932637295476,-0.372014355520747,
119.320319239802));
#38661=CARTESIAN_POINT('Ctrl Pts',(-6.74400518266984,-0.557389537148295,
119.329068751608));
#38662=CARTESIAN_POINT('Ctrl Pts',(-6.72868405709716,-0.74276393580507,
119.337818226458));
#38663=CARTESIAN_POINT('Ctrl Pts',(-6.70571545653074,-0.927506129689138,
119.346567701309));
#38664=CARTESIAN_POINT('Ctrl Pts',(-6.67517739415741,-1.11098863924429,
119.35531717616));
#38665=CARTESIAN_POINT('Ctrl Pts',(-6.64463945823172,-1.29447038906135,
119.364066614782));
#38666=CARTESIAN_POINT('Ctrl Pts',(-6.60653217027236,-1.47669218227865,
119.372816053404));
#38667=CARTESIAN_POINT('Ctrl Pts',(-6.56098496116797,-1.65703510503784,
119.381565492026));
#38668=CARTESIAN_POINT('Ctrl Pts',(-6.51543793687607,-1.83737729603703,
119.390314895146));
#38669=CARTESIAN_POINT('Ctrl Pts',(-6.46245112202733,-2.01584035396754,
119.399064298266));
#38670=CARTESIAN_POINT('Ctrl Pts',(-6.40220448416338,-2.19181813637863,
119.407813701386));
#38671=CARTESIAN_POINT('Ctrl Pts',(-6.34195808575291,-2.36779521935663,
119.416563069732));
#38672=CARTESIAN_POINT('Ctrl Pts',(-6.27445201489348,-2.54128677544547,
119.425312438077));
#38673=CARTESIAN_POINT('Ctrl Pts',(-6.19991555136306,-2.71170355237562,
119.434061806422));
#38674=CARTESIAN_POINT('Ctrl Pts',(-6.12537937789167,-2.88211966612799,
119.442811140719));
#38675=CARTESIAN_POINT('Ctrl Pts',(-6.04381298133752,-3.04946076210177,
119.451560475016));
#38676=CARTESIAN_POINT('Ctrl Pts',(-5.95549339426448,-3.21315848206592,
119.460309809313));
#38677=CARTESIAN_POINT('Ctrl Pts',(-5.8671741435532,-3.37685557859358,119.469059110289));
#38678=CARTESIAN_POINT('Ctrl Pts',(-5.77210188986416,-3.53690907467019,
119.477808411264));
#38679=CARTESIAN_POINT('Ctrl Pts',(-5.67059953467267,-3.692775367846,119.48655771224));
#38680=CARTESIAN_POINT('Ctrl Pts',(-5.56909755761972,-3.84864108035495,
119.495306980621));
#38681=CARTESIAN_POINT('Ctrl Pts',(-5.46116568338284,-4.00031938103988,
119.504056249001));
#38682=CARTESIAN_POINT('Ctrl Pts',(-5.34717048686335,-4.14729511662934,
119.512805517382));
#38683=CARTESIAN_POINT('Ctrl Pts',(-5.23317570555738,-4.29427031687772,
119.521554753895));
#38684=CARTESIAN_POINT('Ctrl Pts',(-5.11311782179025,-4.43654275986877,
119.530303990407));
#38685=CARTESIAN_POINT('Ctrl Pts',(-4.98740459172232,-4.57362924147412,
119.53905322692));
#38686=CARTESIAN_POINT('Ctrl Pts',(-4.86169180911051,-4.71071523514209,
119.547802432291));
#38687=CARTESIAN_POINT('Ctrl Pts',(-4.73032391415654,-4.84261509316307,
119.556551637662));
#38688=CARTESIAN_POINT('Ctrl Pts',(-4.59374707237517,-4.96888084331317,
119.565300843033));
#38689=CARTESIAN_POINT('Ctrl Pts',(-4.45717070537638,-5.09514615452517,
119.57405001799));
#38690=CARTESIAN_POINT('Ctrl Pts',(-4.31538563819758,-5.21577720253427,
119.582799192946));
#38691=CARTESIAN_POINT('Ctrl Pts',(-4.16887341290909,-5.33036429028446,
119.591548367902));
#38692=CARTESIAN_POINT('Ctrl Pts',(-4.02236168477605,-5.44495098920979,
119.60029751317));
#38693=CARTESIAN_POINT('Ctrl Pts',(-3.87112305634711,-5.55349359238569,
119.609046658438));
#38694=CARTESIAN_POINT('Ctrl Pts',(-3.7156711731701,-5.65562346102291,119.617795803706));
#38695=CARTESIAN_POINT('Ctrl Pts',(-3.56021980457576,-5.75775299158599,
119.626544920012));
#38696=CARTESIAN_POINT('Ctrl Pts',(-3.4005554486266,-5.85346967275195,119.635294036318));
#38697=CARTESIAN_POINT('Ctrl Pts',(-3.23722036323671,-5.94244842803415,
119.644043152624));
#38698=CARTESIAN_POINT('Ctrl Pts',(-3.07388580496343,-6.03142689616323,
119.652792240695));
#38699=CARTESIAN_POINT('Ctrl Pts',(-2.90688079258032,-6.11366734484667,
119.661541328766));
#38700=CARTESIAN_POINT('Ctrl Pts',(-2.7367725109497,-6.18889046787145,119.670290416837));
#38701=CARTESIAN_POINT('Ctrl Pts',(-2.56666476417012,-6.2641133543812,119.679039477399));
#38702=CARTESIAN_POINT('Ctrl Pts',(-2.39345402972472,-6.33231884350147,
119.687788537962));
#38703=CARTESIAN_POINT('Ctrl Pts',(-2.21772856474429,-6.39327529620908,
119.696537598524));
#38704=CARTESIAN_POINT('Ctrl Pts',(-2.04200363768658,-6.45423156231959,
119.705286632304));
#38705=CARTESIAN_POINT('Ctrl Pts',(-1.86376426620479,-6.50793874251945,
119.714035666084));
#38706=CARTESIAN_POINT('Ctrl Pts',(-1.68361578195071,-6.55421443796024,
119.722784699864));
#38707=CARTESIAN_POINT('Ctrl Pts',(-1.50346783420238,-6.60048999558596,
119.731533707588));
#38708=CARTESIAN_POINT('Ctrl Pts',(-1.32141106257604,-6.63933404145425,
119.740282715312));
#38709=CARTESIAN_POINT('Ctrl Pts',(-1.13806375959388,-6.67061465526971,
119.749031723037));
#38710=CARTESIAN_POINT('Ctrl Pts',(-0.954716987422261,-6.70189517852437,
119.757780705431));
#38711=CARTESIAN_POINT('Ctrl Pts',(-0.770079973812654,-6.72561226535797,
119.766529687826));
#38712=CARTESIAN_POINT('Ctrl Pts',(-0.584779770554896,-6.74168536939761,
119.775278670221));
#38713=CARTESIAN_POINT('Ctrl Pts',(-0.391490647556318,-6.7584514394238,
119.784404850897));
#38714=CARTESIAN_POINT('Ctrl Pts',(-0.197480213106707,-6.7668997592402,
119.793531031573));
#38715=CARTESIAN_POINT('Ctrl Pts',(-0.00346532630012875,-6.76699911271707,
119.802657212249));
#38716=CARTESIAN_POINT('Ctrl Pts',(0.184486595293712,-6.7670953613978,119.811498199779));
#38717=CARTESIAN_POINT('Ctrl Pts',(0.372442378182879,-6.75935659726783,
119.820339187309));
#38718=CARTESIAN_POINT('Ctrl Pts',(0.55975021771973,-6.74380965729036,119.829180174839));
#38719=CARTESIAN_POINT('Ctrl Pts',(0.745129914455429,-6.72842275717279,
119.837930153437));
#38720=CARTESIAN_POINT('Ctrl Pts',(0.929874656311892,-6.70538772273505,
119.846680132035));
#38721=CARTESIAN_POINT('Ctrl Pts',(1.11335688289552,-6.6747828018078,119.855430110633));
#38722=CARTESIAN_POINT('Ctrl Pts',(1.29683723118622,-6.64417819418069,119.864179999657));
#38723=CARTESIAN_POINT('Ctrl Pts',(1.47905480729991,-6.60600390230129,119.872929888682));
#38724=CARTESIAN_POINT('Ctrl Pts',(1.65939064804556,-6.56038959797198,119.881679777707));
#38725=CARTESIAN_POINT('Ctrl Pts',(1.8397247026401,-6.51477574543328,119.890429580068));
#38726=CARTESIAN_POINT('Ctrl Pts',(2.0181767812559,-6.4617220982018,119.899179382429));
#38727=CARTESIAN_POINT('Ctrl Pts',(2.1941407234742,-6.40140886724103,119.90792918479));
#38728=CARTESIAN_POINT('Ctrl Pts',(2.37010298131849,-6.34109621361467,119.916678903396));
#38729=CARTESIAN_POINT('Ctrl Pts',(2.54357687926678,-6.27352420826067,119.925428622001));
#38730=CARTESIAN_POINT('Ctrl Pts',(2.71397317789748,-6.19892237325594,119.934178340607));
#38731=CARTESIAN_POINT('Ctrl Pts',(2.88436790206976,-6.12432122757069,119.942927978365));
#38732=CARTESIAN_POINT('Ctrl Pts',(3.0516848212603,-6.04269049717531,119.951677616123));
#38733=CARTESIAN_POINT('Ctrl Pts',(3.21535561997161,-5.95430745235052,119.960427253881));
#38734=CARTESIAN_POINT('Ctrl Pts',(3.37902496075058,-5.86592519481645,119.9691768137));
#38735=CARTESIAN_POINT('Ctrl Pts',(3.53904799384657,-5.77079087940366,119.977926373519));
#38736=CARTESIAN_POINT('Ctrl Pts',(3.69488118814771,-5.66922763747163,119.986675933338));
#38737=CARTESIAN_POINT('Ctrl Pts',(3.85071304610618,-5.56766526649201,119.995425418126));
#38738=CARTESIAN_POINT('Ctrl Pts',(4.0023548970575,-5.45967423580873,120.004174902913));
#38739=CARTESIAN_POINT('Ctrl Pts',(4.14929168607435,-5.34562133936498,120.012924387701));
#38740=CARTESIAN_POINT('Ctrl Pts',(4.29622726385545,-5.23156938308705,120.021673800364));
#38741=CARTESIAN_POINT('Ctrl Pts',(4.43845763091862,-5.1114558367738,120.030423213027));
#38742=CARTESIAN_POINT('Ctrl Pts',(4.57549970660765,-4.98568866204393,120.039172625691));
#38743=CARTESIAN_POINT('Ctrl Pts',(4.71254069815098,-4.85992248226352,120.047921969137));
#38744=CARTESIAN_POINT('Ctrl Pts',(4.84439326931117,-4.72850295734203,120.056671312583));
#38745=CARTESIAN_POINT('Ctrl Pts',(4.97060959434503,-4.59187644221893,120.06542065603));
#38746=CARTESIAN_POINT('Ctrl Pts',(5.09682496280324,-4.45525096256883,120.074169933166));
#38747=CARTESIAN_POINT('Ctrl Pts',(5.21740397615652,-4.31341878218552,120.082919210302));
#38748=CARTESIAN_POINT('Ctrl Pts',(5.33193710451751,-4.16686161438911,120.091668487439));
#38749=CARTESIAN_POINT('Ctrl Pts',(5.44646940289213,-4.02030550864745,120.100417701171));
#38750=CARTESIAN_POINT('Ctrl Pts',(5.55495572749507,-3.86902470980361,120.109166914904));
#38751=CARTESIAN_POINT('Ctrl Pts',(5.65702762491309,-3.71353301466005,120.117916128637));
#38752=CARTESIAN_POINT('Ctrl Pts',(5.75909881655017,-3.55804239467115,120.126665281874));
#38753=CARTESIAN_POINT('Ctrl Pts',(5.85475551250654,-3.39834117619774,120.13541443511));
#38754=CARTESIAN_POINT('Ctrl Pts',(5.94367283727975,-3.23497174692189,120.144163588346));
#38755=CARTESIAN_POINT('Ctrl Pts',(6.03258957676195,-3.07160339301194,120.152912683991));
#38756=CARTESIAN_POINT('Ctrl Pts',(6.11476689685172,-2.90456712829741,120.161661779637));
#38757=CARTESIAN_POINT('Ctrl Pts',(6.18992570525153,-2.7344302447615,120.170410875282));
#38758=CARTESIAN_POINT('Ctrl Pts',(6.26508404388595,-2.56429442463281,120.179159916243));
#38759=CARTESIAN_POINT('Ctrl Pts',(6.33322384283218,-2.3910582865625,120.187908957204));
#38760=CARTESIAN_POINT('Ctrl Pts',(6.39411368719942,-2.21531017132344,120.196657998165));
#38761=CARTESIAN_POINT('Ctrl Pts',(6.45500317120806,-2.03956309619781,120.205406987348));
#38762=CARTESIAN_POINT('Ctrl Pts',(6.50864269269996,-1.86130434438902,120.21415597653));
#38763=CARTESIAN_POINT('Ctrl Pts',(6.55485008446264,-1.68113930720216,120.222904965713));
#38764=CARTESIAN_POINT('Ctrl Pts',(6.60199664749344,-1.49731239212105,120.231831779242));
#38765=CARTESIAN_POINT('Ctrl Pts',(6.64140563640856,-1.3115011649993,120.240758592771));
#38766=CARTESIAN_POINT('Ctrl Pts',(6.6729377228213,-1.12436255155912,120.249685406301));
#38767=CARTESIAN_POINT('Ctrl Pts',(6.70384494949835,-0.940932395053909,
120.258435320456));
#38768=CARTESIAN_POINT('Ctrl Pts',(6.72718449348901,-0.756227260509322,
120.267185234612));
#38769=CARTESIAN_POINT('Ctrl Pts',(6.7428770737391,-0.570874564544338,120.275935148767));
#38770=CARTESIAN_POINT('Ctrl Pts',(6.75856934538655,-0.385525513635181,
120.284684890851));
#38771=CARTESIAN_POINT('Ctrl Pts',(6.76661493004095,-0.199529212420992,
120.293434632935));
#38772=CARTESIAN_POINT('Ctrl Pts',(6.76698649908906,-0.013517438603244,
120.302184375019));
#38773=CARTESIAN_POINT('Ctrl Pts',(6.76735806132397,0.172490924442939,120.310933956665));
#38774=CARTESIAN_POINT('Ctrl Pts',(6.76005588896304,0.358514472898549,120.319683538311));
#38775=CARTESIAN_POINT('Ctrl Pts',(6.74510478454608,0.543921359659338,120.328433119957));
#38776=CARTESIAN_POINT('Ctrl Pts',(6.73015393440718,0.729325093147661,120.337182552796));
#38777=CARTESIAN_POINT('Ctrl Pts',(6.70755443556934,0.91411190025366,120.345931985635));
#38778=CARTESIAN_POINT('Ctrl Pts',(6.67738304682361,1.09765415591278,120.354681418474));
#38779=CARTESIAN_POINT('Ctrl Pts',(6.64721213111908,1.28119353391025,120.363430714135));
#38780=CARTESIAN_POINT('Ctrl Pts',(6.60946960955547,1.46348811672417,120.372180009797));
#38781=CARTESIAN_POINT('Ctrl Pts',(6.56428366991239,1.64391876347998,120.380929305458));
#38782=CARTESIAN_POINT('Ctrl Pts',(6.5190983786778,1.82434682109494,120.389678475569));
#38783=CARTESIAN_POINT('Ctrl Pts',(6.46646995271989,2.00291071820225,120.39842764568));
#38784=CARTESIAN_POINT('Ctrl Pts',(6.40657713281623,2.17900400212486,120.407176815791));
#38785=CARTESIAN_POINT('Ctrl Pts',(6.34668509279139,2.35509499309444,120.415925871976));
#38786=CARTESIAN_POINT('Ctrl Pts',(6.2795289403761,2.52871516397912,120.424674928162));
#38787=CARTESIAN_POINT('Ctrl Pts',(6.20533675061536,2.69927486771214,120.433423984348));
#38788=CARTESIAN_POINT('Ctrl Pts',(6.1283211790801,2.87632521635724,120.44250598563));
#38789=CARTESIAN_POINT('Ctrl Pts',(6.04372366626177,3.05007728919804,120.451587986912));
#38790=CARTESIAN_POINT('Ctrl Pts',(5.95185378007969,3.21989527478009,120.460669988195));
#38791=CARTESIAN_POINT('Ctrl Pts',(5.86334450817478,3.38350129286567,120.469419768502));
#38792=CARTESIAN_POINT('Ctrl Pts',(5.76808562057368,3.54345567124778,120.478169548809));
#38793=CARTESIAN_POINT('Ctrl Pts',(5.66640068804603,3.69921508465127,120.486919329116));
#38794=CARTESIAN_POINT('Ctrl Pts',(5.56471941108049,3.85496889852101,120.49566879487));
#38795=CARTESIAN_POINT('Ctrl Pts',(5.45661270815247,4.00652780919455,120.504418260623));
#38796=CARTESIAN_POINT('Ctrl Pts',(5.34244776449255,4.15337704569048,120.513167726377));
#38797=CARTESIAN_POINT('Ctrl Pts',(5.2282863181974,4.30022178356074,120.521916924096));
#38798=CARTESIAN_POINT('Ctrl Pts',(5.10806717844218,4.44235690972508,120.530666121816));
#38799=CARTESIAN_POINT('Ctrl Pts',(4.98219864544872,4.57929969070479,120.539415319535));
#38800=CARTESIAN_POINT('Ctrl Pts',(4.85633329944181,4.7162390042984,120.548164295726));
#38801=CARTESIAN_POINT('Ctrl Pts',(4.72481904033808,4.84798602483461,120.556913271916));
#38802=CARTESIAN_POINT('Ctrl Pts',(4.58810250737362,4.97409332258975,120.565662248106));
#38803=CARTESIAN_POINT('Ctrl Pts',(4.45137708685812,5.10020881821987,120.574411793042));
#38804=CARTESIAN_POINT('Ctrl Pts',(4.30944892636227,5.22068366307788,120.583161337978));
#38805=CARTESIAN_POINT('Ctrl Pts',(4.16280009466842,5.33510865604709,120.591910882915));
#38806=CARTESIAN_POINT('Ctrl Pts',(4.01615988348969,5.44952692272759,120.600659913523));
#38807=CARTESIAN_POINT('Ctrl Pts',(3.86479978232409,5.55789587288503,120.609408944131));
#38808=CARTESIAN_POINT('Ctrl Pts',(3.70923383581243,5.65984746713763,120.618157974739));
#38809=CARTESIAN_POINT('Ctrl Pts',(3.55366577799719,5.76180044505272,120.626907124087));
#38810=CARTESIAN_POINT('Ctrl Pts',(3.39389200027023,5.85733573570953,120.635656273435));
#38811=CARTESIAN_POINT('Ctrl Pts',(3.23045513626227,5.94612887621827,120.644405422784));
#38812=CARTESIAN_POINT('Ctrl Pts',(3.18695122151708,5.9697639920662,120.646734286897));
#38813=CARTESIAN_POINT('Ctrl Pts',(3.14318791262736,5.99292165435295,120.649063151009));
#38814=CARTESIAN_POINT('Ctrl Pts',(3.09917575053273,6.01559628526632,120.651392015122));
#38815=CARTESIAN_POINT('Origin',(0.,0.,-3.69717978381041));
#38816=CARTESIAN_POINT('',(3.09917575053267,6.01559628526635,123.045751582742));
#38817=CARTESIAN_POINT('',(3.0991757505325,6.01559628526643,122.651206263353));
#38818=CARTESIAN_POINT('',(3.09917575053259,6.01559628526639,-3.69717978381041));
#38819=CARTESIAN_POINT('',(-6.767,6.76859095031027E-12,121.69717978381));
#38820=CARTESIAN_POINT('Ctrl Pts',(-6.767,6.7685908980338E-12,121.69717978381));
#38821=CARTESIAN_POINT('Ctrl Pts',(-6.76700000000019,-0.186007249408928,
121.705929295616));
#38822=CARTESIAN_POINT('Ctrl Pts',(-6.75932637295475,-0.372014355520807,
121.714678807422));
#38823=CARTESIAN_POINT('Ctrl Pts',(-6.74400518266983,-0.557389537148355,
121.723428319228));
#38824=CARTESIAN_POINT('Ctrl Pts',(-6.72868405709718,-0.742763935804875,
121.732177794078));
#38825=CARTESIAN_POINT('Ctrl Pts',(-6.70571545653079,-0.927506129688694,
121.740927268929));
#38826=CARTESIAN_POINT('Ctrl Pts',(-6.67517739415753,-1.1109886392436,121.74967674378));
#38827=CARTESIAN_POINT('Ctrl Pts',(-6.64463945823183,-1.29447038906078,
121.758426182402));
#38828=CARTESIAN_POINT('Ctrl Pts',(-6.60653217027247,-1.47669218227821,
121.767175621024));
#38829=CARTESIAN_POINT('Ctrl Pts',(-6.56098496116805,-1.65703510503753,
121.775925059646));
#38830=CARTESIAN_POINT('Ctrl Pts',(-6.51543793687619,-1.83737729603659,
121.784674462766));
#38831=CARTESIAN_POINT('Ctrl Pts',(-6.4624511220275,-2.01584035396699,121.793423865886));
#38832=CARTESIAN_POINT('Ctrl Pts',(-6.40220448416361,-2.19181813637796,
121.802173269006));
#38833=CARTESIAN_POINT('Ctrl Pts',(-6.34195808575316,-2.36779521935597,
121.810922637351));
#38834=CARTESIAN_POINT('Ctrl Pts',(-6.27445201489374,-2.54128677544482,
121.819672005697));
#38835=CARTESIAN_POINT('Ctrl Pts',(-6.19991555136334,-2.71170355237498,
121.828421374042));
#38836=CARTESIAN_POINT('Ctrl Pts',(-6.12537937789192,-2.88211966612747,
121.837170708339));
#38837=CARTESIAN_POINT('Ctrl Pts',(-6.04381298133772,-3.04946076210137,
121.845920042636));
#38838=CARTESIAN_POINT('Ctrl Pts',(-5.95549339426463,-3.21315848206564,
121.854669376933));
#38839=CARTESIAN_POINT('Ctrl Pts',(-5.8671741435533,-3.37685557859342,121.863418677909));
#38840=CARTESIAN_POINT('Ctrl Pts',(-5.7721018898642,-3.53690907467014,121.872167978884));
#38841=CARTESIAN_POINT('Ctrl Pts',(-5.67059953467263,-3.69277536784605,
121.88091727986));
#38842=CARTESIAN_POINT('Ctrl Pts',(-5.56909755761975,-3.84864108035489,
121.889666548241));
#38843=CARTESIAN_POINT('Ctrl Pts',(-5.46116568338295,-4.00031938103972,
121.898415816621));
#38844=CARTESIAN_POINT('Ctrl Pts',(-5.34717048686355,-4.14729511662908,
121.907165085002));
#38845=CARTESIAN_POINT('Ctrl Pts',(-5.23317570555759,-4.29427031687747,
121.915914321515));
#38846=CARTESIAN_POINT('Ctrl Pts',(-5.11311782179046,-4.43654275986852,
121.924663558027));
#38847=CARTESIAN_POINT('Ctrl Pts',(-4.98740459172254,-4.57362924147388,
121.93341279454));
#38848=CARTESIAN_POINT('Ctrl Pts',(-4.8616918091109,-4.71071523514167,121.942161999911));
#38849=CARTESIAN_POINT('Ctrl Pts',(-4.73032391415713,-4.84261509316248,
121.950911205282));
#38850=CARTESIAN_POINT('Ctrl Pts',(-4.59374707237597,-4.96888084331243,
121.959660410653));
#38851=CARTESIAN_POINT('Ctrl Pts',(-4.4571707053772,-5.09514615452446,121.96840958561));
#38852=CARTESIAN_POINT('Ctrl Pts',(-4.31538563819842,-5.21577720253357,
121.977158760566));
#38853=CARTESIAN_POINT('Ctrl Pts',(-4.16887341290995,-5.33036429028378,
121.985907935522));
#38854=CARTESIAN_POINT('Ctrl Pts',(-4.02236168477693,-5.44495098920914,
121.99465708079));
#38855=CARTESIAN_POINT('Ctrl Pts',(-3.87112305634801,-5.55349359238507,
122.003406226058));
#38856=CARTESIAN_POINT('Ctrl Pts',(-3.71567117317101,-5.65562346102231,
122.012155371326));
#38857=CARTESIAN_POINT('Ctrl Pts',(-3.56021980457712,-5.75775299158514,
122.020904487632));
#38858=CARTESIAN_POINT('Ctrl Pts',(-3.40055544862842,-5.85346967275088,
122.029653603938));
#38859=CARTESIAN_POINT('Ctrl Pts',(-3.23722036323902,-5.9424484280329,122.038402720244));
#38860=CARTESIAN_POINT('Ctrl Pts',(-3.07388580496566,-6.0314268961621,122.047151808315));
#38861=CARTESIAN_POINT('Ctrl Pts',(-2.90688079258247,-6.11366734484565,
122.055900896386));
#38862=CARTESIAN_POINT('Ctrl Pts',(-2.73677251095175,-6.18889046787054,
122.064649984457));
#38863=CARTESIAN_POINT('Ctrl Pts',(-2.56666476417232,-6.26411335438029,
122.073399045019));
#38864=CARTESIAN_POINT('Ctrl Pts',(-2.39345402972706,-6.33231884350058,
122.082148105581));
#38865=CARTESIAN_POINT('Ctrl Pts',(-2.21772856474678,-6.39327529620821,
122.090897166144));
#38866=CARTESIAN_POINT('Ctrl Pts',(-2.04200363768909,-6.45423156231879,
122.099646199924));
#38867=CARTESIAN_POINT('Ctrl Pts',(-1.86376426620732,-6.50793874251873,
122.108395233704));
#38868=CARTESIAN_POINT('Ctrl Pts',(-1.68361578195325,-6.55421443795959,
122.117144267484));
#38869=CARTESIAN_POINT('Ctrl Pts',(-1.50346783420507,-6.60048999558534,
122.125893275208));
#38870=CARTESIAN_POINT('Ctrl Pts',(-1.32141106257887,-6.63933404145368,
122.134642282932));
#38871=CARTESIAN_POINT('Ctrl Pts',(-1.13806375959685,-6.67061465526921,
122.143391290656));
#38872=CARTESIAN_POINT('Ctrl Pts',(-0.954716987425374,-6.70189517852392,
122.152140273051));
#38873=CARTESIAN_POINT('Ctrl Pts',(-0.770079973815904,-6.72561226535759,
122.160889255446));
#38874=CARTESIAN_POINT('Ctrl Pts',(-0.584779770558282,-6.74168536939732,
122.169638237841));
#38875=CARTESIAN_POINT('Ctrl Pts',(-0.391490647559712,-6.7584514394236,
122.178764418517));
#38876=CARTESIAN_POINT('Ctrl Pts',(-0.197480213110103,-6.7668997592401,
122.187890599193));
#38877=CARTESIAN_POINT('Ctrl Pts',(-0.00346532630352457,-6.76699911271707,
122.197016779869));
#38878=CARTESIAN_POINT('Ctrl Pts',(0.184486595290316,-6.76709536139789,
122.205857767399));
#38879=CARTESIAN_POINT('Ctrl Pts',(0.372442378179485,-6.75935659726802,
122.214698754929));
#38880=CARTESIAN_POINT('Ctrl Pts',(0.559750217716344,-6.74380965729064,
122.223539742459));
#38881=CARTESIAN_POINT('Ctrl Pts',(0.745129914452052,-6.72842275717317,
122.232289721057));
#38882=CARTESIAN_POINT('Ctrl Pts',(0.929874656308528,-6.70538772273551,
122.241039699655));
#38883=CARTESIAN_POINT('Ctrl Pts',(1.11335688289217,-6.67478280180836,122.249789678252));
#38884=CARTESIAN_POINT('Ctrl Pts',(1.29683723118301,-6.64417819418132,122.258539567277));
#38885=CARTESIAN_POINT('Ctrl Pts',(1.47905480729685,-6.60600390230198,122.267289456302));
#38886=CARTESIAN_POINT('Ctrl Pts',(1.65939064804263,-6.56038959797272,122.276039345327));
#38887=CARTESIAN_POINT('Ctrl Pts',(1.83972470263732,-6.51477574543407,122.284789147688));
#38888=CARTESIAN_POINT('Ctrl Pts',(2.01817678125327,-6.46172209820263,122.293538950049));
#38889=CARTESIAN_POINT('Ctrl Pts',(2.19414072347171,-6.40140886724189,122.30228875241));
#38890=CARTESIAN_POINT('Ctrl Pts',(2.37010298131591,-6.34109621361563,122.311038471016));
#38891=CARTESIAN_POINT('Ctrl Pts',(2.5435768792641,-6.27352420826175,122.319788189621));
#38892=CARTESIAN_POINT('Ctrl Pts',(2.71397317789472,-6.19892237325715,122.328537908226));
#38893=CARTESIAN_POINT('Ctrl Pts',(2.88436790206703,-6.12432122757198,122.337287545985));
#38894=CARTESIAN_POINT('Ctrl Pts',(3.05168482125761,-6.04269049717667,122.346037183743));
#38895=CARTESIAN_POINT('Ctrl Pts',(3.21535561996896,-5.95430745235196,122.354786821501));
#38896=CARTESIAN_POINT('Ctrl Pts',(3.37902496074785,-5.86592519481802,122.36353638132));
#38897=CARTESIAN_POINT('Ctrl Pts',(3.53904799384378,-5.77079087940536,122.372285941139));
#38898=CARTESIAN_POINT('Ctrl Pts',(3.69488118814487,-5.66922763747348,122.381035500958));
#38899=CARTESIAN_POINT('Ctrl Pts',(3.85071304610349,-5.56766526649387,122.389784985746));
#38900=CARTESIAN_POINT('Ctrl Pts',(4.00235489705497,-5.45967423581059,122.398534470533));
#38901=CARTESIAN_POINT('Ctrl Pts',(4.14929168607197,-5.34562133936683,122.407283955321));
#38902=CARTESIAN_POINT('Ctrl Pts',(4.29622726385302,-5.23156938308904,122.416033367984));
#38903=CARTESIAN_POINT('Ctrl Pts',(4.43845763091615,-5.11145583677594,122.424782780647));
#38904=CARTESIAN_POINT('Ctrl Pts',(4.57549970660514,-4.98568866204622,122.43353219331));
#38905=CARTESIAN_POINT('Ctrl Pts',(4.71254069814863,-4.8599224822658,122.442281536757));
#38906=CARTESIAN_POINT('Ctrl Pts',(4.84439326930898,-4.72850295734428,122.451030880203));
#38907=CARTESIAN_POINT('Ctrl Pts',(4.97060959434299,-4.59187644222114,122.459780223649));
#38908=CARTESIAN_POINT('Ctrl Pts',(5.09682496280126,-4.4552509625711,122.468529500786));
#38909=CARTESIAN_POINT('Ctrl Pts',(5.2174039761546,-4.31341878218784,122.477278777922));
#38910=CARTESIAN_POINT('Ctrl Pts',(5.33193710451566,-4.16686161439148,122.486028055058));
#38911=CARTESIAN_POINT('Ctrl Pts',(5.44646940289026,-4.02030550864997,122.494777268791));
#38912=CARTESIAN_POINT('Ctrl Pts',(5.5549557274932,-3.86902470980629,122.503526482524));
#38913=CARTESIAN_POINT('Ctrl Pts',(5.65702762491123,-3.71353301466289,122.512275696257));
#38914=CARTESIAN_POINT('Ctrl Pts',(5.75909881654838,-3.55804239467404,122.521024849493));
#38915=CARTESIAN_POINT('Ctrl Pts',(5.85475551250483,-3.39834117620068,122.529774002729));
#38916=CARTESIAN_POINT('Ctrl Pts',(5.94367283727813,-3.23497174692487,122.538523155966));
#38917=CARTESIAN_POINT('Ctrl Pts',(6.03258957676047,-3.07160339301485,122.547272251611));
#38918=CARTESIAN_POINT('Ctrl Pts',(6.11476689685037,-2.90456712830024,122.556021347257));
#38919=CARTESIAN_POINT('Ctrl Pts',(6.18992570525031,-2.73443024476425,122.564770442902));
#38920=CARTESIAN_POINT('Ctrl Pts',(6.26508404388496,-2.56429442463524,122.573519483863));
#38921=CARTESIAN_POINT('Ctrl Pts',(6.3332238428314,-2.3910582865646,122.582268524824));
#38922=CARTESIAN_POINT('Ctrl Pts',(6.39411368719881,-2.2153101713252,122.591017565785));
#38923=CARTESIAN_POINT('Ctrl Pts',(6.4550031712075,-2.03956309619958,122.599766554968));
#38924=CARTESIAN_POINT('Ctrl Pts',(6.50864269269945,-1.86130434439081,122.60851554415));
#38925=CARTESIAN_POINT('Ctrl Pts',(6.55485008446218,-1.68113930720396,122.617264533333));
#38926=CARTESIAN_POINT('Ctrl Pts',(6.60199664749303,-1.49731239212287,122.626191346862));
#38927=CARTESIAN_POINT('Ctrl Pts',(6.6414056364082,-1.31150116500113,122.635118160391));
#38928=CARTESIAN_POINT('Ctrl Pts',(6.67293772282099,-1.12436255156095,122.644044973921));
#38929=CARTESIAN_POINT('Ctrl Pts',(6.70384494949809,-0.94093239505575,122.652794888076));
#38930=CARTESIAN_POINT('Ctrl Pts',(6.7271844934888,-0.75622726051117,122.661544802232));
#38931=CARTESIAN_POINT('Ctrl Pts',(6.74287707373894,-0.57087456454619,122.670294716387));
#38932=CARTESIAN_POINT('Ctrl Pts',(6.75856934538644,-0.385525513637037,
122.679044458471));
#38933=CARTESIAN_POINT('Ctrl Pts',(6.76661493004089,-0.19952921242285,122.687794200555));
#38934=CARTESIAN_POINT('Ctrl Pts',(6.76698649908906,-0.0135174386051019,
122.696543942639));
#38935=CARTESIAN_POINT('Ctrl Pts',(6.76735806132401,0.172490924441081,122.705293524285));
#38936=CARTESIAN_POINT('Ctrl Pts',(6.76005588896314,0.358514472896692,122.714043105931));
#38937=CARTESIAN_POINT('Ctrl Pts',(6.74510478454622,0.543921359657485,122.722792687577));
#38938=CARTESIAN_POINT('Ctrl Pts',(6.73015393440739,0.729325093145684,122.731542120416));
#38939=CARTESIAN_POINT('Ctrl Pts',(6.70755443556962,0.914111900251564,122.740291553255));
#38940=CARTESIAN_POINT('Ctrl Pts',(6.67738304682398,1.09765415591057,122.749040986094));
#38941=CARTESIAN_POINT('Ctrl Pts',(6.64721213111951,1.28119353390805,122.757790281755));
#38942=CARTESIAN_POINT('Ctrl Pts',(6.60946960955595,1.46348811672198,122.766539577417));
#38943=CARTESIAN_POINT('Ctrl Pts',(6.56428366991293,1.6439187634778,122.775288873078));
#38944=CARTESIAN_POINT('Ctrl Pts',(6.5190983786784,1.82434682109278,122.784038043189));
#38945=CARTESIAN_POINT('Ctrl Pts',(6.46646995272056,2.0029107182001,122.7927872133));
#38946=CARTESIAN_POINT('Ctrl Pts',(6.40657713281696,2.17900400212273,122.80153638341));
#38947=CARTESIAN_POINT('Ctrl Pts',(6.34668509279217,2.35509499309234,122.810285439596));
#38948=CARTESIAN_POINT('Ctrl Pts',(6.27952894037694,2.52871516397704,122.819034495782));
#38949=CARTESIAN_POINT('Ctrl Pts',(6.20533675061626,2.69927486771008,122.827783551968));
#38950=CARTESIAN_POINT('Ctrl Pts',(6.12832117908101,2.87632521635532,122.83686555325));
#38951=CARTESIAN_POINT('Ctrl Pts',(6.04372366626267,3.05007728919627,122.845947554532));
#38952=CARTESIAN_POINT('Ctrl Pts',(5.95185378008057,3.21989527477846,122.855029555815));
#38953=CARTESIAN_POINT('Ctrl Pts',(5.86334450817571,3.38350129286406,122.863779336122));
#38954=CARTESIAN_POINT('Ctrl Pts',(5.76808562057466,3.54345567124619,122.872529116429));
#38955=CARTESIAN_POINT('Ctrl Pts',(5.66640068804705,3.69921508464971,122.881278896736));
#38956=CARTESIAN_POINT('Ctrl Pts',(5.56471941108155,3.85496889851948,122.890028362489));
#38957=CARTESIAN_POINT('Ctrl Pts',(5.45661270815357,4.00652780919305,122.898777828243));
#38958=CARTESIAN_POINT('Ctrl Pts',(5.34244776449369,4.15337704568901,122.907527293996));
#38959=CARTESIAN_POINT('Ctrl Pts',(5.22828631819858,4.3002217835593,122.916276491716));
#38960=CARTESIAN_POINT('Ctrl Pts',(5.1080671784434,4.44235690972368,122.925025689436));
#38961=CARTESIAN_POINT('Ctrl Pts',(4.98219864544997,4.57929969070342,122.933774887155));
#38962=CARTESIAN_POINT('Ctrl Pts',(4.85633329944311,4.71623900429707,122.942523863345));
#38963=CARTESIAN_POINT('Ctrl Pts',(4.72481904033941,4.84798602483331,122.951272839536));
#38964=CARTESIAN_POINT('Ctrl Pts',(4.58810250737498,4.97409332258849,122.960021815726));
#38965=CARTESIAN_POINT('Ctrl Pts',(4.45137708685942,5.10020881821873,122.968771360662));
#38966=CARTESIAN_POINT('Ctrl Pts',(4.30944892636351,5.22068366307686,122.977520905598));
#38967=CARTESIAN_POINT('Ctrl Pts',(4.16280009466959,5.33510865604618,122.986270450534));
#38968=CARTESIAN_POINT('Ctrl Pts',(4.01615988349087,5.44952692272672,122.995019481143));
#38969=CARTESIAN_POINT('Ctrl Pts',(3.8647997823253,5.55789587288419,123.003768511751));
#38970=CARTESIAN_POINT('Ctrl Pts',(3.70923383581366,5.65984746713682,123.012517542359));
#38971=CARTESIAN_POINT('Ctrl Pts',(3.55366577799845,5.76180044505195,123.021266691707));
#38972=CARTESIAN_POINT('Ctrl Pts',(3.3938920002715,5.85733573570879,123.030015841055));
#38973=CARTESIAN_POINT('Ctrl Pts',(3.23045513626356,5.94612887621757,123.038764990403));
#38974=CARTESIAN_POINT('Ctrl Pts',(3.18695122151793,5.96976399206575,123.041093854516));
#38975=CARTESIAN_POINT('Ctrl Pts',(3.14318791262776,5.99292165435275,123.043422718629));
#38976=CARTESIAN_POINT('Ctrl Pts',(3.09917575053267,6.01559628526635,123.045751582742));
#38977=CARTESIAN_POINT('Ctrl Pts',(3.09917575053254,6.01559628526642,121.045781922714));
#38978=CARTESIAN_POINT('Ctrl Pts',(2.94377814450788,6.0956555960054,121.053981099718));
#38979=CARTESIAN_POINT('Ctrl Pts',(2.78526454007982,6.16969567928123,121.062180276722));
#38980=CARTESIAN_POINT('Ctrl Pts',(2.62414456692463,6.23747980292361,121.070379453726));
#38981=CARTESIAN_POINT('Ctrl Pts',(2.46300343222845,6.30527282935118,121.078579707612));
#38982=CARTESIAN_POINT('Ctrl Pts',(2.29925557718677,6.36680811987964,121.086779961498));
#38983=CARTESIAN_POINT('Ctrl Pts',(2.13343027031341,6.42189724938904,121.094980215385));
#38984=CARTESIAN_POINT('Ctrl Pts',(1.96755310133998,6.47700360810187,121.103183033912));
#38985=CARTESIAN_POINT('Ctrl Pts',(1.79959752632693,6.52565967670675,121.111385852439));
#38986=CARTESIAN_POINT('Ctrl Pts',(1.63010766546976,6.56772700399284,121.119588670966));
#38987=CARTESIAN_POINT('Ctrl Pts',(1.45349391549002,6.61156247819789,121.1281362651));
#38988=CARTESIAN_POINT('Ctrl Pts',(1.27521453189092,6.64824324314782,121.136683859235));
#38989=CARTESIAN_POINT('Ctrl Pts',(1.09589560549116,6.67767188635869,121.145231453369));
#38990=CARTESIAN_POINT('Ctrl Pts',(0.923515546466782,6.70596176827772,121.153448292556));
#38991=CARTESIAN_POINT('Ctrl Pts',(0.750175246529651,6.72755026350163,121.161665131743));
#38992=CARTESIAN_POINT('Ctrl Pts',(0.576434595129533,6.74240403398802,121.16988197093));
#38993=CARTESIAN_POINT('Ctrl Pts',(0.402568471726121,6.75726853156864,121.178104744153));
#38994=CARTESIAN_POINT('Ctrl Pts',(0.228301777134898,6.76538859449395,121.186327517375));
#38995=CARTESIAN_POINT('Ctrl Pts',(0.0541937887683528,6.76678298996347,
121.194550290598));
#38996=CARTESIAN_POINT('Ctrl Pts',(-0.120146997815844,6.76817924986657,
121.202784058417));
#38997=CARTESIAN_POINT('Ctrl Pts',(-0.294328298351081,6.76283190029155,
121.211017826235));
#38998=CARTESIAN_POINT('Ctrl Pts',(-0.467795785605221,6.75081151440107,
121.219251594054));
#38999=CARTESIAN_POINT('Ctrl Pts',(-0.488218970115628,6.74939629496823,
121.220220996229));
#39000=CARTESIAN_POINT('Ctrl Pts',(-0.508632271863779,6.74788863533063,
121.221190398403));
#39001=CARTESIAN_POINT('Ctrl Pts',(-0.529034796293258,6.74628869707715,
121.222159800578));
#39002=CARTESIAN_POINT('Ctrl Pts',(-0.700645700907447,6.73283120303253,
121.230313692745));
#39003=CARTESIAN_POINT('Ctrl Pts',(-0.872023887206462,6.7127992772155,121.238467584911));
#39004=CARTESIAN_POINT('Ctrl Pts',(-1.04262025750242,6.68619712532061,121.246621477078));
#39005=CARTESIAN_POINT('Ctrl Pts',(-1.21300845256476,6.65962743548324,121.254765419218));
#39006=CARTESIAN_POINT('Ctrl Pts',(-1.38261637336091,6.62650353435076,121.262909361359));
#39007=CARTESIAN_POINT('Ctrl Pts',(-1.55089657585776,6.58688156952838,121.271053303499));
#39008=CARTESIAN_POINT('Ctrl Pts',(-1.71900684911815,6.54729961493971,121.279189021892));
#39009=CARTESIAN_POINT('Ctrl Pts',(-1.88579171996496,6.50123274296745,121.287324740285));
#39010=CARTESIAN_POINT('Ctrl Pts',(-2.05071051547285,6.4487886755366,121.295460458677));
#39011=CARTESIAN_POINT('Ctrl Pts',(-2.2154974667992,6.39638653446791,121.303589672978));
#39012=CARTESIAN_POINT('Ctrl Pts',(-2.37842096635326,6.33761745936685,121.311718887278));
#39013=CARTESIAN_POINT('Ctrl Pts',(-2.53895216831899,6.27263986587691,121.319848101578));
#39014=CARTESIAN_POINT('Ctrl Pts',(-2.69938878743832,6.20770055631975,121.327972526253));
#39015=CARTESIAN_POINT('Ctrl Pts',(-2.85743557786453,6.13656014993194,121.336096950929));
#39016=CARTESIAN_POINT('Ctrl Pts',(-3.01258046364437,6.05942637137117,121.344221375604));
#39017=CARTESIAN_POINT('Ctrl Pts',(-3.16866717820063,5.98182434139548,121.352395120738));
#39018=CARTESIAN_POINT('Ctrl Pts',(-3.32181628228949,5.89815604766954,121.360568865872));
#39019=CARTESIAN_POINT('Ctrl Pts',(-3.47152777146921,5.80868177230583,121.368742611006));
#39020=CARTESIAN_POINT('Ctrl Pts',(-3.620280552081,5.71978046401948,121.376864013869));
#39021=CARTESIAN_POINT('Ctrl Pts',(-3.76563931006539,5.62514752606199,121.384985416731));
#39022=CARTESIAN_POINT('Ctrl Pts',(-3.90713957320407,5.52508365144843,121.393106819593));
#39023=CARTESIAN_POINT('Ctrl Pts',(-4.04865077639776,5.42501204042317,121.401228850359));
#39024=CARTESIAN_POINT('Ctrl Pts',(-4.18630259167283,5.31950886763514,121.409350881125));
#39025=CARTESIAN_POINT('Ctrl Pts',(-4.31966097371313,5.20891716887299,121.417472911892));
#39026=CARTESIAN_POINT('Ctrl Pts',(-4.45305506083704,5.09829586052956,121.425597117233));
#39027=CARTESIAN_POINT('Ctrl Pts',(-4.58215314423595,4.98258354697544,121.433721322574));
#39028=CARTESIAN_POINT('Ctrl Pts',(-4.70655564283561,4.86216237705944,121.441845527915));
#39029=CARTESIAN_POINT('Ctrl Pts',(-4.83230471240292,4.74043773130393,121.450057672157));
#39030=CARTESIAN_POINT('Ctrl Pts',(-4.95325567413202,4.6139019596473,121.4582698164));
#39031=CARTESIAN_POINT('Ctrl Pts',(-5.06903596436854,4.4829859906025,121.466481960642));
#39032=CARTESIAN_POINT('Ctrl Pts',(-5.18375930816161,4.353265140067,121.474619137059));
#39033=CARTESIAN_POINT('Ctrl Pts',(-5.2934058099648,4.21924405500319,121.482756313475));
#39034=CARTESIAN_POINT('Ctrl Pts',(-5.39765548183425,4.08137284494135,121.490893489892));
#39035=CARTESIAN_POINT('Ctrl Pts',(-5.50334583242183,3.94159632319252,121.499143118047));
#39036=CARTESIAN_POINT('Ctrl Pts',(-5.60348887338751,3.79786280554131,121.507392746203));
#39037=CARTESIAN_POINT('Ctrl Pts',(-5.69779850792845,3.65066859123754,121.515642374358));
#39038=CARTESIAN_POINT('Ctrl Pts',(-5.79210814246933,3.50347437693388,121.523892002513));
#39039=CARTESIAN_POINT('Ctrl Pts',(-5.8805842302813,3.35281982980438,121.532141630669));
#39040=CARTESIAN_POINT('Ctrl Pts',(-5.96299075072147,3.1992233912014,121.540391258824));
#39041=CARTESIAN_POINT('Ctrl Pts',(-6.05007866566296,3.03690136244782,121.54910953635));
#39042=CARTESIAN_POINT('Ctrl Pts',(-6.13062359919724,2.87085576499492,121.557827813875));
#39043=CARTESIAN_POINT('Ctrl Pts',(-6.2043141710099,2.70162444973497,121.566546091401));
#39044=CARTESIAN_POINT('Ctrl Pts',(-6.2778836205095,2.53267129337434,121.575250039034));
#39045=CARTESIAN_POINT('Ctrl Pts',(-6.34462105769029,2.36054312842015,121.583953986667));
#39046=CARTESIAN_POINT('Ctrl Pts',(-6.40426083818913,2.18580239647528,121.592657934301));
#39047=CARTESIAN_POINT('Ctrl Pts',(-6.46394314581031,2.01093706278939,121.601368088426));
#39048=CARTESIAN_POINT('Ctrl Pts',(-6.51651750873807,1.83345568667579,121.610078242552));
#39049=CARTESIAN_POINT('Ctrl Pts',(-6.56176449452805,1.65394550041742,121.618788396678));
#39050=CARTESIAN_POINT('Ctrl Pts',(-6.60680989005414,1.47523509131964,121.627459744191));
#39051=CARTESIAN_POINT('Ctrl Pts',(-6.6445929576778,1.29451418989422,121.636131091703));
#39052=CARTESIAN_POINT('Ctrl Pts',(-6.6749454105017,1.1123815742911,121.644802439216));
#39053=CARTESIAN_POINT('Ctrl Pts',(-6.70550161641409,0.929026320005028,
121.653531996648));
#39054=CARTESIAN_POINT('Ctrl Pts',(-6.72852694174223,0.744240600378212,
121.662261554081));
#39055=CARTESIAN_POINT('Ctrl Pts',(-6.74390080922855,0.558650942258707,
121.670991111513));
#39056=CARTESIAN_POINT('Ctrl Pts',(-6.75927467671487,0.373061284139074,
121.679720668945));
#39057=CARTESIAN_POINT('Ctrl Pts',(-6.7669969978568,0.186667984783223,121.688450226378));
#39058=CARTESIAN_POINT('Ctrl Pts',(-6.76699999912433,0.000108864028085915,
121.69717978381));
#39059=CARTESIAN_POINT('',(-6.76699876671586,-0.00266907362020019,121.30282021619));
#39060=CARTESIAN_POINT('Ctrl Pts',(3.09917575053273,6.01559628526632,120.651392015122));
#39061=CARTESIAN_POINT('Ctrl Pts',(2.9338238445927,6.10078395293757,120.660141463035));
#39062=CARTESIAN_POINT('Ctrl Pts',(2.76495772122981,6.17915010267051,120.668890910947));
#39063=CARTESIAN_POINT('Ctrl Pts',(2.59315093316699,6.25042856433183,120.67764035886));
#39064=CARTESIAN_POINT('Ctrl Pts',(2.42134553245594,6.3217064504146,120.68638973612));
#39065=CARTESIAN_POINT('Ctrl Pts',(2.24659977927557,6.38589665313469,120.69513911338));
#39066=CARTESIAN_POINT('Ctrl Pts',(2.06950718689874,6.44278115439089,120.70388849064));
#39067=CARTESIAN_POINT('Ctrl Pts',(1.89241596572818,6.49966521519736,120.712637800154));
#39068=CARTESIAN_POINT('Ctrl Pts',(1.71297821457156,6.54924360009557,120.721387109669));
#39069=CARTESIAN_POINT('Ctrl Pts',(1.53180337335804,6.59134792173565,120.730136419184));
#39070=CARTESIAN_POINT('Ctrl Pts',(1.35062987477738,6.63345193135314,120.73888566386));
#39071=CARTESIAN_POINT('Ctrl Pts',(1.16771959102903,6.66808192368246,120.747634908536));
#39072=CARTESIAN_POINT('Ctrl Pts',(0.983693746906317,6.69512028363176,120.756384153212));
#39073=CARTESIAN_POINT('Ctrl Pts',(0.799669205419294,6.72215845218874,120.765133335956));
#39074=CARTESIAN_POINT('Ctrl Pts',(0.614529402872849,6.74160505424585,120.7738825187));
#39075=CARTESIAN_POINT('Ctrl Pts',(0.428903127362573,6.75339404354126,120.782631701445));
#39076=CARTESIAN_POINT('Ctrl Pts',(0.243278104163051,6.76518295330334,120.791380825163));
#39077=CARTESIAN_POINT('Ctrl Pts',(0.0571669005381381,6.76931433552277,
120.800129948882));
#39078=CARTESIAN_POINT('Ctrl Pts',(-0.128798404778644,6.76577415902471,
120.8088790726));
#39079=CARTESIAN_POINT('Ctrl Pts',(-0.31476251726011,6.76223400523436,120.8176281402));
#39080=CARTESIAN_POINT('Ctrl Pts',(-0.500580446820403,6.75102239665082,
120.826377207799));
#39081=CARTESIAN_POINT('Ctrl Pts',(-0.685621118843384,6.7321774101249,120.835126275398));
#39082=CARTESIAN_POINT('Ctrl Pts',(-0.87066066541513,6.71333253821763,120.843875289784));
#39083=CARTESIAN_POINT('Ctrl Pts',(-1.05492267885538,6.68685441030604,120.85262430417));
#39084=CARTESIAN_POINT('Ctrl Pts',(-1.2377813763529,6.6528329502817,120.861373318555));
#39085=CARTESIAN_POINT('Ctrl Pts',(-1.42999922978874,6.61707018861859,120.870570128923));
#39086=CARTESIAN_POINT('Ctrl Pts',(-1.62066601233712,6.57297172934408,120.87976693929));
#39087=CARTESIAN_POINT('Ctrl Pts',(-1.80906628500392,6.52070304311292,120.888963749658));
#39088=CARTESIAN_POINT('Ctrl Pts',(-1.98831342545526,6.47097374915031,120.897713747395));
#39089=CARTESIAN_POINT('Ctrl Pts',(-2.16550875896692,6.41384933989531,120.906463745133));
#39090=CARTESIAN_POINT('Ctrl Pts',(-2.34005036713994,6.34952386240482,120.915213742871));
#39091=CARTESIAN_POINT('Ctrl Pts',(-2.51458843547075,6.28519968948602,120.923963563152));
#39092=CARTESIAN_POINT('Ctrl Pts',(-2.68647261718045,6.21367483971104,120.932713383433));
#39093=CARTESIAN_POINT('Ctrl Pts',(-2.85511905908723,6.13519226743847,120.941463203713));
#39094=CARTESIAN_POINT('Ctrl Pts',(-3.02376230488874,6.05671118252942,120.950212858172));
#39095=CARTESIAN_POINT('Ctrl Pts',(-3.18916767379892,5.97127275992639,120.95896251263));
#39096=CARTESIAN_POINT('Ctrl Pts',(-3.35077334102773,5.87916720438005,120.967712167089));
#39097=CARTESIAN_POINT('Ctrl Pts',(-3.51237616037354,5.78706327195651,120.976461667357));
#39098=CARTESIAN_POINT('Ctrl Pts',(-3.67017916302287,5.68829258362307,120.985211167626));
#39099=CARTESIAN_POINT('Ctrl Pts',(-3.8236463656645,5.5831906174105,120.993960667894));
#39100=CARTESIAN_POINT('Ctrl Pts',(-3.97711106778785,5.47809036367711,121.002710025603));
#39101=CARTESIAN_POINT('Ctrl Pts',(-4.12623987481913,5.36665920043236,121.011459383311));
#39102=CARTESIAN_POINT('Ctrl Pts',(-4.27052628213915,5.24927559512347,121.02020874102));
#39103=CARTESIAN_POINT('Ctrl Pts',(-4.41481053024973,5.13189374643041,121.028957967796));
#39104=CARTESIAN_POINT('Ctrl Pts',(-4.55425230136534,5.0085598147735,121.037707194573));
#39105=CARTESIAN_POINT('Ctrl Pts',(-4.6883780063056,4.87969268192065,121.046456421349));
#39106=CARTESIAN_POINT('Ctrl Pts',(-4.82250188228906,4.75082730631798,121.05520552882));
#39107=CARTESIAN_POINT('Ctrl Pts',(-4.95130963052977,4.61642907903514,121.063954636291));
#39108=CARTESIAN_POINT('Ctrl Pts',(-5.07436379033377,4.47695444731678,121.072703743762));
#39109=CARTESIAN_POINT('Ctrl Pts',(-5.19741643562825,4.33748153220563,121.081452743552));
#39110=CARTESIAN_POINT('Ctrl Pts',(-5.31471544462801,4.19293255254554,121.090201743341));
#39111=CARTESIAN_POINT('Ctrl Pts',(-5.42586245275663,4.04379841779555,121.098950743131));
#39112=CARTESIAN_POINT('Ctrl Pts',(-5.53702160019175,3.8946479948431,121.107700698473));
#39113=CARTESIAN_POINT('Ctrl Pts',(-5.64202723081262,3.74091164443833,121.116450653815));
#39114=CARTESIAN_POINT('Ctrl Pts',(-5.74052265232967,3.58311159163232,121.125200609157));
#39115=CARTESIAN_POINT('Ctrl Pts',(-5.8390142706692,3.4253176319178,121.13395022664));
#39116=CARTESIAN_POINT('Ctrl Pts',(-5.93099603115743,3.26346052695607,121.142699844122));
#39117=CARTESIAN_POINT('Ctrl Pts',(-6.01615550622758,3.09809004467068,121.151449461605));
#39118=CARTESIAN_POINT('Ctrl Pts',(-6.10131214578807,2.93272506863812,121.160198787756));
#39119=CARTESIAN_POINT('Ctrl Pts',(-6.17964682328758,2.76384720416872,121.168948113907));
#39120=CARTESIAN_POINT('Ctrl Pts',(-6.25089348288576,2.59203002791563,121.177697440058));
#39121=CARTESIAN_POINT('Ctrl Pts',(-6.32213814889348,2.42021765936983,121.18644652139));
#39122=CARTESIAN_POINT('Ctrl Pts',(-6.38629508412607,2.24546640831856,121.195195602721));
#39123=CARTESIAN_POINT('Ctrl Pts',(-6.44314639819837,2.06836976659963,121.203944684053));
#39124=CARTESIAN_POINT('Ctrl Pts',(-6.50000285283727,1.89125711158184,121.212694556487));
#39125=CARTESIAN_POINT('Ctrl Pts',(-6.54955227673277,1.71179891440149,121.221444428922));
#39126=CARTESIAN_POINT('Ctrl Pts',(-6.59162635926413,1.53060476278312,121.230194301356));
#39127=CARTESIAN_POINT('Ctrl Pts',(-6.63369752055219,1.34942319164583,121.238943566279));
#39128=CARTESIAN_POINT('Ctrl Pts',(-6.66829431424272,1.16650618642598,121.247692831201));
#39129=CARTESIAN_POINT('Ctrl Pts',(-6.69529923745432,0.982474997617564,
121.256442096124));
#39130=CARTESIAN_POINT('Ctrl Pts',(-6.72230554731455,0.798434359176729,
121.265191810303));
#39131=CARTESIAN_POINT('Ctrl Pts',(-6.74171916496712,0.613279706239307,
121.273941524483));
#39132=CARTESIAN_POINT('Ctrl Pts',(-6.75347414817282,0.427639953654331,
121.282691238663));
#39133=CARTESIAN_POINT('Ctrl Pts',(-6.76248837758734,0.285283364199802,
121.289400897838));
#39134=CARTESIAN_POINT('Ctrl Pts',(-6.76699999999985,0.142641701108631,
121.296110557014));
#39135=CARTESIAN_POINT('Ctrl Pts',(-6.767,7.36526836825673E-12,121.30282021619));
#39136=CARTESIAN_POINT('Ctrl Pts',(-6.76699711044301,-0.00625357945092592,
121.30282021619));
#39137=CARTESIAN_POINT('Ctrl Pts',(-6.7667990677175,-0.220555574302487,
121.312887263886));
#39138=CARTESIAN_POINT('Ctrl Pts',(-6.75641746286505,-0.434393464847247,
121.322954311582));
#39139=CARTESIAN_POINT('Ctrl Pts',(-6.73600616481901,-0.64692344795989,
121.333021359278));
#39140=CARTESIAN_POINT('Ctrl Pts',(-6.71538293818884,-0.861660109859227,
121.343192932182));
#39141=CARTESIAN_POINT('Ctrl Pts',(-6.68452074611038,-1.07506164536285,
121.353364505086));
#39142=CARTESIAN_POINT('Ctrl Pts',(-6.64362620636337,-1.28628139616565,
121.363536077989));
#39143=CARTESIAN_POINT('Ctrl Pts',(-6.60229775646945,-1.49974228707341,
121.373815576027));
#39144=CARTESIAN_POINT('Ctrl Pts',(-6.55072295034635,-1.71097494008967,
121.384095074065));
#39145=CARTESIAN_POINT('Ctrl Pts',(-6.48916295838299,-1.91912821342145,
121.394374572103));
#39146=CARTESIAN_POINT('Ctrl Pts',(-6.47633796933195,-1.96249344733842,
121.396516132646));
#39147=CARTESIAN_POINT('Ctrl Pts',(-6.46307976012568,-2.00572510299209,
121.398657693188));
#39148=CARTESIAN_POINT('Ctrl Pts',(-6.44939095057919,-2.04881560092343,
121.400799253731));
#39149=CARTESIAN_POINT('Ctrl Pts',(-6.39726143349232,-2.21291218219047,
121.408954712138));
#39150=CARTESIAN_POINT('Ctrl Pts',(-6.33877995666408,-2.37528556587604,
121.417110170545));
#39151=CARTESIAN_POINT('Ctrl Pts',(-6.2740757464106,-2.5354018474992,121.425265628951));
#39152=CARTESIAN_POINT('Ctrl Pts',(-6.20945028968617,-2.69532324656078,
121.433411161093));
#39153=CARTESIAN_POINT('Ctrl Pts',(-6.13861731113867,-2.85299267681184,
121.441556693235));
#39154=CARTESIAN_POINT('Ctrl Pts',(-6.06175623643756,-3.00788968049202,
121.449702225377));
#39155=CARTESIAN_POINT('Ctrl Pts',(-5.98497254942552,-3.16263072589024,
121.457839556178));
#39156=CARTESIAN_POINT('Ctrl Pts',(-5.90217301060363,-3.3146045769819,121.465976886978));
#39157=CARTESIAN_POINT('Ctrl Pts',(-5.81358572146447,-3.46330911978478,
121.474114217779));
#39158=CARTESIAN_POINT('Ctrl Pts',(-5.72506900967825,-3.61189518991396,
121.482245065581));
#39159=CARTESIAN_POINT('Ctrl Pts',(-5.63077391502269,-3.75721682539706,
121.490375913383));
#39160=CARTESIAN_POINT('Ctrl Pts',(-5.53097520618648,-3.89879497647035,
121.498506761185));
#39161=CARTESIAN_POINT('Ctrl Pts',(-5.43123504237683,-4.04029007339683,
121.506632839179));
#39162=CARTESIAN_POINT('Ctrl Pts',(-5.32599790411775,-4.1780457613,121.514758917172));
#39163=CARTESIAN_POINT('Ctrl Pts',(-5.21558275402377,-4.31161055012275,
121.522884995166));
#39164=CARTESIAN_POINT('Ctrl Pts',(-5.10477609197409,-4.44564893529203,
121.531039886748));
#39165=CARTESIAN_POINT('Ctrl Pts',(-4.98875482570804,-4.57546633021193,
121.539194778331));
#39166=CARTESIAN_POINT('Ctrl Pts',(-4.86788353512265,-4.70063813630467,
121.547349669913));
#39167=CARTESIAN_POINT('Ctrl Pts',(-4.74748360030912,-4.8253218161187,121.555472760269));
#39168=CARTESIAN_POINT('Ctrl Pts',(-4.6222716682509,-4.94539582134728,121.563595850625));
#39169=CARTESIAN_POINT('Ctrl Pts',(-4.49264629704856,-5.0604760892248,121.571718940982));
#39170=CARTESIAN_POINT('Ctrl Pts',(-4.36301074707036,-5.17556539373026,
121.5798426692));
#39171=CARTESIAN_POINT('Ctrl Pts',(-4.22896134117997,-5.28565993689408,
121.587966397419));
#39172=CARTESIAN_POINT('Ctrl Pts',(-4.09093095177298,-5.39041491425529,
121.596090125637));
#39173=CARTESIAN_POINT('Ctrl Pts',(-3.9528634634716,-5.4951980469659,121.604216037297));
#39174=CARTESIAN_POINT('Ctrl Pts',(-3.8108131524038,-5.59463853519105,121.612341948958));
#39175=CARTESIAN_POINT('Ctrl Pts',(-3.66524314378872,-5.68843402852752,
121.620467860618));
#39176=CARTESIAN_POINT('Ctrl Pts',(-3.51874219983684,-5.78282935379372,
121.628645738328));
#39177=CARTESIAN_POINT('Ctrl Pts',(-3.36867670015287,-5.8715070294679,121.636823616038));
#39178=CARTESIAN_POINT('Ctrl Pts',(-3.21554448135241,-5.95420546239749,
121.645001493748));
#39179=CARTESIAN_POINT('Ctrl Pts',(-3.06314312941981,-6.03650919364296,
121.653140340222));
#39180=CARTESIAN_POINT('Ctrl Pts',(-2.90770462327633,-6.11289052619905,
121.661279186695));
#39181=CARTESIAN_POINT('Ctrl Pts',(-2.74974009032668,-6.18313985250619,
121.669418033168));
#39182=CARTESIAN_POINT('Ctrl Pts',(-2.59063923828957,-6.25389451788453,
121.677615426497));
#39183=CARTESIAN_POINT('Ctrl Pts',(-2.42897623128213,-6.31842848308074,
121.685812819825));
#39184=CARTESIAN_POINT('Ctrl Pts',(-2.26528877975034,-6.37657868643815,
121.694010213154));
#39185=CARTESIAN_POINT('Ctrl Pts',(-2.10160132821855,-6.43472888979555,
121.702207606482));
#39186=CARTESIAN_POINT('Ctrl Pts',(-1.93588980568439,-6.48649527865371,
121.71040499981));
#39187=CARTESIAN_POINT('Ctrl Pts',(-1.768701904929,-6.53176718595363,121.718602393139));
#39188=CARTESIAN_POINT('Ctrl Pts',(-1.60092629442354,-6.57719823599775,
121.726828602476));
#39189=CARTESIAN_POINT('Ctrl Pts',(-1.4311646085969,-6.61622438915903,121.735054811813));
#39190=CARTESIAN_POINT('Ctrl Pts',(-1.25994680357312,-6.64867077333251,
121.74328102115));
#39191=CARTESIAN_POINT('Ctrl Pts',(-1.0889213544183,-6.68108070538337,121.751497988693));
#39192=CARTESIAN_POINT('Ctrl Pts',(-0.916443392727803,-6.70692552193531,
121.759714956236));
#39193=CARTESIAN_POINT('Ctrl Pts',(-0.743057841187611,-6.72608013962439,
121.767931923779));
#39194=CARTESIAN_POINT('Ctrl Pts',(-0.569832281017914,-6.74521708240625,
121.776141309123));
#39195=CARTESIAN_POINT('Ctrl Pts',(-0.395701153094108,-6.75767608169907,
121.784350694466));
#39196=CARTESIAN_POINT('Ctrl Pts',(-0.221219470160394,-6.76338309916139,
121.792560079809));
#39197=CARTESIAN_POINT('Ctrl Pts',(-0.0468637814196446,-6.76908599555469,
121.80076353711));
#39198=CARTESIAN_POINT('Ctrl Pts',(0.127841601131879,-6.76804660988572,
121.808966994411));
#39199=CARTESIAN_POINT('Ctrl Pts',(0.302336551891229,-6.76024271823065,
121.817170451711));
#39200=CARTESIAN_POINT('Ctrl Pts',(0.476740502135301,-6.75244289636763,
121.825369630843));
#39201=CARTESIAN_POINT('Ctrl Pts',(0.650933881786635,-6.73788561239784,
121.833568809975));
#39202=CARTESIAN_POINT('Ctrl Pts',(0.824356481458405,-6.716600731879,121.841767989107));
#39203=CARTESIAN_POINT('Ctrl Pts',(0.997746404574913,-6.69531986189037,
121.849965623337));
#39204=CARTESIAN_POINT('Ctrl Pts',(1.17036548064243,-6.66731395780021,121.858163257566));
#39205=CARTESIAN_POINT('Ctrl Pts',(1.34165822783221,-6.63266478873237,121.866360891796));
#39206=CARTESIAN_POINT('Ctrl Pts',(1.51293861092379,-6.59801812067951,121.874557934312));
#39207=CARTESIAN_POINT('Ctrl Pts',(1.68289250406754,-6.55672921288288,121.882754976827));
#39208=CARTESIAN_POINT('Ctrl Pts',(1.8509742857312,-6.50893103309306,121.890952019343));
#39209=CARTESIAN_POINT('Ctrl Pts',(2.01907448365012,-6.46112761618907,121.899149959986));
#39210=CARTESIAN_POINT('Ctrl Pts',(2.18530181635332,-6.40681360451515,121.907347900629));
#39211=CARTESIAN_POINT('Ctrl Pts',(2.34912545074222,-6.34617196557698,121.915545841271));
#39212=CARTESIAN_POINT('Ctrl Pts',(2.51299680961457,-6.28551266074521,121.923746170107));
#39213=CARTESIAN_POINT('Ctrl Pts',(2.67446273909679,-6.21852218142059,121.931946498943));
#39214=CARTESIAN_POINT('Ctrl Pts',(2.83301197825863,-6.14543180997423,121.940146827779));
#39215=CARTESIAN_POINT('Ctrl Pts',(2.99172642984156,-6.07226527646434,121.948355701571));
#39216=CARTESIAN_POINT('Ctrl Pts',(3.14751779294393,-5.99298630237409,121.956564575362));
#39217=CARTESIAN_POINT('Ctrl Pts',(3.29989814603073,-5.90787281733646,121.964773449153));
#39218=CARTESIAN_POINT('Ctrl Pts',(3.45236027997206,-5.82271365283032,121.972986728557));
#39219=CARTESIAN_POINT('Ctrl Pts',(3.60140744859456,-5.73171392171152,121.98120000796));
#39220=CARTESIAN_POINT('Ctrl Pts',(3.74658047352514,-5.63519509470614,121.989413287364));
#39221=CARTESIAN_POINT('Ctrl Pts',(3.89196583682183,-5.5385350937462,121.997638579979));
#39222=CARTESIAN_POINT('Ctrl Pts',(4.03346544145236,-5.43634007443489,122.005863872595));
#39223=CARTESIAN_POINT('Ctrl Pts',(4.17065196527354,-5.32897280763938,122.01408916521));
#39224=CARTESIAN_POINT('Ctrl Pts',(4.2947206966164,-5.23187201225489,122.021527954322));
#39225=CARTESIAN_POINT('Ctrl Pts',(4.41526204542133,-5.13054146037317,122.028966743434));
#39226=CARTESIAN_POINT('Ctrl Pts',(4.53198638129172,-5.0252749616102,122.036405532546));
#39227=CARTESIAN_POINT('Ctrl Pts',(4.66106624041878,-4.908865776415,122.044631733565));
#39228=CARTESIAN_POINT('Ctrl Pts',(4.78583848198063,-4.78731734698028,122.052857934584));
#39229=CARTESIAN_POINT('Ctrl Pts',(4.90586901710682,-4.66098038903742,122.061084135603));
#39230=CARTESIAN_POINT('Ctrl Pts',(5.02576472322457,-4.53478534403988,122.069301096219));
#39231=CARTESIAN_POINT('Ctrl Pts',(5.1409290842546,-4.40381273903107,122.077518056834));
#39232=CARTESIAN_POINT('Ctrl Pts',(5.2509617530061,-4.26845284247901,122.08573501745));
#39233=CARTESIAN_POINT('Ctrl Pts',(5.36089290767535,-4.13321782643586,122.093944397252));
#39234=CARTESIAN_POINT('Ctrl Pts',(5.46570157400974,-3.9936038564033,122.102153777053));
#39235=CARTESIAN_POINT('Ctrl Pts',(5.56502484426122,-3.85003733524175,122.110363156855));
#39236=CARTESIAN_POINT('Ctrl Pts',(5.66427640929441,-3.70657446017152,122.118566609995));
#39237=CARTESIAN_POINT('Ctrl Pts',(5.75805026289624,-3.55916501138617,122.126770063136));
#39238=CARTESIAN_POINT('Ctrl Pts',(5.8460242798256,-3.40826775938887,122.134973516276));
#39239=CARTESIAN_POINT('Ctrl Pts',(5.93395243235963,-3.25744917620151,122.143172692626));
#39240=CARTESIAN_POINT('Ctrl Pts',(6.01608659174577,-3.10314672133383,122.151371868976));
#39241=CARTESIAN_POINT('Ctrl Pts',(6.09214837090922,-2.94584745477903,122.159571045326));
#39242=CARTESIAN_POINT('Ctrl Pts',(6.16819583790101,-2.78857778645518,122.167768678878));
#39243=CARTESIAN_POINT('Ctrl Pts',(6.23817303906425,-2.62831274949341,122.175966312429));
#39244=CARTESIAN_POINT('Ctrl Pts',(6.30184777566054,-2.46556354864407,122.184163945981));
#39245=CARTESIAN_POINT('Ctrl Pts',(6.36551792611308,-2.3028260697314,122.192360989101));
#39246=CARTESIAN_POINT('Ctrl Pts',(6.42288638452119,-2.13760511696331,122.200558032222));
#39247=CARTESIAN_POINT('Ctrl Pts',(6.4737693286473,-1.97043134350466,122.208755075342));
#39248=CARTESIAN_POINT('Ctrl Pts',(6.52465785584281,-1.80323922710623,122.216953017873));
#39249=CARTESIAN_POINT('Ctrl Pts',(6.56905934654972,-1.63409420633661,122.225150960405));
#39250=CARTESIAN_POINT('Ctrl Pts',(6.60684001709581,-1.46354159097082,122.233348902936));
#39251=CARTESIAN_POINT('Ctrl Pts',(6.6446316996796,-1.29293926415734,122.241549234944));
#39252=CARTESIAN_POINT('Ctrl Pts',(6.67579864064143,-1.1209288756312,122.249749566953));
#39253=CARTESIAN_POINT('Ctrl Pts',(6.70025827018953,-0.948065458054879,
122.257949898961));
#39254=CARTESIAN_POINT('Ctrl Pts',(6.72474339328254,-0.775021870076149,
122.266158777932));
#39255=CARTESIAN_POINT('Ctrl Pts',(6.74250718802028,-0.601123832397273,
122.274367656903));
#39256=CARTESIAN_POINT('Ctrl Pts',(6.75351893764249,-0.426932030778096,
122.282576535873));
#39257=CARTESIAN_POINT('Ctrl Pts',(6.7645365986273,-0.252646718959552,122.290789821561));
#39258=CARTESIAN_POINT('Ctrl Pts',(6.76879497988533,-0.0780676870470245,
122.299003107248));
#39259=CARTESIAN_POINT('Ctrl Pts',(6.76631553427568,0.0962449511384691,
122.307216392936));
#39260=CARTESIAN_POINT('Ctrl Pts',(6.76383246154269,0.270812587230064,122.315441693648));
#39261=CARTESIAN_POINT('Ctrl Pts',(6.75459188313694,0.445112692648713,122.32366699436));
#39262=CARTESIAN_POINT('Ctrl Pts',(6.7386672243945,0.618589556063905,122.331892295072));
#39263=CARTESIAN_POINT('Ctrl Pts',(6.72426529151869,0.775478452888617,122.339331087366));
#39264=CARTESIAN_POINT('Ctrl Pts',(6.70439713560802,0.931693923007618,122.34676987966));
#39265=CARTESIAN_POINT('Ctrl Pts',(6.67915281055769,1.08683335117182,122.354208671954));
#39266=CARTESIAN_POINT('Ctrl Pts',(6.65148500222167,1.2568663370111,122.362361596583));
#39267=CARTESIAN_POINT('Ctrl Pts',(6.61727681365689,1.42610807811444,122.370514521212));
#39268=CARTESIAN_POINT('Ctrl Pts',(6.57658092578735,1.59401139474282,122.378667445841));
#39269=CARTESIAN_POINT('Ctrl Pts',(6.53593258489289,1.76171854180155,122.386810845014));
#39270=CARTESIAN_POINT('Ctrl Pts',(6.48881171897181,1.92809002555886,122.394954244186));
#39271=CARTESIAN_POINT('Ctrl Pts',(6.43532261394787,2.0925849694603,122.403097643359));
#39272=CARTESIAN_POINT('Ctrl Pts',(6.3818847567147,2.25692231112737,122.411233240359));
#39273=CARTESIAN_POINT('Ctrl Pts',(6.32209092029141,2.41938634719022,122.419368837359));
#39274=CARTESIAN_POINT('Ctrl Pts',(6.25609616704935,2.57944756655963,122.427504434359));
#39275=CARTESIAN_POINT('Ctrl Pts',(6.19015077552044,2.73938906586634,122.435633946224));
#39276=CARTESIAN_POINT('Ctrl Pts',(6.11801384166961,2.8969309906905,122.443763458089));
#39277=CARTESIAN_POINT('Ctrl Pts',(6.03988987083367,3.05156014985792,122.451892969954));
#39278=CARTESIAN_POINT('Ctrl Pts',(5.96008215820792,3.20952190431493,122.460197690512));
#39279=CARTESIAN_POINT('Ctrl Pts',(5.87402652457492,3.364443543617,122.46850241107));
#39280=CARTESIAN_POINT('Ctrl Pts',(5.78199273309133,3.51579991388576,122.476807131629));
#39281=CARTESIAN_POINT('Ctrl Pts',(5.69196934586634,3.66385002580691,122.484930442236));
#39282=CARTESIAN_POINT('Ctrl Pts',(5.5962264751229,3.80848869102389,122.493053752844));
#39283=CARTESIAN_POINT('Ctrl Pts',(5.49506263634738,3.94925000761144,122.501177063452));
#39284=CARTESIAN_POINT('Ctrl Pts',(5.39390564159697,4.09000180129046,122.509299824494));
#39285=CARTESIAN_POINT('Ctrl Pts',(5.28732862221035,4.22687647149645,122.517422585536));
#39286=CARTESIAN_POINT('Ctrl Pts',(5.17567266775499,4.3594382019079,122.525545346578));
#39287=CARTESIAN_POINT('Ctrl Pts',(5.06400302596988,4.49201618238076,122.533669103348));
#39288=CARTESIAN_POINT('Ctrl Pts',(4.9472534453284,4.62027989086817,122.541792860118));
#39289=CARTESIAN_POINT('Ctrl Pts',(4.8258044005045,4.7438276621386,122.549916616888));
#39290=CARTESIAN_POINT('Ctrl Pts',(4.69961554516717,4.87219715124163,122.55835742076));
#39291=CARTESIAN_POINT('Ctrl Pts',(4.56835331246919,4.99547486805166,122.566798224632));
#39292=CARTESIAN_POINT('Ctrl Pts',(4.4324849164597,5.11325399969112,122.575239028504));
#39293=CARTESIAN_POINT('Ctrl Pts',(4.30155297331786,5.2267539085738,122.583373155977));
#39294=CARTESIAN_POINT('Ctrl Pts',(4.16634401070505,5.33514757407355,122.59150728345));
#39295=CARTESIAN_POINT('Ctrl Pts',(4.02730790080774,5.43811365016322,122.599641410922));
#39296=CARTESIAN_POINT('Ctrl Pts',(3.88819094874203,5.54113959559813,122.607780267961));
#39297=CARTESIAN_POINT('Ctrl Pts',(3.74524271662562,5.63873145810819,122.615919125));
#39298=CARTESIAN_POINT('Ctrl Pts',(3.59894037176235,5.73061228844694,122.624057982039));
#39299=CARTESIAN_POINT('Ctrl Pts',(3.4524688313739,5.82259937699609,122.632206251492));
#39300=CARTESIAN_POINT('Ctrl Pts',(3.30263575147417,5.90886206933069,122.640354520945));
#39301=CARTESIAN_POINT('Ctrl Pts',(3.14994160343767,5.98916996711001,122.648502790398));
#39302=CARTESIAN_POINT('Ctrl Pts',(3.13305439803827,5.99805161701233,122.649403948049));
#39303=CARTESIAN_POINT('Ctrl Pts',(3.11613221692979,6.00686048136917,122.650305105701));
#39304=CARTESIAN_POINT('Ctrl Pts',(3.0991757505325,6.01559628526643,122.651206263353));
#39305=CARTESIAN_POINT('Origin',(0.,0.,-3.69717978381041));
#39306=CARTESIAN_POINT('',(3.09917575053273,6.01559628526632,125.045751582742));
#39307=CARTESIAN_POINT('',(3.09917575053274,6.01559628526631,124.651594452187));
#39308=CARTESIAN_POINT('',(3.09917575053259,6.01559628526639,-3.69717978381041));
#39309=CARTESIAN_POINT('',(-6.767,9.5990736862783E-10,123.697179783765));
#39310=CARTESIAN_POINT('Ctrl Pts',(-6.767,7.29749759425155E-12,123.69717978381));
#39311=CARTESIAN_POINT('Ctrl Pts',(-6.7670000000002,-0.186007249408372,
123.705929295616));
#39312=CARTESIAN_POINT('Ctrl Pts',(-6.75932637295478,-0.372014355520227,
123.714678807422));
#39313=CARTESIAN_POINT('Ctrl Pts',(-6.74400518266988,-0.55738953714775,
123.723428319228));
#39314=CARTESIAN_POINT('Ctrl Pts',(-6.72868405709725,-0.742763935804244,
123.732177794078));
#39315=CARTESIAN_POINT('Ctrl Pts',(-6.70571545653088,-0.927506129688036,
123.740927268929));
#39316=CARTESIAN_POINT('Ctrl Pts',(-6.67517739415764,-1.11098863924292,
123.74967674378));
#39317=CARTESIAN_POINT('Ctrl Pts',(-6.64463945823195,-1.2944703890602,123.758426182402));
#39318=CARTESIAN_POINT('Ctrl Pts',(-6.60653217027257,-1.47669218227774,
123.767175621024));
#39319=CARTESIAN_POINT('Ctrl Pts',(-6.56098496116814,-1.65703510503716,
123.775925059646));
#39320=CARTESIAN_POINT('Ctrl Pts',(-6.51543793687627,-1.83737729603632,
123.784674462766));
#39321=CARTESIAN_POINT('Ctrl Pts',(-6.46245112202755,-2.01584035396681,
123.793423865886));
#39322=CARTESIAN_POINT('Ctrl Pts',(-6.40220448416364,-2.19181813637788,
123.802173269006));
#39323=CARTESIAN_POINT('Ctrl Pts',(-6.3419580857532,-2.36779521935587,123.810922637351));
#39324=CARTESIAN_POINT('Ctrl Pts',(-6.27445201489379,-2.54128677544469,
123.819672005697));
#39325=CARTESIAN_POINT('Ctrl Pts',(-6.1999155513634,-2.71170355237482,123.828421374042));
#39326=CARTESIAN_POINT('Ctrl Pts',(-6.1253793778921,-2.88211966612706,123.837170708339));
#39327=CARTESIAN_POINT('Ctrl Pts',(-6.04381298133805,-3.04946076210072,
123.845920042636));
#39328=CARTESIAN_POINT('Ctrl Pts',(-5.95549339426511,-3.21315848206475,
123.854669376933));
#39329=CARTESIAN_POINT('Ctrl Pts',(-5.86717414355369,-3.37685557859274,
123.863418677909));
#39330=CARTESIAN_POINT('Ctrl Pts',(-5.7721018898645,-3.53690907466967,123.872167978884));
#39331=CARTESIAN_POINT('Ctrl Pts',(-5.67059953467281,-3.69277536784578,
123.88091727986));
#39332=CARTESIAN_POINT('Ctrl Pts',(-5.56909755761995,-3.8486410803546,123.889666548241));
#39333=CARTESIAN_POINT('Ctrl Pts',(-5.46116568338317,-4.00031938103941,
123.898415816621));
#39334=CARTESIAN_POINT('Ctrl Pts',(-5.3471704868638,-4.14729511662876,123.907165085002));
#39335=CARTESIAN_POINT('Ctrl Pts',(-5.23317570555786,-4.29427031687713,
123.915914321515));
#39336=CARTESIAN_POINT('Ctrl Pts',(-5.11311782179076,-4.43654275986818,
123.924663558027));
#39337=CARTESIAN_POINT('Ctrl Pts',(-4.98740459172287,-4.57362924147352,
123.93341279454));
#39338=CARTESIAN_POINT('Ctrl Pts',(-4.86169180911126,-4.7107152351413,123.942161999911));
#39339=CARTESIAN_POINT('Ctrl Pts',(-4.73032391415752,-4.8426150931621,123.950911205282));
#39340=CARTESIAN_POINT('Ctrl Pts',(-4.59374707237639,-4.96888084331204,
123.959660410653));
#39341=CARTESIAN_POINT('Ctrl Pts',(-4.45717070537756,-5.09514615452415,
123.96840958561));
#39342=CARTESIAN_POINT('Ctrl Pts',(-4.3153856381987,-5.21577720253334,123.977158760566));
#39343=CARTESIAN_POINT('Ctrl Pts',(-4.16887341291016,-5.33036429028362,
123.985907935522));
#39344=CARTESIAN_POINT('Ctrl Pts',(-4.02236168477707,-5.44495098920905,
123.99465708079));
#39345=CARTESIAN_POINT('Ctrl Pts',(-3.87112305634806,-5.55349359238503,
124.003406226058));
#39346=CARTESIAN_POINT('Ctrl Pts',(-3.71567117317098,-5.65562346102233,
124.012155371326));
#39347=CARTESIAN_POINT('Ctrl Pts',(-3.56021980457667,-5.75775299158543,
124.020904487632));
#39348=CARTESIAN_POINT('Ctrl Pts',(-3.40055544862755,-5.8534696727514,124.029653603938));
#39349=CARTESIAN_POINT('Ctrl Pts',(-3.23722036323771,-5.94244842803361,
124.038402720244));
#39350=CARTESIAN_POINT('Ctrl Pts',(-3.07388580496435,-6.03142689616277,
124.047151808315));
#39351=CARTESIAN_POINT('Ctrl Pts',(-2.90688079258117,-6.11366734484627,
124.055900896386));
#39352=CARTESIAN_POINT('Ctrl Pts',(-2.73677251095046,-6.18889046787111,
124.064649984457));
#39353=CARTESIAN_POINT('Ctrl Pts',(-2.56666476417127,-6.26411335438071,
124.073399045019));
#39354=CARTESIAN_POINT('Ctrl Pts',(-2.39345402972626,-6.33231884350088,
124.082148105582));
#39355=CARTESIAN_POINT('Ctrl Pts',(-2.21772856474624,-6.3932752962084,124.090897166144));
#39356=CARTESIAN_POINT('Ctrl Pts',(-2.0420036376887,-6.45423156231892,124.099646199924));
#39357=CARTESIAN_POINT('Ctrl Pts',(-1.86376426620707,-6.5079387425188,124.108395233704));
#39358=CARTESIAN_POINT('Ctrl Pts',(-1.68361578195316,-6.55421443795962,
124.117144267484));
#39359=CARTESIAN_POINT('Ctrl Pts',(-1.50346783420525,-6.60048999558529,
124.125893275208));
#39360=CARTESIAN_POINT('Ctrl Pts',(-1.32141106257932,-6.63933404145358,
124.134642282932));
#39361=CARTESIAN_POINT('Ctrl Pts',(-1.13806375959759,-6.67061465526908,
124.143391290656));
#39362=CARTESIAN_POINT('Ctrl Pts',(-0.954716987426143,-6.70189517852381,
124.152140273051));
#39363=CARTESIAN_POINT('Ctrl Pts',(-0.770079973816703,-6.7256122653575,
124.160889255446));
#39364=CARTESIAN_POINT('Ctrl Pts',(-0.58477977055911,-6.74168536939724,
124.169638237841));
#39365=CARTESIAN_POINT('Ctrl Pts',(-0.39149064756057,-6.75845143942355,
124.178764418517));
#39366=CARTESIAN_POINT('Ctrl Pts',(-0.19748021311099,-6.76689975924007,
124.187890599193));
#39367=CARTESIAN_POINT('Ctrl Pts',(-0.00346532630443964,-6.76699911271707,
124.197016779869));
#39368=CARTESIAN_POINT('Ctrl Pts',(0.184486595289502,-6.76709536139791,
124.205857767399));
#39369=CARTESIAN_POINT('Ctrl Pts',(0.372442378178774,-6.75935659726806,
124.214698754929));
#39370=CARTESIAN_POINT('Ctrl Pts',(0.559750217715735,-6.74380965729069,
124.223539742459));
#39371=CARTESIAN_POINT('Ctrl Pts',(0.745129914451417,-6.72842275717324,
124.232289721057));
#39372=CARTESIAN_POINT('Ctrl Pts',(0.929874656307869,-6.7053877227356,124.241039699655));
#39373=CARTESIAN_POINT('Ctrl Pts',(1.11335688289149,-6.67478280180847,124.249789678252));
#39374=CARTESIAN_POINT('Ctrl Pts',(1.2968372311823,-6.64417819418146,124.258539567277));
#39375=CARTESIAN_POINT('Ctrl Pts',(1.47905480729612,-6.60600390230215,124.267289456302));
#39376=CARTESIAN_POINT('Ctrl Pts',(1.65939064804189,-6.56038959797291,124.276039345327));
#39377=CARTESIAN_POINT('Ctrl Pts',(1.83972470263655,-6.51477574543428,124.284789147688));
#39378=CARTESIAN_POINT('Ctrl Pts',(2.01817678125248,-6.46172209820287,124.293538950049));
#39379=CARTESIAN_POINT('Ctrl Pts',(2.1941407234709,-6.40140886724216,124.30228875241));
#39380=CARTESIAN_POINT('Ctrl Pts',(2.37010298131508,-6.34109621361594,124.311038471015));
#39381=CARTESIAN_POINT('Ctrl Pts',(2.54357687926326,-6.27352420826209,124.319788189621));
#39382=CARTESIAN_POINT('Ctrl Pts',(2.71397317789386,-6.19892237325752,124.328537908226));
#39383=CARTESIAN_POINT('Ctrl Pts',(2.88436790206616,-6.12432122757239,124.337287545985));
#39384=CARTESIAN_POINT('Ctrl Pts',(3.05168482125673,-6.04269049717712,124.346037183743));
#39385=CARTESIAN_POINT('Ctrl Pts',(3.21535561996807,-5.95430745235244,124.354786821501));
#39386=CARTESIAN_POINT('Ctrl Pts',(3.37902496074706,-5.86592519481847,124.36353638132));
#39387=CARTESIAN_POINT('Ctrl Pts',(3.53904799384309,-5.77079087940579,124.372285941139));
#39388=CARTESIAN_POINT('Ctrl Pts',(3.69488118814427,-5.66922763747387,124.381035500958));
#39389=CARTESIAN_POINT('Ctrl Pts',(3.85071304610288,-5.56766526649429,124.389784985746));
#39390=CARTESIAN_POINT('Ctrl Pts',(4.00235489705435,-5.45967423581104,124.398534470533));
#39391=CARTESIAN_POINT('Ctrl Pts',(4.14929168607134,-5.34562133936732,124.407283955321));
#39392=CARTESIAN_POINT('Ctrl Pts',(4.29622726385239,-5.23156938308956,124.416033367984));
#39393=CARTESIAN_POINT('Ctrl Pts',(4.43845763091551,-5.11145583677649,124.424782780647));
#39394=CARTESIAN_POINT('Ctrl Pts',(4.5754997066045,-4.98568866204681,124.43353219331));
#39395=CARTESIAN_POINT('Ctrl Pts',(4.71254069814799,-4.85992248226643,124.442281536757));
#39396=CARTESIAN_POINT('Ctrl Pts',(4.84439326930833,-4.72850295734495,124.451030880203));
#39397=CARTESIAN_POINT('Ctrl Pts',(4.97060959434234,-4.59187644222184,124.459780223649));
#39398=CARTESIAN_POINT('Ctrl Pts',(5.09682496280061,-4.45525096257183,124.468529500786));
#39399=CARTESIAN_POINT('Ctrl Pts',(5.21740397615396,-4.31341878218862,124.477278777922));
#39400=CARTESIAN_POINT('Ctrl Pts',(5.33193710451502,-4.1668616143923,124.486028055058));
#39401=CARTESIAN_POINT('Ctrl Pts',(5.44646940288971,-4.02030550865072,124.494777268791));
#39402=CARTESIAN_POINT('Ctrl Pts',(5.55495572749272,-3.86902470980697,124.503526482524));
#39403=CARTESIAN_POINT('Ctrl Pts',(5.65702762491083,-3.7135330146635,124.512275696257));
#39404=CARTESIAN_POINT('Ctrl Pts',(5.75909881654798,-3.55804239467469,124.521024849493));
#39405=CARTESIAN_POINT('Ctrl Pts',(5.85475551250444,-3.39834117620136,124.529774002729));
#39406=CARTESIAN_POINT('Ctrl Pts',(5.94367283727774,-3.23497174692558,124.538523155966));
#39407=CARTESIAN_POINT('Ctrl Pts',(6.03258957676015,-3.07160339301549,124.547272251611));
#39408=CARTESIAN_POINT('Ctrl Pts',(6.11476689685011,-2.9045671283008,124.556021347257));
#39409=CARTESIAN_POINT('Ctrl Pts',(6.1899257052501,-2.73443024476471,124.564770442902));
#39410=CARTESIAN_POINT('Ctrl Pts',(6.2650840438847,-2.56429442463586,124.573519483863));
#39411=CARTESIAN_POINT('Ctrl Pts',(6.3332238428311,-2.39105828656536,124.582268524824));
#39412=CARTESIAN_POINT('Ctrl Pts',(6.39411368719849,-2.21531017132612,124.591017565785));
#39413=CARTESIAN_POINT('Ctrl Pts',(6.45500317120724,-2.03956309620041,124.599766554968));
#39414=CARTESIAN_POINT('Ctrl Pts',(6.50864269269924,-1.86130434439155,124.60851554415));
#39415=CARTESIAN_POINT('Ctrl Pts',(6.55485008446201,-1.68113930720461,124.617264533333));
#39416=CARTESIAN_POINT('Ctrl Pts',(6.60199664749287,-1.49731239212355,124.626191346862));
#39417=CARTESIAN_POINT('Ctrl Pts',(6.64140563640805,-1.31150116500184,124.635118160391));
#39418=CARTESIAN_POINT('Ctrl Pts',(6.67293772282086,-1.1243625515617,124.644044973921));
#39419=CARTESIAN_POINT('Ctrl Pts',(6.703844949498,-0.940932395056396,124.652794888076));
#39420=CARTESIAN_POINT('Ctrl Pts',(6.72718449348874,-0.756227260511717,
124.661544802232));
#39421=CARTESIAN_POINT('Ctrl Pts',(6.7428770737389,-0.570874564546637,124.670294716387));
#39422=CARTESIAN_POINT('Ctrl Pts',(6.75856934538642,-0.385525513637384,
124.679044458471));
#39423=CARTESIAN_POINT('Ctrl Pts',(6.76661493004089,-0.199529212423096,
124.687794200555));
#39424=CARTESIAN_POINT('Ctrl Pts',(6.76698649908906,-0.0135174386052461,
124.696543942639));
#39425=CARTESIAN_POINT('Ctrl Pts',(6.76735806132402,0.17249092444091,124.705293524285));
#39426=CARTESIAN_POINT('Ctrl Pts',(6.76005588896315,0.358514472896495,124.714043105931));
#39427=CARTESIAN_POINT('Ctrl Pts',(6.74510478454624,0.543921359657261,124.722792687577));
#39428=CARTESIAN_POINT('Ctrl Pts',(6.73015393440741,0.729325093145562,124.731542120416));
#39429=CARTESIAN_POINT('Ctrl Pts',(6.70755443556963,0.914111900251542,124.740291553255));
#39430=CARTESIAN_POINT('Ctrl Pts',(6.67738304682396,1.09765415591065,124.749040986094));
#39431=CARTESIAN_POINT('Ctrl Pts',(6.64721213111952,1.28119353390797,124.757790281755));
#39432=CARTESIAN_POINT('Ctrl Pts',(6.609469609556,1.46348811672175,124.766539577417));
#39433=CARTESIAN_POINT('Ctrl Pts',(6.56428366991303,1.64391876347743,124.775288873078));
#39434=CARTESIAN_POINT('Ctrl Pts',(6.51909837867848,1.8243468210925,124.784038043189));
#39435=CARTESIAN_POINT('Ctrl Pts',(6.46646995272061,2.00291071819993,124.7927872133));
#39436=CARTESIAN_POINT('Ctrl Pts',(6.40657713281698,2.17900400212265,124.80153638341));
#39437=CARTESIAN_POINT('Ctrl Pts',(6.34668509279221,2.35509499309223,124.810285439596));
#39438=CARTESIAN_POINT('Ctrl Pts',(6.27952894037699,2.52871516397691,124.819034495782));
#39439=CARTESIAN_POINT('Ctrl Pts',(6.20533675061632,2.69927486770993,124.827783551968));
#39440=CARTESIAN_POINT('Ctrl Pts',(6.12832117908109,2.87632521635515,124.83686555325));
#39441=CARTESIAN_POINT('Ctrl Pts',(6.04372366626276,3.05007728919607,124.845947554532));
#39442=CARTESIAN_POINT('Ctrl Pts',(5.95185378008069,3.21989527477824,124.855029555815));
#39443=CARTESIAN_POINT('Ctrl Pts',(5.86334450817578,3.38350129286393,124.863779336122));
#39444=CARTESIAN_POINT('Ctrl Pts',(5.76808562057468,3.54345567124616,124.872529116429));
#39445=CARTESIAN_POINT('Ctrl Pts',(5.66640068804701,3.69921508464976,124.881278896736));
#39446=CARTESIAN_POINT('Ctrl Pts',(5.56471941108154,3.8549688985195,124.890028362489));
#39447=CARTESIAN_POINT('Ctrl Pts',(5.45661270815357,4.00652780919305,124.898777828243));
#39448=CARTESIAN_POINT('Ctrl Pts',(5.34244776449371,4.15337704568899,124.907527293996));
#39449=CARTESIAN_POINT('Ctrl Pts',(5.22828631819854,4.30022178355936,124.916276491716));
#39450=CARTESIAN_POINT('Ctrl Pts',(5.10806717844328,4.44235690972381,124.925025689436));
#39451=CARTESIAN_POINT('Ctrl Pts',(4.98219864544978,4.57929969070363,124.933774887155));
#39452=CARTESIAN_POINT('Ctrl Pts',(4.85633329944293,4.71623900429725,124.942523863345));
#39453=CARTESIAN_POINT('Ctrl Pts',(4.72481904033925,4.84798602483347,124.951272839536));
#39454=CARTESIAN_POINT('Ctrl Pts',(4.58810250737484,4.97409332258863,124.960021815726));
#39455=CARTESIAN_POINT('Ctrl Pts',(4.45137708685929,5.10020881821885,124.968771360662));
#39456=CARTESIAN_POINT('Ctrl Pts',(4.30944892636339,5.22068366307696,124.977520905598));
#39457=CARTESIAN_POINT('Ctrl Pts',(4.16280009466949,5.33510865604625,124.986270450534));
#39458=CARTESIAN_POINT('Ctrl Pts',(4.0161598834906,5.44952692272693,124.995019481143));
#39459=CARTESIAN_POINT('Ctrl Pts',(3.86479978232483,5.55789587288452,125.003768511751));
#39460=CARTESIAN_POINT('Ctrl Pts',(3.70923383581298,5.65984746713726,125.012517542359));
#39461=CARTESIAN_POINT('Ctrl Pts',(3.55366577799778,5.76180044505236,125.021266691707));
#39462=CARTESIAN_POINT('Ctrl Pts',(3.39389200027085,5.85733573570917,125.030015841055));
#39463=CARTESIAN_POINT('Ctrl Pts',(3.23045513626293,5.94612887621791,125.038764990403));
#39464=CARTESIAN_POINT('Ctrl Pts',(3.18695122151752,5.96976399206596,125.041093854516));
#39465=CARTESIAN_POINT('Ctrl Pts',(3.14318791262759,5.99292165435284,125.043422718629));
#39466=CARTESIAN_POINT('Ctrl Pts',(3.09917575053273,6.01559628526632,125.045751582742));
#39467=CARTESIAN_POINT('Ctrl Pts',(3.09917575053267,6.01559628526635,123.045751582742));
#39468=CARTESIAN_POINT('Ctrl Pts',(2.93382384459276,6.10078395293754,123.054501030655));
#39469=CARTESIAN_POINT('Ctrl Pts',(2.76495772122998,6.17915010267043,123.063250478567));
#39470=CARTESIAN_POINT('Ctrl Pts',(2.59315093316728,6.2504285643317,123.07199992648));
#39471=CARTESIAN_POINT('Ctrl Pts',(2.42134553245636,6.32170645041444,123.08074930374));
#39472=CARTESIAN_POINT('Ctrl Pts',(2.24659977927612,6.3858966531345,123.089498681));
#39473=CARTESIAN_POINT('Ctrl Pts',(2.06950718689942,6.44278115439068,123.09824805826));
#39474=CARTESIAN_POINT('Ctrl Pts',(1.89241596572886,6.49966521519717,123.106997367774));
#39475=CARTESIAN_POINT('Ctrl Pts',(1.71297821457224,6.54924360009539,123.115746677289));
#39476=CARTESIAN_POINT('Ctrl Pts',(1.53180337335873,6.59134792173549,123.124495986804));
#39477=CARTESIAN_POINT('Ctrl Pts',(1.3506298747782,6.63345193135297,123.13324523148));
#39478=CARTESIAN_POINT('Ctrl Pts',(1.16771959102998,6.6680819236823,123.141994476156));
#39479=CARTESIAN_POINT('Ctrl Pts',(0.983693746907394,6.6951202836316,123.150743720832));
#39480=CARTESIAN_POINT('Ctrl Pts',(0.799669205420503,6.72215845218859,123.159492903576));
#39481=CARTESIAN_POINT('Ctrl Pts',(0.614529402874191,6.74160505424572,123.16824208632));
#39482=CARTESIAN_POINT('Ctrl Pts',(0.428903127364045,6.75339404354117,123.176991269065));
#39483=CARTESIAN_POINT('Ctrl Pts',(0.243278104164782,6.76518295330327,123.185740392783));
#39484=CARTESIAN_POINT('Ctrl Pts',(0.0571669005401258,6.76931433552275,
123.194489516502));
#39485=CARTESIAN_POINT('Ctrl Pts',(-0.128798404776401,6.76577415902475,
123.20323864022));
#39486=CARTESIAN_POINT('Ctrl Pts',(-0.314762517257868,6.76223400523447,
123.21198770782));
#39487=CARTESIAN_POINT('Ctrl Pts',(-0.500580446818165,6.75102239665099,
123.220736775419));
#39488=CARTESIAN_POINT('Ctrl Pts',(-0.685621118841152,6.73217741012512,
123.229485843018));
#39489=CARTESIAN_POINT('Ctrl Pts',(-0.87066066541316,6.71333253821789,123.238234857404));
#39490=CARTESIAN_POINT('Ctrl Pts',(-1.05492267885367,6.68685441030631,123.24698387179));
#39491=CARTESIAN_POINT('Ctrl Pts',(-1.23778137635145,6.65283295028197,123.255732886175));
#39492=CARTESIAN_POINT('Ctrl Pts',(-1.42999922976776,6.61707018862254,123.264929696542));
#39493=CARTESIAN_POINT('Ctrl Pts',(-1.62066601229693,6.5729717293534,123.274126506908));
#39494=CARTESIAN_POINT('Ctrl Pts',(-1.80906628494505,6.52070304312926,123.283323317275));
#39495=CARTESIAN_POINT('Ctrl Pts',(-1.98831342539696,6.47097374916823,123.292073315012));
#39496=CARTESIAN_POINT('Ctrl Pts',(-2.16550875890926,6.41384933991479,123.30082331275));
#39497=CARTESIAN_POINT('Ctrl Pts',(-2.34005036708298,6.34952386242581,123.309573310488));
#39498=CARTESIAN_POINT('Ctrl Pts',(-2.51458843541424,6.28519968950862,123.318323130769));
#39499=CARTESIAN_POINT('Ctrl Pts',(-2.68647261712446,6.21367483973524,123.32707295105));
#39500=CARTESIAN_POINT('Ctrl Pts',(-2.85511905903184,6.13519226746425,123.335822771331));
#39501=CARTESIAN_POINT('Ctrl Pts',(-3.02376230483394,6.05671118255677,123.344572425789));
#39502=CARTESIAN_POINT('Ctrl Pts',(-3.18916767374478,5.97127275995531,123.353322080248));
#39503=CARTESIAN_POINT('Ctrl Pts',(-3.35077334097431,5.87916720441049,123.362071734706));
#39504=CARTESIAN_POINT('Ctrl Pts',(-3.51237616032097,5.78706327198842,123.370821234975));
#39505=CARTESIAN_POINT('Ctrl Pts',(-3.67017916297119,5.68829258365641,123.379570735243));
#39506=CARTESIAN_POINT('Ctrl Pts',(-3.82364636561378,5.58319061744524,123.388320235511));
#39507=CARTESIAN_POINT('Ctrl Pts',(-3.97711106773808,5.47809036371325,123.39706959322));
#39508=CARTESIAN_POINT('Ctrl Pts',(-4.12623987477037,5.36665920046984,123.405818950928));
#39509=CARTESIAN_POINT('Ctrl Pts',(-4.27052628209146,5.24927559516227,123.414568308637));
#39510=CARTESIAN_POINT('Ctrl Pts',(-4.41481053020291,5.13189374647068,123.423317535413));
#39511=CARTESIAN_POINT('Ctrl Pts',(-4.55425230131945,5.00855981481522,123.43206676219));
#39512=CARTESIAN_POINT('Ctrl Pts',(-4.68837800626071,4.87969268196378,123.440815988966));
#39513=CARTESIAN_POINT('Ctrl Pts',(-4.82250188224545,4.75082730636225,123.449565096437));
#39514=CARTESIAN_POINT('Ctrl Pts',(-4.95130963048748,4.6164290790805,123.458314203908));
#39515=CARTESIAN_POINT('Ctrl Pts',(-5.07436379029284,4.47695444736317,123.467063311379));
#39516=CARTESIAN_POINT('Ctrl Pts',(-5.19741643558843,4.33748153225334,123.475812311169));
#39517=CARTESIAN_POINT('Ctrl Pts',(-5.31471544458936,4.19293255259452,123.484561310958));
#39518=CARTESIAN_POINT('Ctrl Pts',(-5.4258624527192,4.04379841784577,123.493310310748));
#39519=CARTESIAN_POINT('Ctrl Pts',(-5.53702160015578,3.89464799489424,123.50206026609));
#39520=CARTESIAN_POINT('Ctrl Pts',(-5.64202723077814,3.74091164449034,123.510810221432));
#39521=CARTESIAN_POINT('Ctrl Pts',(-5.74052265229671,3.58311159168513,123.519560176775));
#39522=CARTESIAN_POINT('Ctrl Pts',(-5.83901427063769,3.42531763197151,123.528309794257));
#39523=CARTESIAN_POINT('Ctrl Pts',(-5.93099603112741,3.26346052701063,123.537059411739));
#39524=CARTESIAN_POINT('Ctrl Pts',(-6.01615550619908,3.09809004472602,123.545809029222));
#39525=CARTESIAN_POINT('Ctrl Pts',(-6.10131214576109,2.93272506869425,123.554558355373));
#39526=CARTESIAN_POINT('Ctrl Pts',(-6.17964682326215,2.76384720422556,123.563307681524));
#39527=CARTESIAN_POINT('Ctrl Pts',(-6.25089348286192,2.59203002797313,123.572057007675));
#39528=CARTESIAN_POINT('Ctrl Pts',(-6.32213814887107,2.42021765942834,123.580806089007));
#39529=CARTESIAN_POINT('Ctrl Pts',(-6.38629508410515,2.24546640837803,123.589555170338));
#39530=CARTESIAN_POINT('Ctrl Pts',(-6.44314639817899,2.06836976666,123.59830425167));
#39531=CARTESIAN_POINT('Ctrl Pts',(-6.50000285281951,1.89125711164286,123.607054124104));
#39532=CARTESIAN_POINT('Ctrl Pts',(-6.54955227671666,1.71179891446311,123.615803996539));
#39533=CARTESIAN_POINT('Ctrl Pts',(-6.5916263592497,1.53060476284526,123.624553868973));
#39534=CARTESIAN_POINT('Ctrl Pts',(-6.63369752053947,1.34942319170836,123.633303133896));
#39535=CARTESIAN_POINT('Ctrl Pts',(-6.66829431423173,1.16650618648884,123.642052398818));
#39536=CARTESIAN_POINT('Ctrl Pts',(-6.69529923744506,0.982474997680675,
123.65080166374));
#39537=CARTESIAN_POINT('Ctrl Pts',(-6.72230554730701,0.798434359240222,
123.65955137792));
#39538=CARTESIAN_POINT('Ctrl Pts',(-6.74171916496132,0.613279706303111,
123.6683010921));
#39539=CARTESIAN_POINT('Ctrl Pts',(-6.75347414816876,0.427639953718374,
123.67705080628));
#39540=CARTESIAN_POINT('Ctrl Pts',(-6.76248837756593,0.285283364559399,
123.683760465441));
#39541=CARTESIAN_POINT('Ctrl Pts',(-6.76699999997977,0.142641701764922,
123.690470124603));
#39542=CARTESIAN_POINT('Ctrl Pts',(-6.767,9.59715867638603E-10,123.697179783765));
#39543=CARTESIAN_POINT('',(-6.766999991942,0.000330237817373678,123.302820216223));
#39544=CARTESIAN_POINT('Ctrl Pts',(3.0991757505325,6.01559628526643,122.651206263353));
#39545=CARTESIAN_POINT('Ctrl Pts',(2.96868116764643,6.08282580461548,122.658141446023));
#39546=CARTESIAN_POINT('Ctrl Pts',(2.83615539198715,6.14572607912599,122.665076628692));
#39547=CARTESIAN_POINT('Ctrl Pts',(2.70191747454246,6.20418656721106,122.672011811362));
#39548=CARTESIAN_POINT('Ctrl Pts',(2.54255793686262,6.27358749752281,122.680244861494));
#39549=CARTESIAN_POINT('Ctrl Pts',(2.38028978695587,6.33694602721171,122.688477911626));
#39550=CARTESIAN_POINT('Ctrl Pts',(2.21561077191667,6.39400953294307,122.696710961758));
#39551=CARTESIAN_POINT('Ctrl Pts',(2.05112786427039,6.45100508481075,122.704934207593));
#39552=CARTESIAN_POINT('Ctrl Pts',(1.88424014342203,6.50172042379528,122.713157453427));
#39553=CARTESIAN_POINT('Ctrl Pts',(1.71546768173177,6.54594986483504,122.721380699262));
#39554=CARTESIAN_POINT('Ctrl Pts',(1.54686242192798,6.59013548802735,122.729595798376));
#39555=CARTESIAN_POINT('Ctrl Pts',(1.37637648393742,6.62784791964217,122.737810897489));
#39556=CARTESIAN_POINT('Ctrl Pts',(1.20454764095067,6.65893039313974,122.746025996603));
#39557=CARTESIAN_POINT('Ctrl Pts',(1.03285464829981,6.68998829239011,122.754234600742));
#39558=CARTESIAN_POINT('Ctrl Pts',(0.859821216261961,6.71442661054856,122.762443204881));
#39559=CARTESIAN_POINT('Ctrl Pts',(0.685998021285147,6.7321390148149,122.77065180902));
#39560=CARTESIAN_POINT('Ctrl Pts',(0.512277483922408,6.74984095837625,122.778855565268));
#39561=CARTESIAN_POINT('Ctrl Pts',(0.3377684681806,6.76082486506108,122.787059321517));
#39562=CARTESIAN_POINT('Ctrl Pts',(0.163029630048409,6.76503587128156,122.795263077766));
#39563=CARTESIAN_POINT('Ctrl Pts',(-0.01165750726604,6.76924563157145,122.803464406731));
#39564=CARTESIAN_POINT('Ctrl Pts',(-0.186573973989754,6.76668647067645,
122.811665735695));
#39565=CARTESIAN_POINT('Ctrl Pts',(-0.361157976604668,6.75735554162535,
122.819867064659));
#39566=CARTESIAN_POINT('Ctrl Pts',(-0.535717902419002,6.74802589939844,
122.828067262582));
#39567=CARTESIAN_POINT('Ctrl Pts',(-0.709945097750385,6.73192636731659,
122.836267460505));
#39568=CARTESIAN_POINT('Ctrl Pts',(-0.883279734910622,6.70910619307045,
122.844467658427));
#39569=CARTESIAN_POINT('Ctrl Pts',(-1.05662187933245,6.68628503046433,122.852668211507));
#39570=CARTESIAN_POINT('Ctrl Pts',(-1.22907103332113,6.6567426925079,122.860868764587));
#39571=CARTESIAN_POINT('Ctrl Pts',(-1.40007438230559,6.6205800896909,122.869069317667));
#39572=CARTESIAN_POINT('Ctrl Pts',(-1.57111612673847,6.58440936727064,122.87727171202));
#39573=CARTESIAN_POINT('Ctrl Pts',(-1.74071106914144,6.5416154935125,122.885474106373));
#39574=CARTESIAN_POINT('Ctrl Pts',(-1.90831838714597,6.49235010864946,122.893676500726));
#39575=CARTESIAN_POINT('Ctrl Pts',(-2.07608244745648,6.44303865199121,122.90188656576));
#39576=CARTESIAN_POINT('Ctrl Pts',(-2.24185482549696,6.38724369400404,122.910096630794));
#39577=CARTESIAN_POINT('Ctrl Pts',(-2.40511072476101,6.32516651177181,122.918306695828));
#39578=CARTESIAN_POINT('Ctrl Pts',(-2.56844475540239,6.26305962050138,122.926520690053));
#39579=CARTESIAN_POINT('Ctrl Pts',(-2.72925957648426,6.19466465054113,122.934734684279));
#39580=CARTESIAN_POINT('Ctrl Pts',(-2.88705214789691,6.12023029757246,122.942948678504));
#39581=CARTESIAN_POINT('Ctrl Pts',(-3.04505984313874,6.04569446578961,122.951173871139));
#39582=CARTESIAN_POINT('Ctrl Pts',(-3.20003673621005,5.96510296120563,122.959399063774));
#39583=CARTESIAN_POINT('Ctrl Pts',(-3.35150501644361,5.87875013287292,122.967624256409));
#39584=CARTESIAN_POINT('Ctrl Pts',(-3.48772011644028,5.80109321930529,122.975021154529));
#39585=CARTESIAN_POINT('Ctrl Pts',(-3.62109788751653,5.71877760673496,122.982418052649));
#39586=CARTESIAN_POINT('Ctrl Pts',(-3.75131258146814,5.63204606835907,122.989814950769));
#39587=CARTESIAN_POINT('Ctrl Pts',(-3.90351582426913,5.53066871229175,122.99846091726));
#39588=CARTESIAN_POINT('Ctrl Pts',(-4.0517427285922,5.42302764116862,123.007106883751));
#39589=CARTESIAN_POINT('Ctrl Pts',(-4.19547607149495,5.30945096347196,123.015752850242));
#39590=CARTESIAN_POINT('Ctrl Pts',(-4.33902555991244,5.19601956578614,123.024387757366));
#39591=CARTESIAN_POINT('Ctrl Pts',(-4.47809271039161,5.07666788947707,123.033022664491));
#39592=CARTESIAN_POINT('Ctrl Pts',(-4.61218953336684,4.95176702887983,123.041657571615));
#39593=CARTESIAN_POINT('Ctrl Pts',(-4.75073826263271,4.82271956052067,123.050579150687));
#39594=CARTESIAN_POINT('Ctrl Pts',(-4.88398068823489,4.68774827252662,123.059500729758));
#39595=CARTESIAN_POINT('Ctrl Pts',(-5.01141360740328,4.54730938638809,123.06842230883));
#39596=CARTESIAN_POINT('Ctrl Pts',(-5.13441115902607,4.41175854708852,123.077033367805));
#39597=CARTESIAN_POINT('Ctrl Pts',(-5.25199653218815,4.2711145284883,123.085644426781));
#39598=CARTESIAN_POINT('Ctrl Pts',(-5.36375252695179,4.1258269267649,123.094255485757));
#39599=CARTESIAN_POINT('Ctrl Pts',(-5.47540313065247,3.98067633795801,123.102858424106));
#39600=CARTESIAN_POINT('Ctrl Pts',(-5.58123513095635,3.83089113775599,123.111461362456));
#39601=CARTESIAN_POINT('Ctrl Pts',(-5.68087051348509,3.67695515461035,123.120064300805));
#39602=CARTESIAN_POINT('Ctrl Pts',(-5.78039432743483,3.52319154415464,123.128657605854));
#39603=CARTESIAN_POINT('Ctrl Pts',(-5.87373520092814,3.36528667868517,123.137250910903));
#39604=CARTESIAN_POINT('Ctrl Pts',(-5.96055737582634,3.20375479234636,123.145844215951));
#39605=CARTESIAN_POINT('Ctrl Pts',(-5.97023078724505,3.18575749619905,123.146801650792));
#39606=CARTESIAN_POINT('Ctrl Pts',(-5.97982332173152,3.1677152062004,123.147759085632));
#39607=CARTESIAN_POINT('Ctrl Pts',(-5.98933454802696,3.14962865617691,123.148716520473));
#39608=CARTESIAN_POINT('Ctrl Pts',(-6.0740841776925,2.98846874169211,123.157247728295));
#39609=CARTESIAN_POINT('Ctrl Pts',(-6.15228050461095,2.82397133033367,123.165778936117));
#39610=CARTESIAN_POINT('Ctrl Pts',(-6.2236859368796,2.65669387756421,123.174310143939));
#39611=CARTESIAN_POINT('Ctrl Pts',(-6.29514980765615,2.4892795242196,123.182848333738));
#39612=CARTESIAN_POINT('Ctrl Pts',(-6.35981156980806,2.3190808789042,123.191386523536));
#39613=CARTESIAN_POINT('Ctrl Pts',(-6.41748259220156,2.14667328179906,123.199924713335));
#39614=CARTESIAN_POINT('Ctrl Pts',(-6.47539971699918,1.97352996123396,123.208499338573));
#39615=CARTESIAN_POINT('Ctrl Pts',(-6.526266216052,1.7981591019537,123.21707396381));
#39616=CARTESIAN_POINT('Ctrl Pts',(-6.56994244704369,1.62115552694169,123.225648589048));
#39617=CARTESIAN_POINT('Ctrl Pts',(-6.61354175832605,1.44446367900022,123.23420811322));
#39618=CARTESIAN_POINT('Ctrl Pts',(-6.64997609272299,1.26614518054161,123.242767637391));
#39619=CARTESIAN_POINT('Ctrl Pts',(-6.67915839676466,1.08679902048545,123.251327161562));
#39620=CARTESIAN_POINT('Ctrl Pts',(-6.70841792774907,0.906978245552623,
123.259909337333));
#39621=CARTESIAN_POINT('Ctrl Pts',(-6.73038697429634,0.726124680428343,
123.268491513104));
#39622=CARTESIAN_POINT('Ctrl Pts',(-6.74503026730746,0.544844650433756,
123.277073688876));
#39623=CARTESIAN_POINT('Ctrl Pts',(-6.75967356031858,0.363564620439041,
123.285655864647));
#39624=CARTESIAN_POINT('Ctrl Pts',(-6.76699113312658,0.181858442082662,
123.294238040419));
#39625=CARTESIAN_POINT('Ctrl Pts',(-6.76699999194196,0.000330238511045327,
123.30282021619));
#39626=CARTESIAN_POINT('Ctrl Pts',(-6.766999991942,0.00033023781756751,
123.302820216223));
#39627=CARTESIAN_POINT('Ctrl Pts',(-6.76700164278173,-0.033497603479895,
123.304419507541));
#39628=CARTESIAN_POINT('Ctrl Pts',(-6.76674963937631,-0.0673246409772959,
123.306018798859));
#39629=CARTESIAN_POINT('Ctrl Pts',(-6.76624401275958,-0.101148207078348,
123.307618090177));
#39630=CARTESIAN_POINT('Ctrl Pts',(-6.76364331035425,-0.275120515509138,
123.315844082718));
#39631=CARTESIAN_POINT('Ctrl Pts',(-6.75432517494951,-0.449220794044856,
123.32407007526));
#39632=CARTESIAN_POINT('Ctrl Pts',(-6.73827102947005,-0.62289046661881,
123.332296067801));
#39633=CARTESIAN_POINT('Ctrl Pts',(-6.72223371468706,-0.79637806898869,
123.340513436452));
#39634=CARTESIAN_POINT('Ctrl Pts',(-6.69947448526771,-0.969435610532295,
123.348730805104));
#39635=CARTESIAN_POINT('Ctrl Pts',(-6.67002676664729,-1.1415042409946,123.356948173755));
#39636=CARTESIAN_POINT('Ctrl Pts',(-6.64060402779263,-1.31342690992635,
123.365158571818));
#39637=CARTESIAN_POINT('Ctrl Pts',(-6.60450415972966,-1.48436198732553,
123.37336896988));
#39638=CARTESIAN_POINT('Ctrl Pts',(-6.56181241397131,-1.65375537606142,
123.381579367942));
#39639=CARTESIAN_POINT('Ctrl Pts',(-6.51914834252906,-1.82303895794583,
123.389784443731));
#39640=CARTESIAN_POINT('Ctrl Pts',(-6.46990099232645,-1.99078249567337,
123.39798951952));
#39641=CARTESIAN_POINT('Ctrl Pts',(-6.41420677020203,-2.15644163127465,
123.406194595309));
#39642=CARTESIAN_POINT('Ctrl Pts',(-6.35853751229379,-2.32202651230668,
123.414395993278));
#39643=CARTESIAN_POINT('Ctrl Pts',(-6.29642725358434,-2.48552851372514,
123.422597391248));
#39644=CARTESIAN_POINT('Ctrl Pts',(-6.22806239781778,-2.64641791274323,
123.430798789217));
#39645=CARTESIAN_POINT('Ctrl Pts',(-6.15970289695587,-2.80729470956417,
123.438999544785));
#39646=CARTESIAN_POINT('Ctrl Pts',(-6.08508990686431,-2.96555897870409,
123.447200300352));
#39647=CARTESIAN_POINT('Ctrl Pts',(-6.00445831727879,-3.12070013235197,
123.45540105592));
#39648=CARTESIAN_POINT('Ctrl Pts',(-5.92382713726337,-3.27584049795663,
123.463601769832));
#39649=CARTESIAN_POINT('Ctrl Pts',(-5.83717758297189,-3.42785746118635,
123.471802483744));
#39650=CARTESIAN_POINT('Ctrl Pts',(-5.74479087999741,-3.57626435615414,
123.480003197656));
#39651=CARTESIAN_POINT('Ctrl Pts',(-5.65238790353241,-3.72469739231022,
123.488205356085));
#39652=CARTESIAN_POINT('Ctrl Pts',(-5.55424595439009,-3.8695187890467,123.496407514515));
#39653=CARTESIAN_POINT('Ctrl Pts',(-5.45069005157621,-4.01027018561694,
123.504609672944));
#39654=CARTESIAN_POINT('Ctrl Pts',(-5.34709714076258,-4.151071882822,123.512814762597));
#39655=CARTESIAN_POINT('Ctrl Pts',(-5.23808663429509,-4.28780039392327,
123.52101985225));
#39656=CARTESIAN_POINT('Ctrl Pts',(-5.12402437777205,-4.42002977094021,
123.529224941903));
#39657=CARTESIAN_POINT('Ctrl Pts',(-5.00983181860643,-4.552410204387,123.537439404901));
#39658=CARTESIAN_POINT('Ctrl Pts',(-4.89057621420478,-4.68028096383782,
123.545653867899));
#39659=CARTESIAN_POINT('Ctrl Pts',(-4.76666161661593,-4.80325161038649,
123.553868330897));
#39660=CARTESIAN_POINT('Ctrl Pts',(-4.64267360354444,-4.92629511315664,
123.562087660704));
#39661=CARTESIAN_POINT('Ctrl Pts',(-4.51402135845631,-5.04443247392336,
123.570306990512));
#39662=CARTESIAN_POINT('Ctrl Pts',(-4.38114258680509,-5.15731312158597,
123.578526320319));
#39663=CARTESIAN_POINT('Ctrl Pts',(-4.24805792755352,-5.27036867096828,
123.58675838548));
#39664=CARTESIAN_POINT('Ctrl Pts',(-4.11073393650097,-5.37815100933363,
123.59499045064));
#39665=CARTESIAN_POINT('Ctrl Pts',(-3.96963898802552,-5.48035175009303,
123.603222515801));
#39666=CARTESIAN_POINT('Ctrl Pts',(-3.8428127171619,-5.57221711430392,123.610622087062));
#39667=CARTESIAN_POINT('Ctrl Pts',(-3.71294016052135,-5.65957320741325,
123.618021658324));
#39668=CARTESIAN_POINT('Ctrl Pts',(-3.5803780409309,-5.74222797213937,123.625421229585));
#39669=CARTESIAN_POINT('Ctrl Pts',(-3.43427432566459,-5.83332615500079,
123.633576687991));
#39670=CARTESIAN_POINT('Ctrl Pts',(-3.28445321693816,-5.91899315122175,
123.641732146398));
#39671=CARTESIAN_POINT('Ctrl Pts',(-3.13135933964687,-5.99890637416574,
123.649887604805));
#39672=CARTESIAN_POINT('Ctrl Pts',(-2.97845179772811,-6.07872233221298,
123.658033136947));
#39673=CARTESIAN_POINT('Ctrl Pts',(-2.82227973681938,-6.15279828969649,
123.666178669089));
#39674=CARTESIAN_POINT('Ctrl Pts',(-2.66331727159753,-6.22085445182656,
123.674324201231));
#39675=CARTESIAN_POINT('Ctrl Pts',(-2.50451485797348,-6.28884209150717,
123.682461532031));
#39676=CARTESIAN_POINT('Ctrl Pts',(-2.34292796678921,-6.35082185951427,
123.690598862832));
#39677=CARTESIAN_POINT('Ctrl Pts',(-2.17905586686755,-6.40655949235392,
123.698736193632));
#39678=CARTESIAN_POINT('Ctrl Pts',(-2.01531432358844,-6.46225271910974,
123.706867041434));
#39679=CARTESIAN_POINT('Ctrl Pts',(-1.84929154108083,-6.51171359560858,
123.714997889236));
#39680=CARTESIAN_POINT('Ctrl Pts',(-1.68150735197763,-6.55475568005743,
123.723128737038));
#39681=CARTESIAN_POINT('Ctrl Pts',(-1.51382159029733,-6.59777251468107,
123.731254815032));
#39682=CARTESIAN_POINT('Ctrl Pts',(-1.34437683296057,-6.63437796550534,
123.739380893026));
#39683=CARTESIAN_POINT('Ctrl Pts',(-1.17370867829032,-6.66443523027316,
123.74750697102));
#39684=CARTESIAN_POINT('Ctrl Pts',(-1.00243536551594,-6.69459907261191,
123.755661862602));
#39685=CARTESIAN_POINT('Ctrl Pts',(-0.829930317602609,-6.71816809240825,
123.763816754184));
#39686=CARTESIAN_POINT('Ctrl Pts',(-0.656746415364533,-6.7350555414121,
123.771971645766));
#39687=CARTESIAN_POINT('Ctrl Pts',(-0.484237869793059,-6.75187713526937,
123.780094736123));
#39688=CARTESIAN_POINT('Ctrl Pts',(-0.311056123235351,-6.76206915767,123.788217826479));
#39689=CARTESIAN_POINT('Ctrl Pts',(-0.137753630643398,-6.76559775165835,
123.796340916835));
#39690=CARTESIAN_POINT('Ctrl Pts',(0.0355624704512306,-6.76912662272801,
123.804464645054));
#39691=CARTESIAN_POINT('Ctrl Pts',(0.20899897071073,-6.76599101565496,123.812588373272));
#39692=CARTESIAN_POINT('Ctrl Pts',(0.382002756699721,-6.75620921033932,
123.820712101491));
#39693=CARTESIAN_POINT('Ctrl Pts',(0.555053041500488,-6.74642477593483,
123.828838013151));
#39694=CARTESIAN_POINT('Ctrl Pts',(0.727670015361962,-6.72999060703069,
123.836963924811));
#39695=CARTESIAN_POINT('Ctrl Pts',(0.899305070451042,-6.70697691887046,
123.845089836471));
#39696=CARTESIAN_POINT('Ctrl Pts',(1.07203774955942,-6.6838160557821,123.853267714182));
#39697=CARTESIAN_POINT('Ctrl Pts',(1.24377553509034,-6.65399127783878,123.861445591892));
#39698=CARTESIAN_POINT('Ctrl Pts',(1.4139698305962,-6.61762633564058,123.869623469602));
#39699=CARTESIAN_POINT('Ctrl Pts',(1.58335182564263,-6.58143495542439,123.877762316075));
#39700=CARTESIAN_POINT('Ctrl Pts',(1.75120469244766,-6.53876585348229,123.885901162548));
#39701=CARTESIAN_POINT('Ctrl Pts',(1.91700343289675,-6.48979097030576,123.894040009022));
#39702=CARTESIAN_POINT('Ctrl Pts',(2.08399484786531,-6.44046378592898,123.90223740235));
#39703=CARTESIAN_POINT('Ctrl Pts',(2.24890211442958,-6.38473987783791,123.910434795679));
#39704=CARTESIAN_POINT('Ctrl Pts',(2.41121018717397,-6.32284385646748,123.918632189007));
#39705=CARTESIAN_POINT('Ctrl Pts',(2.57351825991824,-6.26094783509708,123.926829582335));
#39706=CARTESIAN_POINT('Ctrl Pts',(2.73322682037374,-6.19287990260906,123.935026975664));
#39707=CARTESIAN_POINT('Ctrl Pts',(2.88984720503379,-6.11891102497482,123.943224368992));
#39708=CARTESIAN_POINT('Ctrl Pts',(3.04701815182596,-6.04468212714545,123.951450578329));
#39709=CARTESIAN_POINT('Ctrl Pts',(3.20154699203705,-5.96428991267037,123.959676787666));
#39710=CARTESIAN_POINT('Ctrl Pts',(3.35291692305904,-5.8779449731232,123.967902997003));
#39711=CARTESIAN_POINT('Ctrl Pts',(3.50411679644857,-5.79169703841639,123.976119964546));
#39712=CARTESIAN_POINT('Ctrl Pts',(3.65216451878241,-5.69950987161253,123.984336932089));
#39713=CARTESIAN_POINT('Ctrl Pts',(3.79656418546999,-5.60164166879734,123.992553899633));
#39714=CARTESIAN_POINT('Ctrl Pts',(3.94083060748751,-5.50386377378335,124.000763284976));
#39715=CARTESIAN_POINT('Ctrl Pts',(4.08145538284242,-5.40041548268226,124.008972670319));
#39716=CARTESIAN_POINT('Ctrl Pts',(4.21796803159714,-5.29160038971431,124.017182055663));
#39717=CARTESIAN_POINT('Ctrl Pts',(4.35438210380969,-5.18286387272958,124.025385512963));
#39718=CARTESIAN_POINT('Ctrl Pts',(4.48668968462899,-5.06876849564165,124.033588970264));
#39719=CARTESIAN_POINT('Ctrl Pts',(4.61445000628577,-4.94966060851542,124.041792427565));
#39720=CARTESIAN_POINT('Ctrl Pts',(4.74214369991099,-4.83061483710681,124.049991606696));
#39721=CARTESIAN_POINT('Ctrl Pts',(4.86529459699136,-4.70656200731514,124.058190785828));
#39722=CARTESIAN_POINT('Ctrl Pts',(4.98349564833184,-4.5778881728432,124.06638996496));
#39723=CARTESIAN_POINT('Ctrl Pts',(5.10167442804651,-4.44923858329514,124.07458759919));
#39724=CARTESIAN_POINT('Ctrl Pts',(5.21490497283096,-4.31596998303971,124.08278523342));
#39725=CARTESIAN_POINT('Ctrl Pts',(5.32281749377134,-4.17850486753358,124.09098286765));
#39726=CARTESIAN_POINT('Ctrl Pts',(5.43072222546795,-4.04104967440982,124.099179910165));
#39727=CARTESIAN_POINT('Ctrl Pts',(5.53330947562752,-3.89939885088064,124.107376952681));
#39728=CARTESIAN_POINT('Ctrl Pts',(5.63025016535381,-3.75400746876367,124.115573995196));
#39729=CARTESIAN_POINT('Ctrl Pts',(5.72720147660268,-3.6086001565161,124.123771935839));
#39730=CARTESIAN_POINT('Ctrl Pts',(5.81850479581267,-3.45945176764502,124.131969876482));
#39731=CARTESIAN_POINT('Ctrl Pts',(5.90387472776674,-3.30704584165947,124.140167817125));
#39732=CARTESIAN_POINT('Ctrl Pts',(5.9892695293673,-3.15459551735456,124.148368145961));
#39733=CARTESIAN_POINT('Ctrl Pts',(6.06872732552163,-2.99888607854712,124.156568474797));
#39734=CARTESIAN_POINT('Ctrl Pts',(6.14200895323333,-2.84042514747382,124.164768803633));
#39735=CARTESIAN_POINT('Ctrl Pts',(6.21536694230291,-2.68179909599794,124.172977677424));
#39736=CARTESIAN_POINT('Ctrl Pts',(6.28253575456501,-2.52041615015348,124.181186551216));
#39737=CARTESIAN_POINT('Ctrl Pts',(6.34332424525404,-2.35680430234931,124.189395425007));
#39738=CARTESIAN_POINT('Ctrl Pts',(6.40414536045541,-2.19310464587141,124.19760870441));
#39739=CARTESIAN_POINT('Ctrl Pts',(6.45857921603039,-2.02717404319272,124.205821983814));
#39740=CARTESIAN_POINT('Ctrl Pts',(6.50648478417683,-1.85955498796765,124.214035263217));
#39741=CARTESIAN_POINT('Ctrl Pts',(6.55446042174608,-1.69169076352939,124.222260555833));
#39742=CARTESIAN_POINT('Ctrl Pts',(6.59588860441139,-1.52213349956341,124.230485848448));
#39743=CARTESIAN_POINT('Ctrl Pts',(6.63067933757173,-1.35143646624593,124.238711141064));
#39744=CARTESIAN_POINT('Ctrl Pts',(6.66214337649842,-1.19706150449338,124.246149930176));
#39745=CARTESIAN_POINT('Ctrl Pts',(6.68817926852513,-1.04175461526081,124.253588719288));
#39746=CARTESIAN_POINT('Ctrl Pts',(6.70875710235929,-0.885927277796426,
124.2610275084));
#39747=CARTESIAN_POINT('Ctrl Pts',(6.73151314438449,-0.713605279835282,
124.269253709419));
#39748=CARTESIAN_POINT('Ctrl Pts',(6.74765729947289,-0.540165090666825,
124.277479910438));
#39749=CARTESIAN_POINT('Ctrl Pts',(6.75708660405581,-0.366155192902602,
124.285706111457));
#39750=CARTESIAN_POINT('Ctrl Pts',(6.76650531680238,-0.192340758583608,
124.293923072072));
#39751=CARTESIAN_POINT('Ctrl Pts',(6.76922417941891,-0.0179582448376579,
124.302140032688));
#39752=CARTESIAN_POINT('Ctrl Pts',(6.76519156342863,0.156435642083491,124.310356993304));
#39753=CARTESIAN_POINT('Ctrl Pts',(6.76116266785444,0.330668636466773,124.318566373105));
#39754=CARTESIAN_POINT('Ctrl Pts',(6.75039470677595,0.504912626840805,124.326775752907));
#39755=CARTESIAN_POINT('Ctrl Pts',(6.73288798451109,0.678607683441808,124.334985132709));
#39756=CARTESIAN_POINT('Ctrl Pts',(6.71539390100989,0.852177343024529,124.343188585849));
#39757=CARTESIAN_POINT('Ctrl Pts',(6.69117078231921,1.02519850280473,124.35139203899));
#39758=CARTESIAN_POINT('Ctrl Pts',(6.66027096730924,1.19711304479471,124.35959549213));
#39759=CARTESIAN_POINT('Ctrl Pts',(6.62938726161657,1.36893796081429,124.36779466848));
#39760=CARTESIAN_POINT('Ctrl Pts',(6.59183385733291,1.53965705623929,124.37599384483));
#39761=CARTESIAN_POINT('Ctrl Pts',(6.54771473279626,1.70871904592966,124.38419302118));
#39762=CARTESIAN_POINT('Ctrl Pts',(6.50360390993851,1.87774922405607,124.392390654732));
#39763=CARTESIAN_POINT('Ctrl Pts',(6.45292991213696,2.04512256931115,124.400588288283));
#39764=CARTESIAN_POINT('Ctrl Pts',(6.39584753416592,2.21029937332111,124.408785921835));
#39765=CARTESIAN_POINT('Ctrl Pts',(6.3387692675271,2.37546428054717,124.416982964955));
#39766=CARTESIAN_POINT('Ctrl Pts',(6.27528365626154,2.53843262230696,124.425180008076));
#39767=CARTESIAN_POINT('Ctrl Pts',(6.20559493137233,2.69868126086168,124.433377051196));
#39768=CARTESIAN_POINT('Ctrl Pts',(6.13589855997216,2.85894748250427,124.441574993728));
#39769=CARTESIAN_POINT('Ctrl Pts',(6.05999786200951,3.01649307741875,124.449772936259));
#39770=CARTESIAN_POINT('Ctrl Pts',(5.97814466214256,3.17081620383404,124.45797087879));
#39771=CARTESIAN_POINT('Ctrl Pts',(5.89626760429474,3.32518431124216,124.466171210798));
#39772=CARTESIAN_POINT('Ctrl Pts',(5.8084347566719,3.4763277624671,124.474371542807));
#39773=CARTESIAN_POINT('Ctrl Pts',(5.71494323247086,3.62377052938448,124.482571874815));
#39774=CARTESIAN_POINT('Ctrl Pts',(5.6213542648325,3.77136697151617,124.490780753786));
#39775=CARTESIAN_POINT('Ctrl Pts',(5.52209502989166,3.91525472009512,124.498989632757));
#39776=CARTESIAN_POINT('Ctrl Pts',(5.41750577645059,4.05498707299104,124.507198511727));
#39777=CARTESIAN_POINT('Ctrl Pts',(5.31286037707233,4.1947944374551,124.515411797415));
#39778=CARTESIAN_POINT('Ctrl Pts',(5.20287948081253,4.33044168089375,124.523625083102));
#39779=CARTESIAN_POINT('Ctrl Pts',(5.08794267584501,4.46151637084469,124.53183836879));
#39780=CARTESIAN_POINT('Ctrl Pts',(4.97283773249764,4.59278280691223,124.540063669502));
#39781=CARTESIAN_POINT('Ctrl Pts',(4.85276263875451,4.71946306149385,124.548288970214));
#39782=CARTESIAN_POINT('Ctrl Pts',(4.72813368781738,4.84118175966638,124.556514270926));
#39783=CARTESIAN_POINT('Ctrl Pts',(4.61542183541384,4.95126163950179,124.56395306322));
#39784=CARTESIAN_POINT('Ctrl Pts',(4.49898596854104,5.05728383354036,124.571391855514));
#39785=CARTESIAN_POINT('Ctrl Pts',(4.37915574804594,5.15900028439195,124.578830647808));
#39786=CARTESIAN_POINT('Ctrl Pts',(4.24781994086785,5.27048311502257,124.586983681211));
#39787=CARTESIAN_POINT('Ctrl Pts',(4.11201878678538,5.37712181140436,124.595136714613));
#39788=CARTESIAN_POINT('Ctrl Pts',(3.97214727178368,5.47853402392113,124.603289748016));
#39789=CARTESIAN_POINT('Ctrl Pts',(3.83246405080114,5.57980971605285,124.611431805864));
#39790=CARTESIAN_POINT('Ctrl Pts',(3.68872167560797,5.67587272549816,124.619573863713));
#39791=CARTESIAN_POINT('Ctrl Pts',(3.54135009387041,5.76637915096155,124.627715921561));
#39792=CARTESIAN_POINT('Ctrl Pts',(3.39728263191387,5.85485639232339,124.63567543177));
#39793=CARTESIAN_POINT('Ctrl Pts',(3.24974724590813,5.93802333903456,124.643634941979));
#39794=CARTESIAN_POINT('Ctrl Pts',(3.09917575053274,6.01559628526631,124.651594452187));
#39795=CARTESIAN_POINT('Origin',(0.,0.,-3.69717978381041));
#39796=CARTESIAN_POINT('',(3.09917575053273,6.01559628526631,127.045911902629));
#39797=CARTESIAN_POINT('',(3.09917575053261,6.01559628526638,126.651394038606));
#39798=CARTESIAN_POINT('',(3.09917575053259,6.01559628526639,-3.69717978381041));
#39799=CARTESIAN_POINT('',(-6.76699999483142,0.000264483490106234,125.697369247924));
#39800=CARTESIAN_POINT('Ctrl Pts',(-6.76699999483143,0.000264483490106234,
125.697369247924));
#39801=CARTESIAN_POINT('Ctrl Pts',(-6.76700666497119,-0.170395831555567,
125.705445979297));
#39802=CARTESIAN_POINT('Ctrl Pts',(-6.76055310740299,-0.341346504411689,
125.713522710671));
#39803=CARTESIAN_POINT('Ctrl Pts',(-6.74759927607116,-0.512047858665496,
125.721599442044));
#39804=CARTESIAN_POINT('Ctrl Pts',(-6.73466049174337,-0.682550928419518,
125.729666791591));
#39805=CARTESIAN_POINT('Ctrl Pts',(-6.71523648697607,-0.852804888403578,
125.737734141137));
#39806=CARTESIAN_POINT('Ctrl Pts',(-6.68933914014784,-1.02226751297604,
125.745801490683));
#39807=CARTESIAN_POINT('Ctrl Pts',(-6.6634662145074,-1.19157033436069,125.753861232721));
#39808=CARTESIAN_POINT('Ctrl Pts',(-6.63113215195376,-1.36008293983411,
125.76192097476));
#39809=CARTESIAN_POINT('Ctrl Pts',(-6.59240079476521,-1.52726577948277,
125.769980716799));
#39810=CARTESIAN_POINT('Ctrl Pts',(-6.55369750536983,-1.694327465273,125.778034618113));
#39811=CARTESIAN_POINT('Ctrl Pts',(-6.50860623349195,-1.86006094202274,
125.786088519428));
#39812=CARTESIAN_POINT('Ctrl Pts',(-6.45724228911631,-2.02393453936831,
125.794142420743));
#39813=CARTESIAN_POINT('Ctrl Pts',(-6.40370052093684,-2.19475635351177,
125.802537806307));
#39814=CARTESIAN_POINT('Ctrl Pts',(-6.34334257886107,-2.36355670945537,
125.810933191871));
#39815=CARTESIAN_POINT('Ctrl Pts',(-6.27635770124143,-2.52974761706922,
125.819328577435));
#39816=CARTESIAN_POINT('Ctrl Pts',(-6.21213961181366,-2.68907406426871,
125.827377194378));
#39817=CARTESIAN_POINT('Ctrl Pts',(-6.14183121813148,-2.84600193101904,
125.835425811321));
#39818=CARTESIAN_POINT('Ctrl Pts',(-6.06564932049882,-3.00003121995958,
125.843474428264));
#39819=CARTESIAN_POINT('Ctrl Pts',(-5.98946870220167,-3.15405792226021,
125.851522910045));
#39820=CARTESIAN_POINT('Ctrl Pts',(-5.90741494106427,-3.30518580913329,
125.859571391826));
#39821=CARTESIAN_POINT('Ctrl Pts',(-5.81975164502797,-3.45293784916472,
125.867619873607));
#39822=CARTESIAN_POINT('Ctrl Pts',(-5.73207250866444,-3.60071658726442,
125.87566980971));
#39823=CARTESIAN_POINT('Ctrl Pts',(-5.63878201021364,-3.74511794376387,
125.883719745812));
#39824=CARTESIAN_POINT('Ctrl Pts',(-5.54018800530699,-3.88569245641656,
125.891769681914));
#39825=CARTESIAN_POINT('Ctrl Pts',(-5.4415567090948,-4.02632013870272,125.899822662752));
#39826=CARTESIAN_POINT('Ctrl Pts',(-5.33761812784836,-4.1631177913874,125.907875643589));
#39827=CARTESIAN_POINT('Ctrl Pts',(-5.22872134141143,-4.29566783327909,
125.915928624427));
#39828=CARTESIAN_POINT('Ctrl Pts',(-5.11970598587234,-4.42836219843294,
125.923990373518));
#39829=CARTESIAN_POINT('Ctrl Pts',(-5.00572188434,-4.55679943201993,125.93205212261));
#39830=CARTESIAN_POINT('Ctrl Pts',(-4.88715649169459,-4.68059722959447,
125.940113871702));
#39831=CARTESIAN_POINT('Ctrl Pts',(-4.76851500700475,-4.80447447722863,
125.948180794605));
#39832=CARTESIAN_POINT('Ctrl Pts',(-4.64528664285792,-4.92370610134431,
125.956247717508));
#39833=CARTESIAN_POINT('Ctrl Pts',(-4.51789267863167,-5.03794945829812,
125.964314640411));
#39834=CARTESIAN_POINT('Ctrl Pts',(-4.39032760122543,-5.15234626478324,
125.972392398653));
#39835=CARTESIAN_POINT('Ctrl Pts',(-4.25858604145576,-5.26174119461539,
125.980470156895));
#39836=CARTESIAN_POINT('Ctrl Pts',(-4.12311955990129,-5.36583396078926,
125.988547915138));
#39837=CARTESIAN_POINT('Ctrl Pts',(-4.08352062257188,-5.3962618782849,125.990909168185));
#39838=CARTESIAN_POINT('Ctrl Pts',(-4.04360356575319,-5.4262370299317,125.993270421233));
#39839=CARTESIAN_POINT('Ctrl Pts',(-4.00338006729888,-5.45575265538624,
125.99563167428));
#39840=CARTESIAN_POINT('Ctrl Pts',(-3.86327100415885,-5.55856337025048,
126.003856541958));
#39841=CARTESIAN_POINT('Ctrl Pts',(-3.71900227672201,-5.65611774598859,
126.012081409635));
#39842=CARTESIAN_POINT('Ctrl Pts',(-3.57100494534304,-5.74806164548846,
126.020306277313));
#39843=CARTESIAN_POINT('Ctrl Pts',(-3.42317434952305,-5.83990195989437,
126.028521878756));
#39844=CARTESIAN_POINT('Ctrl Pts',(-3.27162381637479,-5.92614419684376,
126.0367374802));
#39845=CARTESIAN_POINT('Ctrl Pts',(-3.11681632686272,-6.00647525463995,
126.044953081644));
#39846=CARTESIAN_POINT('Ctrl Pts',(-2.9621521413842,-6.08673195062949,126.053161077972));
#39847=CARTESIAN_POINT('Ctrl Pts',(-2.80423732029464,-6.16108820072119,
126.0613690743));
#39848=CARTESIAN_POINT('Ctrl Pts',(-2.64356266883131,-6.22927487079849,
126.069577070628));
#39849=CARTESIAN_POINT('Ctrl Pts',(-2.48300448024666,-6.29741211667718,
126.077779117499));
#39850=CARTESIAN_POINT('Ctrl Pts',(-2.3196907746823,-6.35938855020906,126.085981164371));
#39851=CARTESIAN_POINT('Ctrl Pts',(-2.154135815517,-6.41498151893729,126.094183211242));
#39852=CARTESIAN_POINT('Ctrl Pts',(-1.98866761173854,-6.47054535540918,
126.102380960014));
#39853=CARTESIAN_POINT('Ctrl Pts',(-1.82096083341129,-6.51973227713905,
126.110578708785));
#39854=CARTESIAN_POINT('Ctrl Pts',(-1.65154860902888,-6.56236818473444,
126.118776457557));
#39855=CARTESIAN_POINT('Ctrl Pts',(-1.48216869662586,-6.60499596038674,
126.126972642773));
#39856=CARTESIAN_POINT('Ctrl Pts',(-1.31108433213543,-6.64107511719608,
126.135168827988));
#39857=CARTESIAN_POINT('Ctrl Pts',(-1.1388429527302,-6.67048167143999,126.143365013204));
#39858=CARTESIAN_POINT('Ctrl Pts',(-0.966614315353741,-6.69988605025333,
126.151560592084));
#39859=CARTESIAN_POINT('Ctrl Pts',(-0.793229187079543,-6.72261874829726,
126.159756170965));
#39860=CARTESIAN_POINT('Ctrl Pts',(-0.619244270849144,-6.73860709145596,
126.167951749845));
#39861=CARTESIAN_POINT('Ctrl Pts',(-0.445240571134841,-6.75459716072283,
126.176148213523));
#39862=CARTESIAN_POINT('Ctrl Pts',(-0.27063731185326,-6.76384139161749,
126.184344677202));
#39863=CARTESIAN_POINT('Ctrl Pts',(-0.0959954308768129,-6.76631907888261,
126.19254114088));
#39864=CARTESIAN_POINT('Ctrl Pts',(0.07869707866419,-6.76879748442761,126.200739980708));
#39865=CARTESIAN_POINT('Ctrl Pts',(0.25342787349751,-6.7645054339659,126.208938820536));
#39866=CARTESIAN_POINT('Ctrl Pts',(0.427636852273128,-6.75347434455614,
126.217137660364));
#39867=CARTESIAN_POINT('Ctrl Pts',(0.602027797283428,-6.74243173285965,
126.225345064113));
#39868=CARTESIAN_POINT('Ctrl Pts',(0.77589547870112,-6.72463604168225,126.233552467862));
#39869=CARTESIAN_POINT('Ctrl Pts',(0.948684742881594,-6.70017061414287,
126.241759871611));
#39870=CARTESIAN_POINT('Ctrl Pts',(1.1215665621358,-6.67569208162582,126.24997167168));
#39871=CARTESIAN_POINT('Ctrl Pts',(1.29336845984038,-6.64453675451651,126.258183471749));
#39872=CARTESIAN_POINT('Ctrl Pts',(1.46354639827537,-6.60683895218396,126.266395271818));
#39873=CARTESIAN_POINT('Ctrl Pts',(1.6339748624145,-6.5690856534189,126.274619160804));
#39874=CARTESIAN_POINT('Ctrl Pts',(1.8027742424728,-6.52477072238826,126.282843049791));
#39875=CARTESIAN_POINT('Ctrl Pts',(1.96941531432961,-6.47407849193104,126.291066938777));
#39876=CARTESIAN_POINT('Ctrl Pts',(2.12338878386462,-6.42723974734667,126.298665670027));
#39877=CARTESIAN_POINT('Ctrl Pts',(2.27551959781055,-6.37495704037652,126.306264401277));
#39878=CARTESIAN_POINT('Ctrl Pts',(2.42540700211847,-6.31741164355108,126.313863132527));
#39879=CARTESIAN_POINT('Ctrl Pts',(2.58764476592958,-6.25512464524265,126.322087980849));
#39880=CARTESIAN_POINT('Ctrl Pts',(2.74770929359056,-6.18649655697364,126.330312829171));
#39881=CARTESIAN_POINT('Ctrl Pts',(2.90506962383229,-6.11169857573874,126.338537677493));
#39882=CARTESIAN_POINT('Ctrl Pts',(3.0622527314522,-6.03698483361494,126.346753262812));
#39883=CARTESIAN_POINT('Ctrl Pts',(3.21673738499637,-5.9561151877116,126.354968848131));
#39884=CARTESIAN_POINT('Ctrl Pts',(3.36800988956307,-5.86930987287308,126.363184433451));
#39885=CARTESIAN_POINT('Ctrl Pts',(3.51914242140731,-5.78258487914959,126.371392416874));
#39886=CARTESIAN_POINT('Ctrl Pts',(3.66706841426848,-5.68993533192966,126.379600400297));
#39887=CARTESIAN_POINT('Ctrl Pts',(3.81129612084373,-5.59162864282326,126.38780838372));
#39888=CARTESIAN_POINT('Ctrl Pts',(3.9554193421296,-5.49339317167563,126.396010420897));
#39889=CARTESIAN_POINT('Ctrl Pts',(4.09584931835875,-5.3895089229256,126.404212458073));
#39890=CARTESIAN_POINT('Ctrl Pts',(4.23212072517856,-5.280288170878,126.41241449525));
#39891=CARTESIAN_POINT('Ctrl Pts',(4.36832077513082,-5.17112461095103,126.420612237529));
#39892=CARTESIAN_POINT('Ctrl Pts',(4.5003663144841,-5.05663033845595,126.428809979809));
#39893=CARTESIAN_POINT('Ctrl Pts',(4.62782266742955,-4.9371597461319,126.437007722088));
#39894=CARTESIAN_POINT('Ctrl Pts',(4.755254786659,-4.81771186916364,126.445203905702));
#39895=CARTESIAN_POINT('Ctrl Pts',(4.87809919175065,-4.69328979756881,126.453400089317));
#39896=CARTESIAN_POINT('Ctrl Pts',(4.99595563296128,-4.56428705423777,126.461596272931));
#39897=CARTESIAN_POINT('Ctrl Pts',(5.11380339829346,-4.43529380730853,126.469791853192));
#39898=CARTESIAN_POINT('Ctrl Pts',(5.22666368831546,-4.30172082449852,126.477987433453));
#39899=CARTESIAN_POINT('Ctrl Pts',(5.33417441025133,-4.16399716150478,126.486183013714));
#39900=CARTESIAN_POINT('Ctrl Pts',(5.4416967782023,-4.02625857970267,126.494379481754));
#39901=CARTESIAN_POINT('Ctrl Pts',(5.54386820270352,-3.88436870484852,126.502575949795));
#39902=CARTESIAN_POINT('Ctrl Pts',(5.64036802219003,-3.73878824945411,126.510772417836));
#39903=CARTESIAN_POINT('Ctrl Pts',(5.73689585201883,-3.59316553741706,126.518971265009));
#39904=CARTESIAN_POINT('Ctrl Pts',(5.82774859949183,-3.44385041008105,126.527170112183));
#39905=CARTESIAN_POINT('Ctrl Pts',(5.91264990493643,-3.2913310531843,126.535368959356));
#39906=CARTESIAN_POINT('Ctrl Pts',(5.99763994050094,-3.13865229872875,126.543576375122));
#39907=CARTESIAN_POINT('Ctrl Pts',(6.07666593285695,-2.98276293833167,126.551783790888));
#39908=CARTESIAN_POINT('Ctrl Pts',(6.14949788143819,-2.8241750664906,126.559991206654));
#39909=CARTESIAN_POINT('Ctrl Pts',(6.22236886538212,-2.66550219712831,126.568203021306));
#39910=CARTESIAN_POINT('Ctrl Pts',(6.28903905058444,-2.50412826439997,126.576414835958));
#39911=CARTESIAN_POINT('Ctrl Pts',(6.34932733121625,-2.34058356848678,126.58462665061));
#39912=CARTESIAN_POINT('Ctrl Pts',(6.40970439550668,-2.17679802814581,126.592850558408));
#39913=CARTESIAN_POINT('Ctrl Pts',(6.46368066195745,-2.01083567718833,126.601074466205));
#39914=CARTESIAN_POINT('Ctrl Pts',(6.51112510832687,-1.8432413905171,126.609298374003));
#39915=CARTESIAN_POINT('Ctrl Pts',(6.55496290055401,-1.68838736481421,126.616897112926));
#39916=CARTESIAN_POINT('Ctrl Pts',(6.5932247183944,-1.53214043268882,126.62449585185));
#39917=CARTESIAN_POINT('Ctrl Pts',(6.62584641610265,-1.37493573312345,126.632094590773));
#39918=CARTESIAN_POINT('Ctrl Pts',(6.66083891672611,-1.20630608065252,126.640245572948));
#39919=CARTESIAN_POINT('Ctrl Pts',(6.68944467460571,-1.03607480295576,126.648396555122));
#39920=CARTESIAN_POINT('Ctrl Pts',(6.71151692872969,-0.864771365954496,
126.656547537296));
#39921=CARTESIAN_POINT('Ctrl Pts',(6.73356354388478,-0.693666913772199,
126.664689051349));
#39922=CARTESIAN_POINT('Ctrl Pts',(6.74909171605032,-0.521493140358055,
126.672830565402));
#39923=CARTESIAN_POINT('Ctrl Pts',(6.75800510869489,-0.348792131295672,
126.680972079455));
#39924=CARTESIAN_POINT('Ctrl Pts',(6.76691002331251,-0.176255387835315,
126.689105849658));
#39925=CARTESIAN_POINT('Ctrl Pts',(6.76921266551185,-0.00319276980574204,
126.697239619861));
#39926=CARTESIAN_POINT('Ctrl Pts',(6.76486816740433,0.169846040988923,126.705373390065));
#39927=CARTESIAN_POINT('Ctrl Pts',(6.76052688785489,0.342756658503348,126.713501134483));
#39928=CARTESIAN_POINT('Ctrl Pts',(6.74954828245963,0.515643139853826,126.721628878901));
#39929=CARTESIAN_POINT('Ctrl Pts',(6.73193948586503,0.687953311389146,126.729756623319));
#39930=CARTESIAN_POINT('Ctrl Pts',(6.71434003237387,0.860172056361169,126.737880055213));
#39931=CARTESIAN_POINT('Ctrl Pts',(6.69011743081647,1.03181473749403,126.746003487107));
#39932=CARTESIAN_POINT('Ctrl Pts',(6.65933083642415,1.20233182235624,126.754126919001));
#39933=CARTESIAN_POINT('Ctrl Pts',(6.62834894398616,1.37393060053607,126.762301882752));
#39934=CARTESIAN_POINT('Ctrl Pts',(6.59071950768561,1.54438907747378,126.770476846502));
#39935=CARTESIAN_POINT('Ctrl Pts',(6.54655560714764,1.71315459971475,126.778651810253));
#39936=CARTESIAN_POINT('Ctrl Pts',(6.50268005401,1.88081824691726,126.786773399426));
#39937=CARTESIAN_POINT('Ctrl Pts',(6.45235522942674,2.04681062899697,126.794894988599));
#39938=CARTESIAN_POINT('Ctrl Pts',(6.39574276095292,2.21060252775536,126.803016577772));
#39939=CARTESIAN_POINT('Ctrl Pts',(6.33912281847213,2.37441605040376,126.811139239162));
#39940=CARTESIAN_POINT('Ctrl Pts',(6.27621369826234,2.53602816514689,126.819261900551));
#39941=CARTESIAN_POINT('Ctrl Pts',(6.20722607997339,2.6949273444934,126.82738456194));
#39942=CARTESIAN_POINT('Ctrl Pts',(6.1382162166206,2.85387776089482,126.835509842483));
#39943=CARTESIAN_POINT('Ctrl Pts',(6.06312409787922,3.01011316439387,126.843635123025));
#39944=CARTESIAN_POINT('Ctrl Pts',(5.98220744982599,3.16314448409276,126.851760403567));
#39945=CARTESIAN_POINT('Ctrl Pts',(5.90040923168254,3.31784304826555,126.859974207355));
#39946=CARTESIAN_POINT('Ctrl Pts',(5.81265900614377,3.46926696439047,126.868188011143));
#39947=CARTESIAN_POINT('Ctrl Pts',(5.71926880003638,3.61693978287314,126.876401814931));
#39948=CARTESIAN_POINT('Ctrl Pts',(5.62672523073721,3.76327386093632,126.884541155786));
#39949=CARTESIAN_POINT('Ctrl Pts',(5.52864377957336,3.90592430928612,126.892680496641));
#39950=CARTESIAN_POINT('Ctrl Pts',(5.42536932350576,4.0444600014789,126.900819837496));
#39951=CARTESIAN_POINT('Ctrl Pts',(5.32067765460782,4.18489678875281,126.90907087275));
#39952=CARTESIAN_POINT('Ctrl Pts',(5.21064966899737,4.32110476377659,126.917321908004));
#39953=CARTESIAN_POINT('Ctrl Pts',(5.09568372992345,4.45267294157042,126.925572943258));
#39954=CARTESIAN_POINT('Ctrl Pts',(4.98071779084954,4.58424111936425,126.933823978513));
#39955=CARTESIAN_POINT('Ctrl Pts',(4.86081421067522,4.71116926692677,126.942075013767));
#39956=CARTESIAN_POINT('Ctrl Pts',(4.73640624482451,4.83308854501833,126.950326049021));
#39957=CARTESIAN_POINT('Ctrl Pts',(4.612305237309,4.95470700524524,126.95855672606));
#39958=CARTESIAN_POINT('Ctrl Pts',(4.48333480053266,5.07172103184382,126.9667874031));
#39959=CARTESIAN_POINT('Ctrl Pts',(4.34986944856124,5.18371727435762,126.97501808014));
#39960=CARTESIAN_POINT('Ctrl Pts',(4.21654329177819,5.29559671248853,126.983240173149));
#39961=CARTESIAN_POINT('Ctrl Pts',(4.07873182077674,5.40246855319842,126.991462266158));
#39962=CARTESIAN_POINT('Ctrl Pts',(3.93684733088864,5.50395513183701,126.999684359167));
#39963=CARTESIAN_POINT('Ctrl Pts',(3.79512205608919,5.6053278277346,127.007897225789));
#39964=CARTESIAN_POINT('Ctrl Pts',(3.6493331580027,5.70132709457614,127.016110092411));
#39965=CARTESIAN_POINT('Ctrl Pts',(3.49992675786233,5.79161477392957,127.024322959033));
#39966=CARTESIAN_POINT('Ctrl Pts',(3.3690132171906,5.87072704604166,127.031519273565));
#39967=CARTESIAN_POINT('Ctrl Pts',(3.23532291245085,5.94545461306768,127.038715588097));
#39968=CARTESIAN_POINT('Ctrl Pts',(3.09917575053273,6.01559628526631,127.045911902629));
#39969=CARTESIAN_POINT('Ctrl Pts',(3.09917575053273,6.01559628526632,125.045751582742));
#39970=CARTESIAN_POINT('Ctrl Pts',(2.93382384521587,6.10078395261652,125.054501030622));
#39971=CARTESIAN_POINT('Ctrl Pts',(2.76495772250264,6.17915010207986,125.063250478501));
#39972=CARTESIAN_POINT('Ctrl Pts',(2.59315093510946,6.25042856352594,125.071999926381));
#39973=CARTESIAN_POINT('Ctrl Pts',(2.42134553504201,6.32170644940429,125.080749303609));
#39974=CARTESIAN_POINT('Ctrl Pts',(2.24659978252431,6.38589665197217,125.089498680837));
#39975=CARTESIAN_POINT('Ctrl Pts',(2.06950719082269,6.44278115313047,125.098248058066));
#39976=CARTESIAN_POINT('Ctrl Pts',(1.89241597030047,6.49966521384767,125.10699736755));
#39977=CARTESIAN_POINT('Ctrl Pts',(1.71297821980402,6.54924359870869,125.115746677035));
#39978=CARTESIAN_POINT('Ctrl Pts',(1.53180337925603,6.59134792036498,125.124495986519));
#39979=CARTESIAN_POINT('Ctrl Pts',(1.3506298813133,6.63345193000509,125.133245231166));
#39980=CARTESIAN_POINT('Ctrl Pts',(1.16771959820771,6.66808192240814,125.141994475813));
#39981=CARTESIAN_POINT('Ctrl Pts',(0.983693754726281,6.6951202824828,125.15074372046));
#39982=CARTESIAN_POINT('Ctrl Pts',(0.799669213852509,6.72215845116926,125.159492903177));
#39983=CARTESIAN_POINT('Ctrl Pts',(0.614529411917502,6.74160505340517,125.168242085893));
#39984=CARTESIAN_POINT('Ctrl Pts',(0.428903137010801,6.75339404292851,125.17699126861));
#39985=CARTESIAN_POINT('Ctrl Pts',(0.24327811438683,6.76518295292029,125.185740392302));
#39986=CARTESIAN_POINT('Ctrl Pts',(0.0571669113294544,6.76931433541626,
125.194489515994));
#39987=CARTESIAN_POINT('Ctrl Pts',(-0.128798393433531,6.76577415924068,
125.203238639687));
#39988=CARTESIAN_POINT('Ctrl Pts',(-0.314762505389531,6.76223400577229,
125.211987707261));
#39989=CARTESIAN_POINT('Ctrl Pts',(-0.500580434438059,6.75102239755431,
125.220736774835));
#39990=CARTESIAN_POINT('Ctrl Pts',(-0.685621105968318,6.73217741143612,
125.229485842409));
#39991=CARTESIAN_POINT('Ctrl Pts',(-0.870660652075532,6.71333253993372,
125.238234856771));
#39992=CARTESIAN_POINT('Ctrl Pts',(-1.05492266507006,6.68685441246682,125.246983871133));
#39993=CARTESIAN_POINT('Ctrl Pts',(-1.23778136214556,6.65283295292502,125.255732885496));
#39994=CARTESIAN_POINT('Ctrl Pts',(-1.42999398956116,6.61707116400479,125.264929445816));
#39995=CARTESIAN_POINT('Ctrl Pts',(-1.62065563051565,6.57297413101274,125.274126006137));
#39996=CARTESIAN_POINT('Ctrl Pts',(-1.80905090416564,6.52070731026455,125.283322566458));
#39997=CARTESIAN_POINT('Ctrl Pts',(-1.98829816030723,6.47097843955113,125.292072564117));
#39998=CARTESIAN_POINT('Ctrl Pts',(-2.16549362698938,6.41385444883848,125.300822561776));
#39999=CARTESIAN_POINT('Ctrl Pts',(-2.34003538537155,6.34952938375822,125.309572559436));
#40000=CARTESIAN_POINT('Ctrl Pts',(-2.51457360400769,6.28520562320472,125.318322379643));
#40001=CARTESIAN_POINT('Ctrl Pts',(-2.68645795305744,6.21368117965436,125.32707219985));
#40002=CARTESIAN_POINT('Ctrl Pts',(-2.85510457878042,6.1351990060818,125.335822020057));
#40003=CARTESIAN_POINT('Ctrl Pts',(-3.02374800849086,6.05671831982041,125.344571674447));
#40004=CARTESIAN_POINT('Ctrl Pts',(-3.1891535777815,5.97128028833215,125.353321328837));
#40005=CARTESIAN_POINT('Ctrl Pts',(-3.35075946119047,5.87917511503464,125.362070983227));
#40006=CARTESIAN_POINT('Ctrl Pts',(-3.51236249680474,5.78707156480072,125.370820483432));
#40007=CARTESIAN_POINT('Ctrl Pts',(-3.67016573151701,5.68830124978307,125.379569983637));
#40008=CARTESIAN_POINT('Ctrl Pts',(-3.82363318123566,5.58319964673965,125.388319483842));
#40009=CARTESIAN_POINT('Ctrl Pts',(-3.97709813051924,5.47809975610972,125.397068841492));
#40010=CARTESIAN_POINT('Ctrl Pts',(-4.12622719971903,5.36666894581433,125.405818199142));
#40011=CARTESIAN_POINT('Ctrl Pts',(-4.27051388333216,5.24928568209688,125.414567556791));
#40012=CARTESIAN_POINT('Ctrl Pts',(-4.41479840781406,5.13190417492316,125.423316783514));
#40013=CARTESIAN_POINT('Ctrl Pts',(-4.55424046941923,5.00857057342068,125.432066010237));
#40014=CARTESIAN_POINT('Ctrl Pts',(-4.68836647798648,4.87970375823089,125.44081523696));
#40015=CARTESIAN_POINT('Ctrl Pts',(-4.82249065766897,4.75083870021376,125.449564344382));
#40016=CARTESIAN_POINT('Ctrl Pts',(-4.95129872273929,4.61644077801867,125.458313451804));
#40017=CARTESIAN_POINT('Ctrl Pts',(-5.07435321143231,4.47696643784903,125.467062559227));
#40018=CARTESIAN_POINT('Ctrl Pts',(-5.19740618568199,4.33749381420342,125.475811558973));
#40019=CARTESIAN_POINT('Ctrl Pts',(-5.31470553568899,4.19294511246392,125.484560558719));
#40020=CARTESIAN_POINT('Ctrl Pts',(-5.42585289572275,4.04381124114084,125.493309558465));
#40021=CARTESIAN_POINT('Ctrl Pts',(-5.53701239368999,3.89466108353792,125.502059513652));
#40022=CARTESIAN_POINT('Ctrl Pts',(-5.64201838589909,3.74092498410192,125.51080946884));
#40023=CARTESIAN_POINT('Ctrl Pts',(-5.7405141788448,3.58312516701298,125.519559424027));
#40024=CARTESIAN_POINT('Ctrl Pts',(-5.83900616882317,3.42533144264672,125.528309041375));
#40025=CARTESIAN_POINT('Ctrl Pts',(-5.93098831075965,3.2634745577638,125.537058658722));
#40026=CARTESIAN_POINT('Ctrl Pts',(-6.01614817580147,3.09810427952332,125.54580827607));
#40027=CARTESIAN_POINT('Ctrl Pts',(-6.10130520551454,2.93273950715233,125.554557602106));
#40028=CARTESIAN_POINT('Ctrl Pts',(-6.17964028165778,2.76386183029532,125.563306928142));
#40029=CARTESIAN_POINT('Ctrl Pts',(-6.25088734704388,2.59204482495321,125.572056254179));
#40030=CARTESIAN_POINT('Ctrl Pts',(-6.32213241899031,2.42023262692257,125.580805335415));
#40031=CARTESIAN_POINT('Ctrl Pts',(-6.38628976727249,2.24548152967231,125.589554416652));
#40032=CARTESIAN_POINT('Ctrl Pts',(-6.44314150010717,2.06838502450504,125.598303497888));
#40033=CARTESIAN_POINT('Ctrl Pts',(-6.49999837221279,1.89127251020532,125.607053370022));
#40034=CARTESIAN_POINT('Ctrl Pts',(-6.54954821963115,1.71181443660043,125.615803242157));
#40035=CARTESIAN_POINT('Ctrl Pts',(-6.59162273031443,1.53062039095333,125.624553114291));
#40036=CARTESIAN_POINT('Ctrl Pts',(-6.63369432010818,1.34943892412851,125.633302378993));
#40037=CARTESIAN_POINT('Ctrl Pts',(-6.66829154679582,1.16652200558753,125.642051643695));
#40038=CARTESIAN_POINT('Ctrl Pts',(-6.69529690603127,0.982490885498748,
125.650800908397));
#40039=CARTESIAN_POINT('Ctrl Pts',(-6.72230365088011,0.798450322988453,
125.659550622014));
#40040=CARTESIAN_POINT('Ctrl Pts',(-6.7417177071427,0.61329572810763,125.66830033563));
#40041=CARTESIAN_POINT('Ctrl Pts',(-6.75347313109847,0.427656015427243,
125.677050049247));
#40042=CARTESIAN_POINT('Ctrl Pts',(-6.76248266272047,0.285378980759063,
125.683755959796));
#40043=CARTESIAN_POINT('Ctrl Pts',(-6.76699461942155,0.142817180247322,
125.690461870345));
#40044=CARTESIAN_POINT('Ctrl Pts',(-6.76699999518896,0.00025517189615077,
125.697167780894));
#40045=CARTESIAN_POINT('',(-6.76699862817337,0.00430886293122851,125.302820216149));
#40046=CARTESIAN_POINT('Ctrl Pts',(3.09917575053274,6.01559628526631,124.651594452187));
#40047=CARTESIAN_POINT('Ctrl Pts',(2.94538860019882,6.0948259051505,124.659723948344));
#40048=CARTESIAN_POINT('Ctrl Pts',(2.78843446991074,6.16821968728965,124.667853444502));
#40049=CARTESIAN_POINT('Ctrl Pts',(2.62880128532791,6.23551864741485,124.675982940659));
#40050=CARTESIAN_POINT('Ctrl Pts',(2.469253132826,6.30278175928809,124.684108106464));
#40051=CARTESIAN_POINT('Ctrl Pts',(2.30702910414561,6.36395637304771,124.692233272268));
#40052=CARTESIAN_POINT('Ctrl Pts',(2.14263979064315,6.41883040183745,124.700358438073));
#40053=CARTESIAN_POINT('Ctrl Pts',(1.97717870612209,6.47406219350409,124.708536577621));
#40054=CARTESIAN_POINT('Ctrl Pts',(1.80952433868321,6.52291078568762,124.716714717168));
#40055=CARTESIAN_POINT('Ctrl Pts',(1.64021620764073,6.56520980564922,124.724892856716));
#40056=CARTESIAN_POINT('Ctrl Pts',(1.47204394050188,6.60722504756875,124.733016130301));
#40057=CARTESIAN_POINT('Ctrl Pts',(1.30224039707465,6.64277826479993,124.741139403887));
#40058=CARTESIAN_POINT('Ctrl Pts',(1.13134756793747,6.67175701599826,124.749262677472));
#40059=CARTESIAN_POINT('Ctrl Pts',(0.960432600274631,6.70073952128522,124.757387003397));
#40060=CARTESIAN_POINT('Ctrl Pts',(0.788428426541787,6.72314580292431,124.765511329322));
#40061=CARTESIAN_POINT('Ctrl Pts',(0.61588508276254,6.73891493972365,124.773635655247));
#40062=CARTESIAN_POINT('Ctrl Pts',(0.443286559430474,6.75468911951044,124.781762579341));
#40063=CARTESIAN_POINT('Ctrl Pts',(0.27014888681954,6.76382189447387,124.789889503434));
#40064=CARTESIAN_POINT('Ctrl Pts',(0.0970250051294995,6.76630439371298,
124.798016427528));
#40065=CARTESIAN_POINT('Ctrl Pts',(-0.0780414356972559,6.7688147481592,
124.806234540835));
#40066=CARTESIAN_POINT('Ctrl Pts',(-0.25309338976398,6.7645246807498,124.814452654142));
#40067=CARTESIAN_POINT('Ctrl Pts',(-0.427562340379117,6.75347906231222,
124.82267076745));
#40068=CARTESIAN_POINT('Ctrl Pts',(-0.600392740664454,6.74253718039435,
124.83081169916));
#40069=CARTESIAN_POINT('Ctrl Pts',(-0.772650685166828,6.72496619823817,
124.83895263087));
#40070=CARTESIAN_POINT('Ctrl Pts',(-0.943792187809526,6.70086153462596,
124.84709356258));
#40071=CARTESIAN_POINT('Ctrl Pts',(-1.11736749809088,6.67641407798271,124.855350266686));
#40072=CARTESIAN_POINT('Ctrl Pts',(-1.28979398685506,6.64524578252713,124.863606970792));
#40073=CARTESIAN_POINT('Ctrl Pts',(-1.4605188123745,6.60750889509051,124.871863674898));
#40074=CARTESIAN_POINT('Ctrl Pts',(-1.63124363789394,6.56977200765389,124.880120379004));
#40075=CARTESIAN_POINT('Ctrl Pts',(-1.8002664449856,6.52546669049656,124.888377083109));
#40076=CARTESIAN_POINT('Ctrl Pts',(-1.96705462613735,6.47479614333854,124.896633787215));
#40077=CARTESIAN_POINT('Ctrl Pts',(-2.13336498911482,6.4242707581948,124.904866837347));
#40078=CARTESIAN_POINT('Ctrl Pts',(-2.2979705540881,6.36725967384907,124.913099887479));
#40079=CARTESIAN_POINT('Ctrl Pts',(-2.46032861007741,6.30389341045949,124.921332937611));
#40080=CARTESIAN_POINT('Ctrl Pts',(-2.62249332257937,6.24060260654907,124.929556183446));
#40081=CARTESIAN_POINT('Ctrl Pts',(-2.78241552515022,6.17097182238606,124.937779429281));
#40082=CARTESIAN_POINT('Ctrl Pts',(-2.93956595489824,6.09518178537796,124.946002675116));
#40083=CARTESIAN_POINT('Ctrl Pts',(-3.09656069663765,6.01946683311479,124.954217774229));
#40084=CARTESIAN_POINT('Ctrl Pts',(-3.25078881380083,5.93760493461024,124.962432873343));
#40085=CARTESIAN_POINT('Ctrl Pts',(-3.40173929587612,5.84982553268832,124.970647972456));
#40086=CARTESIAN_POINT('Ctrl Pts',(-3.55257043434711,5.76211553041366,124.978856576595));
#40087=CARTESIAN_POINT('Ctrl Pts',(-3.70012879092889,5.66849752252889,124.987065180734));
#40088=CARTESIAN_POINT('Ctrl Pts',(-3.84392624197688,5.56924770918313,124.995273784873));
#40089=CARTESIAN_POINT('Ctrl Pts',(-3.9876387682076,5.47005651142618,125.003477541122));
#40090=CARTESIAN_POINT('Ctrl Pts',(-4.12759451972279,5.36524033710329,125.011681297371));
#40091=CARTESIAN_POINT('Ctrl Pts',(-4.26333267911365,5.25511973861696,125.01988505362));
#40092=CARTESIAN_POINT('Ctrl Pts',(-4.39903067700317,5.14503172204116,125.028086382585));
#40093=CARTESIAN_POINT('Ctrl Pts',(-4.53051328826264,5.02964262995709,125.036287711549));
#40094=CARTESIAN_POINT('Ctrl Pts',(-4.65735104236138,4.90931464343195,125.044489040513));
#40095=CARTESIAN_POINT('Ctrl Pts',(-4.784171304323,4.78900325128484,125.052689238436));
#40096=CARTESIAN_POINT('Ctrl Pts',(-4.90634772452803,4.66375456717125,125.060889436359));
#40097=CARTESIAN_POINT('Ctrl Pts',(-5.0234861144979,4.53396915047366,125.069089634281));
#40098=CARTESIAN_POINT('Ctrl Pts',(-5.14062957782509,4.4041781126659,125.077290187361));
#40099=CARTESIAN_POINT('Ctrl Pts',(-5.25273433609446,4.26985021676648,125.085490740441));
#40100=CARTESIAN_POINT('Ctrl Pts',(-5.35944504467483,4.13142079835865,125.093691293521));
#40101=CARTESIAN_POINT('Ctrl Pts',(-5.4661797130524,3.99296029833928,125.101893687874));
#40102=CARTESIAN_POINT('Ctrl Pts',(-5.56751770081911,3.85039672530774,125.110096082227));
#40103=CARTESIAN_POINT('Ctrl Pts',(-5.66314569202678,3.70419625166898,125.118298476581));
#40104=CARTESIAN_POINT('Ctrl Pts',(-5.75886311221631,3.55785905488736,125.126508541614));
#40105=CARTESIAN_POINT('Ctrl Pts',(-5.84885967089522,3.40787846252971,125.134718606648));
#40106=CARTESIAN_POINT('Ctrl Pts',(-5.93286644233673,3.25474803593069,125.142928671682));
#40107=CARTESIAN_POINT('Ctrl Pts',(-6.01691341792889,3.10154432382583,125.151142665907));
#40108=CARTESIAN_POINT('Ctrl Pts',(-6.094964730807,2.94518809224704,125.159356660133));
#40109=CARTESIAN_POINT('Ctrl Pts',(-6.16679876877899,2.78619488646899,125.167570654358));
#40110=CARTESIAN_POINT('Ctrl Pts',(-6.23873074046976,2.62698491999723,125.175795846993));
#40111=CARTESIAN_POINT('Ctrl Pts',(-6.30442836263358,2.46513112659334,125.184021039628));
#40112=CARTESIAN_POINT('Ctrl Pts',(-6.36371883538669,2.30116743939781,125.192246232263));
#40113=CARTESIAN_POINT('Ctrl Pts',(-6.41703863054339,2.1537152466854,125.199643130383));
#40114=CARTESIAN_POINT('Ctrl Pts',(-6.4651773432269,2.00455709494514,125.207040028503));
#40115=CARTESIAN_POINT('Ctrl Pts',(-6.5080444707201,1.85408903969836,125.214436926623));
#40116=CARTESIAN_POINT('Ctrl Pts',(-6.56532637959985,1.65302360951934,125.224321154209));
#40117=CARTESIAN_POINT('Ctrl Pts',(-6.61330786675181,1.44922672452033,125.234205381795));
#40118=CARTESIAN_POINT('Ctrl Pts',(-6.6517697274498,1.24348240557814,125.24408960938));
#40119=CARTESIAN_POINT('Ctrl Pts',(-6.68992873370557,1.03935814816764,125.25389600708));
#40120=CARTESIAN_POINT('Ctrl Pts',(-6.71871742499295,0.833317035117996,
125.26370240478));
#40121=CARTESIAN_POINT('Ctrl Pts',(-6.73796965843727,0.626142062138283,
125.27350880248));
#40122=CARTESIAN_POINT('Ctrl Pts',(-6.75715135987306,0.419726090289727,
125.283279273703));
#40123=CARTESIAN_POINT('Ctrl Pts',(-6.76686626403555,0.212184572460418,
125.293049744926));
#40124=CARTESIAN_POINT('Ctrl Pts',(-6.76699862817337,0.00430886293105204,
125.302820216149));
#40125=CARTESIAN_POINT('Ctrl Pts',(-6.76699862817393,0.0043088620540932,
125.30282021619));
#40126=CARTESIAN_POINT('Ctrl Pts',(-6.76710572847117,-0.163890434048294,
125.310725836264));
#40127=CARTESIAN_POINT('Ctrl Pts',(-6.76093751050823,-0.332268221061752,
125.318631456339));
#40128=CARTESIAN_POINT('Ctrl Pts',(-6.74848063473331,-0.5002980338053,125.326537076413));
#40129=CARTESIAN_POINT('Ctrl Pts',(-6.73602882106901,-0.668259564138937,
125.334439483874));
#40130=CARTESIAN_POINT('Ctrl Pts',(-6.71729345518341,-0.835873016889208,
125.342341891336));
#40131=CARTESIAN_POINT('Ctrl Pts',(-6.69231329044887,-1.00261249866605,
125.350244298797));
#40132=CARTESIAN_POINT('Ctrl Pts',(-6.66797906649877,-1.165040406328,125.35794236464));
#40133=CARTESIAN_POINT('Ctrl Pts',(-6.63771907011902,-1.32663862890468,
125.365640430484));
#40134=CARTESIAN_POINT('Ctrl Pts',(-6.60161642942235,-1.48692619816216,
125.373338496327));
#40135=CARTESIAN_POINT('Ctrl Pts',(-6.56130376484322,-1.66590532243092,
125.381934253874));
#40136=CARTESIAN_POINT('Ctrl Pts',(-6.51373197784661,-1.8431390565141,125.390530011422));
#40137=CARTESIAN_POINT('Ctrl Pts',(-6.45908654331555,-2.01804113584437,
125.39912576897));
#40138=CARTESIAN_POINT('Ctrl Pts',(-6.40439012273616,-2.19310640476121,
125.407729546651));
#40139=CARTESIAN_POINT('Ctrl Pts',(-6.34260697192179,-2.36583538510928,
125.416333324333));
#40140=CARTESIAN_POINT('Ctrl Pts',(-6.27397138739989,-2.53566007778794,
125.424937102014));
#40141=CARTESIAN_POINT('Ctrl Pts',(-6.20263836438787,-2.71215902939211,
125.433879015682));
#40142=CARTESIAN_POINT('Ctrl Pts',(-6.12390355555075,-2.88552045053691,
125.44282092935));
#40143=CARTESIAN_POINT('Ctrl Pts',(-6.03808280548288,-3.05513420885761,
125.451762843018));
#40144=CARTESIAN_POINT('Ctrl Pts',(-5.95528252329576,-3.2187783979455,125.460390045349));
#40145=CARTESIAN_POINT('Ctrl Pts',(-5.86588676675858,-3.37893399160023,
125.46901724768));
#40146=CARTESIAN_POINT('Ctrl Pts',(-5.77022407419043,-3.53508177184535,
125.47764445001));
#40147=CARTESIAN_POINT('Ctrl Pts',(-5.67447027755016,-3.69137825895048,
125.486279868431));
#40148=CARTESIAN_POINT('Ctrl Pts',(-5.57243779871761,-3.84365905901317,
125.494915286851));
#40149=CARTESIAN_POINT('Ctrl Pts',(-5.46449742710046,-3.99143543968989,
125.503550705272));
#40150=CARTESIAN_POINT('Ctrl Pts',(-5.35639758895895,-4.13943013892024,
125.512198881293));
#40151=CARTESIAN_POINT('Ctrl Pts',(-5.2423726027151,-4.28290687917374,125.520847057314));
#40152=CARTESIAN_POINT('Ctrl Pts',(-5.12283324264721,-4.42141024651962,
125.529495233335));
#40153=CARTESIAN_POINT('Ctrl Pts',(-5.11018643160661,-4.43606337762485,
125.530410177567));
#40154=CARTESIAN_POINT('Ctrl Pts',(-5.09747793258958,-4.45066087703468,
125.531325121799));
#40155=CARTESIAN_POINT('Ctrl Pts',(-5.08470825549322,-4.46520223019283,
125.532240066031));
#40156=CARTESIAN_POINT('Ctrl Pts',(-4.96989987167918,-4.59593922862748,
125.540466058572));
#40157=CARTESIAN_POINT('Ctrl Pts',(-4.84989533998742,-4.72241708047132,
125.548692051113));
#40158=CARTESIAN_POINT('Ctrl Pts',(-4.72504278143572,-4.84419856256968,
125.556918043655));
#40159=CARTESIAN_POINT('Ctrl Pts',(-4.60032111465371,-4.96585237252506,
125.565135412306));
#40160=CARTESIAN_POINT('Ctrl Pts',(-4.47076179658654,-5.0828193691989,125.573352780958));
#40161=CARTESIAN_POINT('Ctrl Pts',(-4.3367527091754,-5.19469584667474,125.581570149609));
#40162=CARTESIAN_POINT('Ctrl Pts',(-4.20285729833344,-5.30647742212285,
125.589780547671));
#40163=CARTESIAN_POINT('Ctrl Pts',(-4.06451990932337,-5.41317685024397,
125.597990945734));
#40164=CARTESIAN_POINT('Ctrl Pts',(-3.92216479027695,-5.51442765460857,
125.606201343796));
#40165=CARTESIAN_POINT('Ctrl Pts',(-3.77990195090861,-5.61561282458156,
125.614406419585));
#40166=CARTESIAN_POINT('Ctrl Pts',(-3.63362686027734,-5.71135619935031,
125.622611495374));
#40167=CARTESIAN_POINT('Ctrl Pts',(-3.48379638847768,-5.80133189221492,
125.630816571162));
#40168=CARTESIAN_POINT('Ctrl Pts',(-3.33403307625314,-5.89126725463651,
125.639017969132));
#40169=CARTESIAN_POINT('Ctrl Pts',(-3.18071786440322,-5.97543990173833,
125.647219367101));
#40170=CARTESIAN_POINT('Ctrl Pts',(-3.02433618793491,-6.05356751200045,
125.655420765071));
#40171=CARTESIAN_POINT('Ctrl Pts',(-2.86796676058128,-6.13168900265778,
125.663621520639));
#40172=CARTESIAN_POINT('Ctrl Pts',(-2.70853166340291,-6.20376623182548,
125.671822276206));
#40173=CARTESIAN_POINT('Ctrl Pts',(-2.54654082793056,-6.2695628884064,125.680023031774));
#40174=CARTESIAN_POINT('Ctrl Pts',(-2.38455081529468,-6.33535921077156,
125.688223745686));
#40175=CARTESIAN_POINT('Ctrl Pts',(-2.22000542185178,-6.39487488824521,
125.696424459597));
#40176=CARTESIAN_POINT('Ctrl Pts',(-2.0534343344751,-6.44792186940869,125.704625173509));
#40177=CARTESIAN_POINT('Ctrl Pts',(-1.8868339063714,-6.50097819455268,125.712827331939));
#40178=CARTESIAN_POINT('Ctrl Pts',(-1.71820741491762,-6.5475634445163,125.721029490369));
#40179=CARTESIAN_POINT('Ctrl Pts',(-1.5480995243689,-6.58753951507304,125.729231648798));
#40180=CARTESIAN_POINT('Ctrl Pts',(-1.37793084199032,-6.62752987196578,
125.737436738451));
#40181=CARTESIAN_POINT('Ctrl Pts',(-1.20628005454706,-6.66090626240241,
125.745641828104));
#40182=CARTESIAN_POINT('Ctrl Pts',(-1.03370188142339,-6.68758173186256,
125.753846917757));
#40183=CARTESIAN_POINT('Ctrl Pts',(-0.860926558141236,-6.71428767489266,
125.762061380755));
#40184=CARTESIAN_POINT('Ctrl Pts',(-0.687222087152422,-6.73427734878347,
125.770275843753));
#40185=CARTESIAN_POINT('Ctrl Pts',(-0.513149240485588,-6.74751560627977,
125.77849030675));
#40186=CARTESIAN_POINT('Ctrl Pts',(-0.338973261159087,-6.76076170702521,
125.786709636558));
#40187=CARTESIAN_POINT('Ctrl Pts',(-0.164428828620265,-6.76724840455046,
125.794928966365));
#40188=CARTESIAN_POINT('Ctrl Pts',(0.00992352496164936,-6.76699272377711,
125.803148296173));
#40189=CARTESIAN_POINT('Ctrl Pts',(0.184546026944872,-6.7667366468419,125.811380361333));
#40190=CARTESIAN_POINT('Ctrl Pts',(0.35897549738885,-6.75971732901395,125.819612426494));
#40191=CARTESIAN_POINT('Ctrl Pts',(0.532655418187711,-6.74600379524614,
125.827844491655));
#40192=CARTESIAN_POINT('Ctrl Pts',(0.688771401904405,-6.73367708640986,
125.835244062916));
#40193=CARTESIAN_POINT('Ctrl Pts',(0.844281684288117,-6.71594237343187,
125.842643634177));
#40194=CARTESIAN_POINT('Ctrl Pts',(0.998790178529936,-6.69288481742157,
125.850043205438));
#40195=CARTESIAN_POINT('Ctrl Pts',(1.1690821527284,-6.66747186681032,125.858198663845));
#40196=CARTESIAN_POINT('Ctrl Pts',(1.33868135385016,-6.63551392819872,125.866354122252));
#40197=CARTESIAN_POINT('Ctrl Pts',(1.50704013197942,-6.59705381519686,125.874509580658));
#40198=CARTESIAN_POINT('Ctrl Pts',(1.67519399534527,-6.55864051320803,125.8826551128));
#40199=CARTESIAN_POINT('Ctrl Pts',(1.8421100885522,-6.51374087051423,125.890800644942));
#40200=CARTESIAN_POINT('Ctrl Pts',(2.00724606716769,-6.46244939831949,125.898946177084));
#40201=CARTESIAN_POINT('Ctrl Pts',(2.17221577837386,-6.41120956902094,125.907083507885));
#40202=CARTESIAN_POINT('Ctrl Pts',(2.33540859671976,-6.35359083001216,125.915220838685));
#40203=CARTESIAN_POINT('Ctrl Pts',(2.49629256009574,-6.28973866344307,125.923358169486));
#40204=CARTESIAN_POINT('Ctrl Pts',(2.65704834747318,-6.22593736779386,125.931489017288));
#40205=CARTESIAN_POINT('Ctrl Pts',(2.81549860433318,-6.15591266703359,125.93961986509));
#40206=CARTESIAN_POINT('Ctrl Pts',(2.9711267303755,-6.07985978062391,125.947750712892));
#40207=CARTESIAN_POINT('Ctrl Pts',(3.12666356011906,-6.00385150920263,125.955876790886));
#40208=CARTESIAN_POINT('Ctrl Pts',(3.27938122847468,-5.92182225472123,125.964002868879));
#40209=CARTESIAN_POINT('Ctrl Pts',(3.42878332811567,-5.83401524585221,125.972128946873));
#40210=CARTESIAN_POINT('Ctrl Pts',(3.57871518031466,-5.74589688936713,125.980283838455));
#40211=CARTESIAN_POINT('Ctrl Pts',(3.72530756450427,-5.65195987244917,125.988438730038));
#40212=CARTESIAN_POINT('Ctrl Pts',(3.86808338058065,-5.55249673218056,125.99659362162));
#40213=CARTESIAN_POINT('Ctrl Pts',(4.01030242089413,-5.45342146338294,126.004716711976));
#40214=CARTESIAN_POINT('Ctrl Pts',(4.14873431378981,-5.34886331835999,126.012839802332));
#40215=CARTESIAN_POINT('Ctrl Pts',(4.28293658568011,-5.23915481762496,126.020962892689));
#40216=CARTESIAN_POINT('Ctrl Pts',(4.4171493957457,-5.12943770207741,126.029086620907));
#40217=CARTESIAN_POINT('Ctrl Pts',(4.54713163998007,-5.01456965674763,126.037210349126));
#40218=CARTESIAN_POINT('Ctrl Pts',(4.67247415664623,-4.89492331456511,126.045334077344));
#40219=CARTESIAN_POINT('Ctrl Pts',(4.79785036204331,-4.7752448146317,126.053459989004));
#40220=CARTESIAN_POINT('Ctrl Pts',(4.91858409228166,-4.65078571309535,126.061585900665));
#40221=CARTESIAN_POINT('Ctrl Pts',(5.03430329756695,-4.52195525277579,126.069711812325));
#40222=CARTESIAN_POINT('Ctrl Pts',(5.1507625392001,-4.39230090826939,126.077889690035));
#40223=CARTESIAN_POINT('Ctrl Pts',(5.26214264545633,-4.25821937975416,126.086067567745));
#40224=CARTESIAN_POINT('Ctrl Pts',(5.36810629527053,-4.12016065253249,126.094245445455));
#40225=CARTESIAN_POINT('Ctrl Pts',(5.47356420356573,-3.98276084967344,126.102384291929));
#40226=CARTESIAN_POINT('Ctrl Pts',(5.5736570840351,-3.84142206365063,126.110523138402));
#40227=CARTESIAN_POINT('Ctrl Pts',(5.66809683140575,-3.69661565621964,126.118661984875));
#40228=CARTESIAN_POINT('Ctrl Pts',(5.76321593182907,-3.55076758277752,126.126859378204));
#40229=CARTESIAN_POINT('Ctrl Pts',(5.85260006682131,-3.40140213526468,126.135056771532));
#40230=CARTESIAN_POINT('Ctrl Pts',(5.93600286567616,-3.24902431180261,126.143254164861));
#40231=CARTESIAN_POINT('Ctrl Pts',(6.01940566453096,-3.09664648834064,126.151451558189));
#40232=CARTESIAN_POINT('Ctrl Pts',(6.09682701594818,-2.9412566493515,126.159648951518));
#40233=CARTESIAN_POINT('Ctrl Pts',(6.16807069414603,-2.78337796786872,126.167846344846));
#40234=CARTESIAN_POINT('Ctrl Pts',(6.23956481274092,-2.62494430100793,126.176072554183));
#40235=CARTESIAN_POINT('Ctrl Pts',(6.30505063601268,-2.46353278482734,126.18429876352));
#40236=CARTESIAN_POINT('Ctrl Pts',(6.36427136386523,-2.2996388862352,126.192524972857));
#40237=CARTESIAN_POINT('Ctrl Pts',(6.42342555976696,-2.13592911541713,126.2007419404));
#40238=CARTESIAN_POINT('Ctrl Pts',(6.47632855517849,-1.96974284977542,126.208958907943));
#40239=CARTESIAN_POINT('Ctrl Pts',(6.52277033073405,-1.80159823836937,126.217175875487));
#40240=CARTESIAN_POINT('Ctrl Pts',(6.56916925218075,-1.63360878226038,126.22538526083));
#40241=CARTESIAN_POINT('Ctrl Pts',(6.60911873260524,-1.46366492273824,126.233594646173));
#40242=CARTESIAN_POINT('Ctrl Pts',(6.64245754800751,-1.2923028758453,126.241804031517));
#40243=CARTESIAN_POINT('Ctrl Pts',(6.67577228926573,-1.12106457043968,126.250007488817));
#40244=CARTESIAN_POINT('Ctrl Pts',(6.70248580547753,-0.948410468066173,
126.258210946118));
#40245=CARTESIAN_POINT('Ctrl Pts',(6.72248721792287,-0.774890059856023,
126.266414403419));
#40246=CARTESIAN_POINT('Ctrl Pts',(6.74247819947153,-0.601460143927614,
126.27461358255));
#40247=CARTESIAN_POINT('Ctrl Pts',(6.75576400973546,-0.42716517762927,126.282812761682));
#40248=CARTESIAN_POINT('Ctrl Pts',(6.76228518536541,-0.252563005579774,
126.291011940814));
#40249=CARTESIAN_POINT('Ctrl Pts',(6.76880513226528,-0.0779937323438108,
126.299209575044));
#40250=CARTESIAN_POINT('Ctrl Pts',(6.76856296382229,0.0968822735593504,
126.307407209274));
#40251=CARTESIAN_POINT('Ctrl Pts',(6.76155121244582,0.271503593848233,126.315604843504));
#40252=CARTESIAN_POINT('Ctrl Pts',(6.75453996718524,0.446112309778875,126.323801886019));
#40253=CARTESIAN_POINT('Ctrl Pts',(6.74076012564427,0.620466018281871,126.331998928535));
#40254=CARTESIAN_POINT('Ctrl Pts',(6.7202563349705,0.794004906967783,126.34019597105));
#40255=CARTESIAN_POINT('Ctrl Pts',(6.69975029775319,0.967562809828921,126.348393911693));
#40256=CARTESIAN_POINT('Ctrl Pts',(6.67251888572896,1.14030535872973,126.356591852336));
#40257=CARTESIAN_POINT('Ctrl Pts',(6.63865845961037,1.31167940314837,126.364789792979));
#40258=CARTESIAN_POINT('Ctrl Pts',(6.60478816939993,1.48310337160845,126.372990121815));
#40259=CARTESIAN_POINT('Ctrl Pts',(6.56428508800642,1.65315768969983,126.381190450651));
#40260=CARTESIAN_POINT('Ctrl Pts',(6.51729638575349,1.82130085934328,126.389390779487));
#40261=CARTESIAN_POINT('Ctrl Pts',(6.47025872005376,1.98961923853169,126.397599653278));
#40262=CARTESIAN_POINT('Ctrl Pts',(6.41672202832614,2.15602214472305,126.40580852707));
#40263=CARTESIAN_POINT('Ctrl Pts',(6.35688324221719,2.31998371649852,126.414017400861));
#40264=CARTESIAN_POINT('Ctrl Pts',(6.29701234129188,2.48403328464072,126.422230680265));
#40265=CARTESIAN_POINT('Ctrl Pts',(6.23083273911924,2.64563857475918,126.430443959668));
#40266=CARTESIAN_POINT('Ctrl Pts',(6.15858891991479,2.80429519050737,126.438657239071));
#40267=CARTESIAN_POINT('Ctrl Pts',(6.08623943277005,2.96318386649247,126.446882531687));
#40268=CARTESIAN_POINT('Ctrl Pts',(6.00780816389592,3.11911492864928,126.455107824302));
#40269=CARTESIAN_POINT('Ctrl Pts',(5.92358543184648,3.27160887509741,126.463333116918));
#40270=CARTESIAN_POINT('Ctrl Pts',(5.84741608791609,3.40952133141019,126.47077190603));
#40271=CARTESIAN_POINT('Ctrl Pts',(5.76651056850129,3.54462275421643,126.478210695142));
#40272=CARTESIAN_POINT('Ctrl Pts',(5.68111296843999,3.67658053628953,126.485649484254));
#40273=CARTESIAN_POINT('Ctrl Pts',(5.58667845118299,3.82250231207049,126.4938754585));
#40274=CARTESIAN_POINT('Ctrl Pts',(5.48648624044273,3.96498731542591,126.502101432746));
#40275=CARTESIAN_POINT('Ctrl Pts',(5.38081365457187,4.10355131742896,126.510327406992));
#40276=CARTESIAN_POINT('Ctrl Pts',(5.27525496088637,4.24196597741609,126.518544515417));
#40277=CARTESIAN_POINT('Ctrl Pts',(5.16422786736725,4.37646776719986,126.526761623842));
#40278=CARTESIAN_POINT('Ctrl Pts',(5.04805414095819,4.50659942639179,126.534978732268));
#40279=CARTESIAN_POINT('Ctrl Pts',(4.93198449783409,4.63661449699711,126.543188478756));
#40280=CARTESIAN_POINT('Ctrl Pts',(4.8107776411001,4.76226696770519,126.551398225245));
#40281=CARTESIAN_POINT('Ctrl Pts',(4.68479699099187,4.88313077371409,126.559607971733));
#40282=CARTESIAN_POINT('Ctrl Pts',(4.55891905785163,5.00389603471879,126.567811024493));
#40283=CARTESIAN_POINT('Ctrl Pts',(4.42827534534742,5.11988016414388,126.576014077253));
#40284=CARTESIAN_POINT('Ctrl Pts',(4.29326759855843,5.23069233726935,126.584217130013));
#40285=CARTESIAN_POINT('Ctrl Pts',(4.1583245922381,5.34145137246614,126.592416249151));
#40286=CARTESIAN_POINT('Ctrl Pts',(4.01902199568574,5.44704316348565,126.600615368289));
#40287=CARTESIAN_POINT('Ctrl Pts',(3.87579647803769,5.54711552618391,126.608814487427));
#40288=CARTESIAN_POINT('Ctrl Pts',(3.7326042956021,5.64716459740782,126.61701169825));
#40289=CARTESIAN_POINT('Ctrl Pts',(3.58549130240188,5.74169659109429,126.625208909073));
#40290=CARTESIAN_POINT('Ctrl Pts',(3.43492527580759,5.83040113110737,126.633406119896));
#40291=CARTESIAN_POINT('Ctrl Pts',(3.3247914955315,5.89528539843029,126.639402092799));
#40292=CARTESIAN_POINT('Ctrl Pts',(3.21281087344299,5.95705259306496,126.645398065703));
#40293=CARTESIAN_POINT('Ctrl Pts',(3.09917575053261,6.01559628526638,126.651394038606));
#40294=CARTESIAN_POINT('Origin',(0.,0.,-3.69717978381041));
#40295=CARTESIAN_POINT('',(3.09917575053253,6.01559628526642,129.045751582742));
#40296=CARTESIAN_POINT('',(3.09917575053256,6.01559628526641,128.651204297413));
#40297=CARTESIAN_POINT('',(3.09917575053259,6.01559628526639,-3.69717978381041));
#40298=CARTESIAN_POINT('',(-6.767,7.58899778956212E-12,127.69717978381));
#40299=CARTESIAN_POINT('Ctrl Pts',(-6.767,7.58899730750792E-12,127.69717978381));
#40300=CARTESIAN_POINT('Ctrl Pts',(-6.76700000000021,-0.186007249408207,
127.705929295616));
#40301=CARTESIAN_POINT('Ctrl Pts',(-6.75932637295479,-0.372014355520188,
127.714678807422));
#40302=CARTESIAN_POINT('Ctrl Pts',(-6.74400518266988,-0.557389537147837,
127.723428319228));
#40303=CARTESIAN_POINT('Ctrl Pts',(-6.72868405709723,-0.742763935804457,
127.732177794078));
#40304=CARTESIAN_POINT('Ctrl Pts',(-6.70571545653084,-0.927506129688376,
127.740927268929));
#40305=CARTESIAN_POINT('Ctrl Pts',(-6.67517739415756,-1.11098863924338,
127.74967674378));
#40306=CARTESIAN_POINT('Ctrl Pts',(-6.64463945823188,-1.29447038906054,
127.758426182402));
#40307=CARTESIAN_POINT('Ctrl Pts',(-6.60653217027252,-1.47669218227794,
127.767175621024));
#40308=CARTESIAN_POINT('Ctrl Pts',(-6.56098496116812,-1.65703510503724,
127.775925059646));
#40309=CARTESIAN_POINT('Ctrl Pts',(-6.51543793687625,-1.8373772960364,127.784674462766));
#40310=CARTESIAN_POINT('Ctrl Pts',(-6.46245112202753,-2.01584035396688,
127.793423865886));
#40311=CARTESIAN_POINT('Ctrl Pts',(-6.40220448416362,-2.19181813637795,
127.802173269006));
#40312=CARTESIAN_POINT('Ctrl Pts',(-6.34195808575317,-2.36779521935593,
127.810922637352));
#40313=CARTESIAN_POINT('Ctrl Pts',(-6.27445201489377,-2.54128677544476,
127.819672005697));
#40314=CARTESIAN_POINT('Ctrl Pts',(-6.19991555136338,-2.71170355237489,
127.828421374042));
#40315=CARTESIAN_POINT('Ctrl Pts',(-6.12537937789207,-2.88211966612712,
127.837170708339));
#40316=CARTESIAN_POINT('Ctrl Pts',(-6.04381298133802,-3.04946076210077,
127.845920042636));
#40317=CARTESIAN_POINT('Ctrl Pts',(-5.95549339426508,-3.21315848206481,
127.854669376933));
#40318=CARTESIAN_POINT('Ctrl Pts',(-5.86717414355366,-3.3768555785928,127.863418677909));
#40319=CARTESIAN_POINT('Ctrl Pts',(-5.77210188986446,-3.53690907466972,
127.872167978884));
#40320=CARTESIAN_POINT('Ctrl Pts',(-5.67059953467278,-3.69277536784583,
127.88091727986));
#40321=CARTESIAN_POINT('Ctrl Pts',(-5.56909755761985,-3.84864108035475,
127.889666548241));
#40322=CARTESIAN_POINT('Ctrl Pts',(-5.46116568338299,-4.00031938103966,
127.898415816621));
#40323=CARTESIAN_POINT('Ctrl Pts',(-5.34717048686353,-4.14729511662911,
127.907165085002));
#40324=CARTESIAN_POINT('Ctrl Pts',(-5.23317570555759,-4.29427031687747,
127.915914321515));
#40325=CARTESIAN_POINT('Ctrl Pts',(-5.11311782179048,-4.4365427598685,127.924663558027));
#40326=CARTESIAN_POINT('Ctrl Pts',(-4.98740459172257,-4.57362924147384,
127.93341279454));
#40327=CARTESIAN_POINT('Ctrl Pts',(-4.86169180911079,-4.7107152351418,127.942161999911));
#40328=CARTESIAN_POINT('Ctrl Pts',(-4.73032391415684,-4.84261509316276,
127.950911205282));
#40329=CARTESIAN_POINT('Ctrl Pts',(-4.59374707237551,-4.96888084331285,
127.959660410653));
#40330=CARTESIAN_POINT('Ctrl Pts',(-4.45717070537675,-5.09514615452485,
127.96840958561));
#40331=CARTESIAN_POINT('Ctrl Pts',(-4.31538563819798,-5.21577720253393,
127.977158760566));
#40332=CARTESIAN_POINT('Ctrl Pts',(-4.16887341290952,-5.33036429028412,
127.985907935522));
#40333=CARTESIAN_POINT('Ctrl Pts',(-4.02236168477642,-5.44495098920953,
127.99465708079));
#40334=CARTESIAN_POINT('Ctrl Pts',(-3.8711230563474,-5.55349359238549,128.003406226058));
#40335=CARTESIAN_POINT('Ctrl Pts',(-3.71567117317031,-5.65562346102277,
128.012155371326));
#40336=CARTESIAN_POINT('Ctrl Pts',(-3.56021980457621,-5.75775299158571,
128.020904487632));
#40337=CARTESIAN_POINT('Ctrl Pts',(-3.4005554486273,-5.85346967275154,128.029653603938));
#40338=CARTESIAN_POINT('Ctrl Pts',(-3.23722036323768,-5.94244842803363,
128.038402720244));
#40339=CARTESIAN_POINT('Ctrl Pts',(-3.0738858049641,-6.0314268961629,128.047151808315));
#40340=CARTESIAN_POINT('Ctrl Pts',(-2.90688079258068,-6.11366734484651,
128.055900896386));
#40341=CARTESIAN_POINT('Ctrl Pts',(-2.73677251094973,-6.18889046787144,
128.064649984457));
#40342=CARTESIAN_POINT('Ctrl Pts',(-2.56666476416983,-6.26411335438133,
128.073399045019));
#40343=CARTESIAN_POINT('Ctrl Pts',(-2.39345402972409,-6.33231884350172,
128.082148105582));
#40344=CARTESIAN_POINT('Ctrl Pts',(-2.21772856474332,-6.39327529620941,
128.090897166144));
#40345=CARTESIAN_POINT('Ctrl Pts',(-2.04200363768575,-6.45423156231985,
128.099646199924));
#40346=CARTESIAN_POINT('Ctrl Pts',(-1.8637642662041,-6.50793874251965,128.108395233704));
#40347=CARTESIAN_POINT('Ctrl Pts',(-1.68361578195017,-6.55421443796038,
128.117144267484));
#40348=CARTESIAN_POINT('Ctrl Pts',(-1.50346783420211,-6.60048999558601,
128.125893275208));
#40349=CARTESIAN_POINT('Ctrl Pts',(-1.32141106257604,-6.63933404145424,
128.134642282932));
#40350=CARTESIAN_POINT('Ctrl Pts',(-1.13806375959417,-6.67061465526966,
128.143391290657));
#40351=CARTESIAN_POINT('Ctrl Pts',(-0.954716987422707,-6.7018951785243,
128.152140273051));
#40352=CARTESIAN_POINT('Ctrl Pts',(-0.770079973813257,-6.7256122653579,
128.160889255446));
#40353=CARTESIAN_POINT('Ctrl Pts',(-0.584779770555658,-6.74168536939754,
128.169638237841));
#40354=CARTESIAN_POINT('Ctrl Pts',(-0.391490647557111,-6.75845143942375,
128.178764418517));
#40355=CARTESIAN_POINT('Ctrl Pts',(-0.197480213107528,-6.76689975924017,
128.187890599193));
#40356=CARTESIAN_POINT('Ctrl Pts',(-0.00346532630097921,-6.76699911271707,
128.197016779869));
#40357=CARTESIAN_POINT('Ctrl Pts',(0.184486595292832,-6.76709536139782,
128.205857767399));
#40358=CARTESIAN_POINT('Ctrl Pts',(0.372442378181968,-6.75935659726788,
128.214698754929));
#40359=CARTESIAN_POINT('Ctrl Pts',(0.559750217718792,-6.74380965729044,
128.223539742459));
#40360=CARTESIAN_POINT('Ctrl Pts',(0.745129914454466,-6.7284227571729,128.232289721057));
#40361=CARTESIAN_POINT('Ctrl Pts',(0.929874656310905,-6.70538772273518,
128.241039699655));
#40362=CARTESIAN_POINT('Ctrl Pts',(1.11335688289451,-6.67478280180797,128.249789678252));
#40363=CARTESIAN_POINT('Ctrl Pts',(1.29683723118518,-6.64417819418089,128.258539567277));
#40364=CARTESIAN_POINT('Ctrl Pts',(1.47905480729886,-6.60600390230153,128.267289456302));
#40365=CARTESIAN_POINT('Ctrl Pts',(1.65939064804448,-6.56038959797225,128.276039345327));
#40366=CARTESIAN_POINT('Ctrl Pts',(1.83972470263913,-6.51477574543356,128.284789147688));
#40367=CARTESIAN_POINT('Ctrl Pts',(2.01817678125503,-6.46172209820208,128.293538950049));
#40368=CARTESIAN_POINT('Ctrl Pts',(2.19414072347343,-6.4014088672413,128.30228875241));
#40369=CARTESIAN_POINT('Ctrl Pts',(2.37010298131771,-6.34109621361496,128.311038471016));
#40370=CARTESIAN_POINT('Ctrl Pts',(2.54357687926597,-6.27352420826099,128.319788189621));
#40371=CARTESIAN_POINT('Ctrl Pts',(2.71397317789666,-6.1989223732563,128.328537908227));
#40372=CARTESIAN_POINT('Ctrl Pts',(2.88436790206904,-6.12432122757104,128.337287545985));
#40373=CARTESIAN_POINT('Ctrl Pts',(3.05168482125968,-6.04269049717563,128.346037183743));
#40374=CARTESIAN_POINT('Ctrl Pts',(3.21535561997108,-5.95430745235081,128.354786821501));
#40375=CARTESIAN_POINT('Ctrl Pts',(3.37902496075003,-5.86592519481676,128.36353638132));
#40376=CARTESIAN_POINT('Ctrl Pts',(3.53904799384601,-5.770790879404,128.372285941139));
#40377=CARTESIAN_POINT('Ctrl Pts',(3.69488118814714,-5.669227637472,128.381035500958));
#40378=CARTESIAN_POINT('Ctrl Pts',(3.85071304610559,-5.56766526649241,128.389784985746));
#40379=CARTESIAN_POINT('Ctrl Pts',(4.0023548970569,-5.45967423580917,128.398534470533));
#40380=CARTESIAN_POINT('Ctrl Pts',(4.14929168607374,-5.34562133936546,128.407283955321));
#40381=CARTESIAN_POINT('Ctrl Pts',(4.29622726385473,-5.23156938308763,128.416033367984));
#40382=CARTESIAN_POINT('Ctrl Pts',(4.4384576309178,-5.11145583677451,128.424782780647));
#40383=CARTESIAN_POINT('Ctrl Pts',(4.57549970660673,-4.98568866204476,128.433532193311));
#40384=CARTESIAN_POINT('Ctrl Pts',(4.71254069815016,-4.85992248226432,128.442281536757));
#40385=CARTESIAN_POINT('Ctrl Pts',(4.84439326931045,-4.72850295734278,128.451030880203));
#40386=CARTESIAN_POINT('Ctrl Pts',(4.97060959434439,-4.59187644221962,128.45978022365));
#40387=CARTESIAN_POINT('Ctrl Pts',(5.09682496280269,-4.45525096256946,128.468529500786));
#40388=CARTESIAN_POINT('Ctrl Pts',(5.21740397615605,-4.3134187821861,128.477278777922));
#40389=CARTESIAN_POINT('Ctrl Pts',(5.33193710451712,-4.16686161438962,128.486028055058));
#40390=CARTESIAN_POINT('Ctrl Pts',(5.44646940289165,-4.02030550864809,128.494777268791));
#40391=CARTESIAN_POINT('Ctrl Pts',(5.55495572749452,-3.86902470980439,128.503526482524));
#40392=CARTESIAN_POINT('Ctrl Pts',(5.65702762491248,-3.71353301466098,128.512275696257));
#40393=CARTESIAN_POINT('Ctrl Pts',(5.75909881654957,-3.55804239467212,128.521024849494));
#40394=CARTESIAN_POINT('Ctrl Pts',(5.85475551250595,-3.39834117619875,128.52977400273));
#40395=CARTESIAN_POINT('Ctrl Pts',(5.94367283727918,-3.23497174692294,128.538523155966));
#40396=CARTESIAN_POINT('Ctrl Pts',(6.03258957676146,-3.07160339301292,128.547272251611));
#40397=CARTESIAN_POINT('Ctrl Pts',(6.11476689685129,-2.90456712829831,128.556021347257));
#40398=CARTESIAN_POINT('Ctrl Pts',(6.18992570525116,-2.73443024476232,128.564770442902));
#40399=CARTESIAN_POINT('Ctrl Pts',(6.2650840438857,-2.56429442463343,128.573519483863));
#40400=CARTESIAN_POINT('Ctrl Pts',(6.33322384283203,-2.39105828656292,128.582268524824));
#40401=CARTESIAN_POINT('Ctrl Pts',(6.39411368719935,-2.21531017132365,128.591017565785));
#40402=CARTESIAN_POINT('Ctrl Pts',(6.45500317120798,-2.03956309619804,128.599766554968));
#40403=CARTESIAN_POINT('Ctrl Pts',(6.50864269269989,-1.86130434438929,128.60851554415));
#40404=CARTESIAN_POINT('Ctrl Pts',(6.55485008446256,-1.68113930720245,128.617264533333));
#40405=CARTESIAN_POINT('Ctrl Pts',(6.60199664749336,-1.49731239212138,128.626191346862));
#40406=CARTESIAN_POINT('Ctrl Pts',(6.64140563640849,-1.31150116499966,128.635118160391));
#40407=CARTESIAN_POINT('Ctrl Pts',(6.67293772282123,-1.12436255155951,128.644044973921));
#40408=CARTESIAN_POINT('Ctrl Pts',(6.70384494949829,-0.940932395054325,
128.652794888076));
#40409=CARTESIAN_POINT('Ctrl Pts',(6.72718449348896,-0.756227260509767,
128.661544802232));
#40410=CARTESIAN_POINT('Ctrl Pts',(6.74287707373906,-0.570874564544813,
128.670294716387));
#40411=CARTESIAN_POINT('Ctrl Pts',(6.75856934538653,-0.385525513635557,
128.679044458471));
#40412=CARTESIAN_POINT('Ctrl Pts',(6.76661493004094,-0.199529212421269,
128.687794200555));
#40413=CARTESIAN_POINT('Ctrl Pts',(6.76698649908906,-0.0135174386034205,
128.696543942639));
#40414=CARTESIAN_POINT('Ctrl Pts',(6.76735806132397,0.172490924442862,128.705293524285));
#40415=CARTESIAN_POINT('Ctrl Pts',(6.76005588896304,0.35851447289857,128.714043105931));
#40416=CARTESIAN_POINT('Ctrl Pts',(6.74510478454607,0.543921359659458,128.722792687577));
#40417=CARTESIAN_POINT('Ctrl Pts',(6.73015393440717,0.729325093147752,128.731542120416));
#40418=CARTESIAN_POINT('Ctrl Pts',(6.70755443556933,0.914111900253724,128.740291553255));
#40419=CARTESIAN_POINT('Ctrl Pts',(6.67738304682361,1.09765415591282,128.749040986094));
#40420=CARTESIAN_POINT('Ctrl Pts',(6.6472121311191,1.28119353391013,128.757790281755));
#40421=CARTESIAN_POINT('Ctrl Pts',(6.60946960955552,1.4634881167239,128.766539577417));
#40422=CARTESIAN_POINT('Ctrl Pts',(6.5642836699125,1.64391876347956,128.775288873078));
#40423=CARTESIAN_POINT('Ctrl Pts',(6.51909837867792,1.82434682109449,128.784038043189));
#40424=CARTESIAN_POINT('Ctrl Pts',(6.46646995272004,2.00291071820178,128.7927872133));
#40425=CARTESIAN_POINT('Ctrl Pts',(6.4065771328164,2.17900400212436,128.801536383411));
#40426=CARTESIAN_POINT('Ctrl Pts',(6.34668509279158,2.35509499309393,128.810285439596));
#40427=CARTESIAN_POINT('Ctrl Pts',(6.27952894037632,2.52871516397859,128.819034495782));
#40428=CARTESIAN_POINT('Ctrl Pts',(6.20533675061561,2.69927486771158,128.827783551968));
#40429=CARTESIAN_POINT('Ctrl Pts',(6.12832117908032,2.87632521635678,128.83686555325));
#40430=CARTESIAN_POINT('Ctrl Pts',(6.04372366626195,3.05007728919768,128.845947554532));
#40431=CARTESIAN_POINT('Ctrl Pts',(5.95185378007983,3.21989527477982,128.855029555815));
#40432=CARTESIAN_POINT('Ctrl Pts',(5.86334450817489,3.38350129286548,128.863779336122));
#40433=CARTESIAN_POINT('Ctrl Pts',(5.76808562057375,3.54345567124769,128.872529116429));
#40434=CARTESIAN_POINT('Ctrl Pts',(5.66640068804604,3.69921508465126,128.881278896736));
#40435=CARTESIAN_POINT('Ctrl Pts',(5.56471941108052,3.85496889852097,128.89002836249));
#40436=CARTESIAN_POINT('Ctrl Pts',(5.45661270815251,4.00652780919449,128.898777828243));
#40437=CARTESIAN_POINT('Ctrl Pts',(5.34244776449261,4.1533770456904,128.907527293997));
#40438=CARTESIAN_POINT('Ctrl Pts',(5.2282863181974,4.30022178356074,128.916276491716));
#40439=CARTESIAN_POINT('Ctrl Pts',(5.10806717844212,4.44235690972516,128.925025689436));
#40440=CARTESIAN_POINT('Ctrl Pts',(4.98219864544858,4.57929969070494,128.933774887155));
#40441=CARTESIAN_POINT('Ctrl Pts',(4.85633329944169,4.71623900429852,128.942523863346));
#40442=CARTESIAN_POINT('Ctrl Pts',(4.72481904033798,4.84798602483471,128.951272839536));
#40443=CARTESIAN_POINT('Ctrl Pts',(4.58810250737353,4.97409332258983,128.960021815726));
#40444=CARTESIAN_POINT('Ctrl Pts',(4.45137708685805,5.10020881821993,128.968771360662));
#40445=CARTESIAN_POINT('Ctrl Pts',(4.30944892636222,5.22068366307792,128.977520905598));
#40446=CARTESIAN_POINT('Ctrl Pts',(4.1628000946684,5.33510865604711,128.986270450535));
#40447=CARTESIAN_POINT('Ctrl Pts',(4.01615988348958,5.44952692272767,128.995019481143));
#40448=CARTESIAN_POINT('Ctrl Pts',(3.8647997823239,5.55789587288516,129.003768511751));
#40449=CARTESIAN_POINT('Ctrl Pts',(3.70923383581215,5.65984746713781,129.012517542359));
#40450=CARTESIAN_POINT('Ctrl Pts',(3.55366577799683,5.76180044505295,129.021266691707));
#40451=CARTESIAN_POINT('Ctrl Pts',(3.39389200026977,5.8573357357098,129.030015841055));
#40452=CARTESIAN_POINT('Ctrl Pts',(3.23045513626172,5.94612887621857,129.038764990404));
#40453=CARTESIAN_POINT('Ctrl Pts',(3.18695122151664,5.96976399206643,129.041093854517));
#40454=CARTESIAN_POINT('Ctrl Pts',(3.14318791262705,5.99292165435312,129.043422718629));
#40455=CARTESIAN_POINT('Ctrl Pts',(3.09917575053253,6.01559628526642,129.045751582742));
#40456=CARTESIAN_POINT('Ctrl Pts',(3.09917575053273,6.01559628526631,127.045911902629));
#40457=CARTESIAN_POINT('Ctrl Pts',(2.94398502489705,6.09554901327362,127.05411480057));
#40458=CARTESIAN_POINT('Ctrl Pts',(2.78560179809225,6.16954220727552,127.062317698511));
#40459=CARTESIAN_POINT('Ctrl Pts',(2.62452527368248,6.23731962366864,127.070520596452));
#40460=CARTESIAN_POINT('Ctrl Pts',(2.46249362782818,6.30549893390749,127.078772134402));
#40461=CARTESIAN_POINT('Ctrl Pts',(2.29773695407367,6.3673883226108,127.087023672353));
#40462=CARTESIAN_POINT('Ctrl Pts',(2.13078641942083,6.42277496373739,127.095275210304));
#40463=CARTESIAN_POINT('Ctrl Pts',(1.96490192961397,6.47780793936998,127.103474058938));
#40464=CARTESIAN_POINT('Ctrl Pts',(1.79685186523018,6.52642087548502,127.111672907573));
#40465=CARTESIAN_POINT('Ctrl Pts',(1.62717491405476,6.56845421686647,127.119871756207));
#40466=CARTESIAN_POINT('Ctrl Pts',(1.45749451425469,6.61048841256087,127.12807077148));
#40467=CARTESIAN_POINT('Ctrl Pts',(1.28618750966292,6.6459426607097,127.136269786754));
#40468=CARTESIAN_POINT('Ctrl Pts',(1.11380504865354,6.67470803208604,127.144468802027));
#40469=CARTESIAN_POINT('Ctrl Pts',(0.941387813069357,6.70347920627754,127.152669471281));
#40470=CARTESIAN_POINT('Ctrl Pts',(0.767895042453905,6.72555875720563,127.160870140535));
#40471=CARTESIAN_POINT('Ctrl Pts',(0.593885370547981,6.74088934537937,127.169070809789));
#40472=CARTESIAN_POINT('Ctrl Pts',(0.417968350331196,6.75638797462311,127.177361367912));
#40473=CARTESIAN_POINT('Ctrl Pts',(0.241523403679143,6.76498877367479,127.185651926035));
#40474=CARTESIAN_POINT('Ctrl Pts',(0.0651295830442705,6.76668657005868,
127.193942484159));
#40475=CARTESIAN_POINT('Ctrl Pts',(-0.109594544721961,6.76836829559323,
127.202154566257));
#40476=CARTESIAN_POINT('Ctrl Pts',(-0.284268152398203,6.76327720213396,
127.210366648356));
#40477=CARTESIAN_POINT('Ctrl Pts',(-0.458332117798099,6.75146063232207,
127.218578730455));
#40478=CARTESIAN_POINT('Ctrl Pts',(-0.634891159568652,6.73947468084608,
127.22690852659));
#40479=CARTESIAN_POINT('Ctrl Pts',(-0.810822565445924,6.72056901307334,
127.235238322726));
#40480=CARTESIAN_POINT('Ctrl Pts',(-0.985552264639139,6.69484695371483,
127.243568118861));
#40481=CARTESIAN_POINT('Ctrl Pts',(-1.16028196383248,6.6691248943563,127.251897914997));
#40482=CARTESIAN_POINT('Ctrl Pts',(-1.3338095928365,6.63658656471674,127.260227711132));
#40483=CARTESIAN_POINT('Ctrl Pts',(-1.50557612075279,6.59738808503934,127.268557507268));
#40484=CARTESIAN_POINT('Ctrl Pts',(-1.68385719114858,6.55670293526335,127.27720322532));
#40485=CARTESIAN_POINT('Ctrl Pts',(-1.86064759279046,6.50875066070558,127.285848943373));
#40486=CARTESIAN_POINT('Ctrl Pts',(-2.0353473042416,6.45365403094375,127.294494661425));
#40487=CARTESIAN_POINT('Ctrl Pts',(-2.20982273686541,6.39862813402635,127.303129280137));
#40488=CARTESIAN_POINT('Ctrl Pts',(-2.38221254190671,6.33647626243224,127.31176389885));
#40489=CARTESIAN_POINT('Ctrl Pts',(-2.55192873554816,6.26737175606199,127.320398517562));
#40490=CARTESIAN_POINT('Ctrl Pts',(-2.72763864585318,6.19582674697676,127.329338077464));
#40491=CARTESIAN_POINT('Ctrl Pts',(-2.90048233561038,6.11682910355213,127.338277637367));
#40492=CARTESIAN_POINT('Ctrl Pts',(-3.06982345566104,6.0306279068662,127.347217197269));
#40493=CARTESIAN_POINT('Ctrl Pts',(-3.23293413282105,5.94759824721095,127.35582785054));
#40494=CARTESIAN_POINT('Ctrl Pts',(-3.392795046907,5.85788576583019,127.36443850381));
#40495=CARTESIAN_POINT('Ctrl Pts',(-3.54885651637059,5.7617624409736,127.373049157081));
#40496=CARTESIAN_POINT('Ctrl Pts',(-3.7047702632137,5.66573010327409,127.381651659792));
#40497=CARTESIAN_POINT('Ctrl Pts',(-3.85689147691732,5.56329918006359,127.390254162503));
#40498=CARTESIAN_POINT('Ctrl Pts',(-4.00469493663627,5.45478757280976,127.398856665214));
#40499=CARTESIAN_POINT('Ctrl Pts',(-4.1523320465364,5.3463980931857,127.407449485982));
#40500=CARTESIAN_POINT('Ctrl Pts',(-4.29566085177274,5.2319417625806,127.416042306749));
#40501=CARTESIAN_POINT('Ctrl Pts',(-4.43418482626982,5.11177991764889,127.424635127517));
#40502=CARTESIAN_POINT('Ctrl Pts',(-4.45051050587183,5.09761829842114,127.425647830475));
#40503=CARTESIAN_POINT('Ctrl Pts',(-4.46676948127015,5.08337748059413,127.426660533433));
#40504=CARTESIAN_POINT('Ctrl Pts',(-4.48296096696515,5.06905809482067,127.427673236391));
#40505=CARTESIAN_POINT('Ctrl Pts',(-4.62038526494443,4.94752313660364,127.436268494151));
#40506=CARTESIAN_POINT('Ctrl Pts',(-4.75278342515784,4.82046811009498,127.444863751911));
#40507=CARTESIAN_POINT('Ctrl Pts',(-4.87973112664818,4.68833799246821,127.453459009671));
#40508=CARTESIAN_POINT('Ctrl Pts',(-5.0067977092774,4.55608414058963,127.462062316525));
#40509=CARTESIAN_POINT('Ctrl Pts',(-5.12840343360427,4.41874593139391,127.47066562338));
#40510=CARTESIAN_POINT('Ctrl Pts',(-5.24416350962005,4.27680232000142,127.479268930234));
#40511=CARTESIAN_POINT('Ctrl Pts',(-5.36472303853082,4.12897367725727,127.488228933174));
#40512=CARTESIAN_POINT('Ctrl Pts',(-5.47894163461994,3.97614991560686,127.497188936114));
#40513=CARTESIAN_POINT('Ctrl Pts',(-5.58643455662435,3.81890533327985,127.506148939054));
#40514=CARTESIAN_POINT('Ctrl Pts',(-5.68993056995751,3.66750757531013,127.514775782259));
#40515=CARTESIAN_POINT('Ctrl Pts',(-5.78719193407782,3.51201210266221,127.523402625464));
#40516=CARTESIAN_POINT('Ctrl Pts',(-5.87792211240528,3.35295699950015,127.532029468668));
#40517=CARTESIAN_POINT('Ctrl Pts',(-5.96873900584857,3.1937498798652,127.540664556954));
#40518=CARTESIAN_POINT('Ctrl Pts',(-6.05301211073054,3.03097660808893,127.549299645241));
#40519=CARTESIAN_POINT('Ctrl Pts',(-6.13049196839731,2.86519758924513,127.557934733527));
#40520=CARTESIAN_POINT('Ctrl Pts',(-6.20808689920134,2.69917235528989,127.566582646652));
#40521=CARTESIAN_POINT('Ctrl Pts',(-6.27886829901054,2.53013273296519,127.575230559777));
#40522=CARTESIAN_POINT('Ctrl Pts',(-6.34263517387559,2.35865810390489,127.583878472902));
#40523=CARTESIAN_POINT('Ctrl Pts',(-6.34978884650288,2.33942126090797,127.584848637106));
#40524=CARTESIAN_POINT('Ctrl Pts',(-6.35685429040264,2.32015378663128,127.58581880131));
#40525=CARTESIAN_POINT('Ctrl Pts',(-6.36383126134657,2.30085650945647,127.586788965515));
#40526=CARTESIAN_POINT('Ctrl Pts',(-6.43074697946329,2.11577745864367,127.596093753357));
#40527=CARTESIAN_POINT('Ctrl Pts',(-6.48963299559788,1.92764419908136,127.605398541199));
#40528=CARTESIAN_POINT('Ctrl Pts',(-6.54023679096125,1.73712167626706,127.614703329041));
#40529=CARTESIAN_POINT('Ctrl Pts',(-6.59070015032034,1.54712789288107,127.623982294171));
#40530=CARTESIAN_POINT('Ctrl Pts',(-6.63292709922294,1.35475824550878,127.633261259301));
#40531=CARTESIAN_POINT('Ctrl Pts',(-6.66671434958378,1.1606932329663,127.642540224431));
#40532=CARTESIAN_POINT('Ctrl Pts',(-6.70031803070446,0.967682593493919,
127.65176877609));
#40533=CARTESIAN_POINT('Ctrl Pts',(-6.72557339603793,0.772995129116876,
127.660997327749));
#40534=CARTESIAN_POINT('Ctrl Pts',(-6.74232838574441,0.577318749726029,
127.670225879408));
#40535=CARTESIAN_POINT('Ctrl Pts',(-6.75864052974762,0.386814229307502,
127.679210514209));
#40536=CARTESIAN_POINT('Ctrl Pts',(-6.76689579452237,0.195372590733599,
127.688195149009));
#40537=CARTESIAN_POINT('Ctrl Pts',(-6.76699901925401,0.00364326986908226,
127.69717978381));
#40538=CARTESIAN_POINT('',(-6.76699990560448,-0.00113028709160019,127.302820216231));
#40539=CARTESIAN_POINT('Ctrl Pts',(3.09917575053261,6.01559628526638,126.651394038606));
#40540=CARTESIAN_POINT('Ctrl Pts',(2.94381645487386,6.0956358588835,126.659591593228));
#40541=CARTESIAN_POINT('Ctrl Pts',(2.78536392356738,6.16964823799883,126.667789147851));
#40542=CARTESIAN_POINT('Ctrl Pts',(2.62432973771906,6.23740189724243,126.675986702473));
#40543=CARTESIAN_POINT('Ctrl Pts',(2.46325647582193,6.30517199737578,126.684186246288));
#40544=CARTESIAN_POINT('Ctrl Pts',(2.29960064213102,6.36668021339887,126.692385790104));
#40545=CARTESIAN_POINT('Ctrl Pts',(2.13389282594102,6.42174356443773,126.700585333919));
#40546=CARTESIAN_POINT('Ctrl Pts',(1.96065235544694,6.47930995484877,126.709157608064));
#40547=CARTESIAN_POINT('Ctrl Pts',(1.78516939970454,6.52983170258234,126.717729882209));
#40548=CARTESIAN_POINT('Ctrl Pts',(1.60806593701526,6.57315852100124,126.726302156354));
#40549=CARTESIAN_POINT('Ctrl Pts',(1.43840199385435,6.61466532581434,126.734514338156));
#40550=CARTESIAN_POINT('Ctrl Pts',(1.26725127013855,6.64956931183984,126.742726519958));
#40551=CARTESIAN_POINT('Ctrl Pts',(1.09516889223115,6.67779110915348,126.75093870176));
#40552=CARTESIAN_POINT('Ctrl Pts',(0.92297235080651,6.70603162947457,126.759156331717));
#40553=CARTESIAN_POINT('Ctrl Pts',(0.749843277962059,6.72758108136217,126.767373961674));
#40554=CARTESIAN_POINT('Ctrl Pts',(0.576340570410812,6.74241207187002,126.775591591632));
#40555=CARTESIAN_POINT('Ctrl Pts',(0.402618889735319,6.75726178017411,126.78381959284));
#40556=CARTESIAN_POINT('Ctrl Pts',(0.228522989437664,6.76537608254519,126.792047594048));
#40557=CARTESIAN_POINT('Ctrl Pts',(0.0546111582759515,6.76677963446363,
126.800275595256));
#40558=CARTESIAN_POINT('Ctrl Pts',(0.032227316660986,6.76696028280498,126.801334604725));
#40559=CARTESIAN_POINT('Ctrl Pts',(0.00984651627423833,6.76702983287537,
126.802393614193));
#40560=CARTESIAN_POINT('Ctrl Pts',(-0.0125300605691292,6.76698839939763,
126.803452623661));
#40561=CARTESIAN_POINT('Ctrl Pts',(-0.184791316048411,6.76666943269672,
126.811605179874));
#40562=CARTESIAN_POINT('Ctrl Pts',(-0.35730982263907,6.75976801858847,126.819757736088));
#40563=CARTESIAN_POINT('Ctrl Pts',(-0.529537051957871,6.7462492920588,126.827910292301));
#40564=CARTESIAN_POINT('Ctrl Pts',(-0.701564751879324,6.73274622729973,
126.836053403581));
#40565=CARTESIAN_POINT('Ctrl Pts',(-0.873301485542799,6.71264113896775,
126.844196514862));
#40566=CARTESIAN_POINT('Ctrl Pts',(-1.04419673789595,6.68595110456003,126.852339626142));
#40567=CARTESIAN_POINT('Ctrl Pts',(-1.21492993257824,6.6592863799532,126.860475015419));
#40568=CARTESIAN_POINT('Ctrl Pts',(-1.38482287589788,6.62604919712483,126.868610404697));
#40569=CARTESIAN_POINT('Ctrl Pts',(-1.55332819486716,6.58630856542804,126.876745793974));
#40570=CARTESIAN_POINT('Ctrl Pts',(-1.72170912953962,6.54659726877278,126.884875178013));
#40571=CARTESIAN_POINT('Ctrl Pts',(-1.88870412510679,6.50039216564878,126.893004562051));
#40572=CARTESIAN_POINT('Ctrl Pts',(-2.05377405370416,6.4478136710308,126.90113394609));
#40573=CARTESIAN_POINT('Ctrl Pts',(-2.21875680646001,6.39526294388417,126.909259036882));
#40574=CARTESIAN_POINT('Ctrl Pts',(-2.3818161694176,6.336345639237,126.917384127674));
#40575=CARTESIAN_POINT('Ctrl Pts',(-2.54242628502315,6.27123254115357,126.925509218466));
#40576=CARTESIAN_POINT('Ctrl Pts',(-2.70364948425946,6.20587089225854,126.933665324491));
#40577=CARTESIAN_POINT('Ctrl Pts',(-2.86240434015847,6.13426614824959,126.941821430516));
#40578=CARTESIAN_POINT('Ctrl Pts',(-3.01817687839044,6.05664076289401,126.949977536541));
#40579=CARTESIAN_POINT('Ctrl Pts',(-3.17332246032779,5.97932780567579,126.958100815715));
#40580=CARTESIAN_POINT('Ctrl Pts',(-3.32550936654906,5.89604276468142,126.966224094888));
#40581=CARTESIAN_POINT('Ctrl Pts',(-3.47425259993951,5.80705242544043,126.974347374062));
#40582=CARTESIAN_POINT('Ctrl Pts',(-3.62301563974854,5.71805023638369,126.982471734918));
#40583=CARTESIAN_POINT('Ctrl Pts',(-3.76833377940971,5.62334142371958,126.990596095775));
#40584=CARTESIAN_POINT('Ctrl Pts',(-3.9097493944689,5.52323715518808,126.998720456632));
#40585=CARTESIAN_POINT('Ctrl Pts',(-4.05121074525977,5.42310051157576,127.006847445017));
#40586=CARTESIAN_POINT('Ctrl Pts',(-4.18876675971709,5.31756514857308,127.014974433403));
#40587=CARTESIAN_POINT('Ctrl Pts',(-4.32199143758641,5.20698367708502,127.023101421788));
#40588=CARTESIAN_POINT('Ctrl Pts',(-4.45607739783106,5.09568730897304,127.031280950228));
#40589=CARTESIAN_POINT('Ctrl Pts',(-4.58577553494708,4.97927960117355,127.039460478668));
#40590=CARTESIAN_POINT('Ctrl Pts',(-4.71068850989165,4.85815837152051,127.047640007108));
#40591=CARTESIAN_POINT('Ctrl Pts',(-4.83501322936692,4.73760754078578,127.055781015512));
#40592=CARTESIAN_POINT('Ctrl Pts',(-4.95459755359684,4.61238779628413,127.063922023916));
#40593=CARTESIAN_POINT('Ctrl Pts',(-5.06908987945627,4.48292502658633,127.072063032319));
#40594=CARTESIAN_POINT('Ctrl Pts',(-5.18439480401483,4.35254340684812,127.080261820778));
#40595=CARTESIAN_POINT('Ctrl Pts',(-5.2945349455551,4.21785860381408,127.088460609236));
#40596=CARTESIAN_POINT('Ctrl Pts',(-5.39919544763404,4.07933542605261,127.096659397694));
#40597=CARTESIAN_POINT('Ctrl Pts',(-5.50385594971299,3.94081224829114,127.104858186152));
#40598=CARTESIAN_POINT('Ctrl Pts',(-5.60303665319985,3.79845103754411,127.113056974611));
#40599=CARTESIAN_POINT('Ctrl Pts',(-5.69646982105714,3.65274151532589,127.121255763069));
#40600=CARTESIAN_POINT('Ctrl Pts',(-5.79352559600295,3.50138251808548,127.129772436384));
#40601=CARTESIAN_POINT('Ctrl Pts',(-5.88466267022944,3.34596973003752,127.138289109699));
#40602=CARTESIAN_POINT('Ctrl Pts',(-5.96953903341556,3.18698803394805,127.146805783014));
#40603=CARTESIAN_POINT('Ctrl Pts',(-6.05429517479537,3.02823152501265,127.15531039302));
#40604=CARTESIAN_POINT('Ctrl Pts',(-6.1328081275134,2.86591646572114,127.163815003025));
#40605=CARTESIAN_POINT('Ctrl Pts',(-6.20477906986329,2.70055655267325,127.172319613031));
#40606=CARTESIAN_POINT('Ctrl Pts',(-6.27665674318821,2.53541093385795,127.18081320169));
#40607=CARTESIAN_POINT('Ctrl Pts',(-6.34200917572603,2.36722862078917,127.189306790349));
#40608=CARTESIAN_POINT('Ctrl Pts',(-6.40058318452126,2.19654817794276,127.197800379008));
#40609=CARTESIAN_POINT('Ctrl Pts',(-6.46093687318422,2.02068187614292,127.206552032106));
#40610=CARTESIAN_POINT('Ctrl Pts',(-6.51409354487708,1.84216352814561,127.215303685205));
#40611=CARTESIAN_POINT('Ctrl Pts',(-6.55982847582034,1.66160746502193,127.224055338303));
#40612=CARTESIAN_POINT('Ctrl Pts',(-6.60410049396021,1.48682680750238,127.232527054271));
#40613=CARTESIAN_POINT('Ctrl Pts',(-6.64141811180504,1.31013712320766,127.240998770238));
#40614=CARTESIAN_POINT('Ctrl Pts',(-6.67162700840373,1.13211397868671,127.249470486205));
#40615=CARTESIAN_POINT('Ctrl Pts',(-6.70333322713052,0.945267009941253,
127.258362107869));
#40616=CARTESIAN_POINT('Ctrl Pts',(-6.72720797912353,0.756951360983467,
127.267253729533));
#40617=CARTESIAN_POINT('Ctrl Pts',(-6.74313260258851,0.567848310649833,
127.276145351197));
#40618=CARTESIAN_POINT('Ctrl Pts',(-6.75905722605351,0.37874526031607,127.285036972862));
#40619=CARTESIAN_POINT('Ctrl Pts',(-6.76703163872077,0.188855216149285,
127.293928594526));
#40620=CARTESIAN_POINT('Ctrl Pts',(-6.76699990560463,-0.00113028621264427,
127.30282021619));
#40621=CARTESIAN_POINT('Ctrl Pts',(-6.76699990560448,-0.00113028709141402,
127.302820216231));
#40622=CARTESIAN_POINT('Ctrl Pts',(-6.76696867316269,-0.188118117230485,
127.311571542099));
#40623=CARTESIAN_POINT('Ctrl Pts',(-6.75918283403797,-0.374911890116693,
127.320322867967));
#40624=CARTESIAN_POINT('Ctrl Pts',(-6.74371597829373,-0.560877708690457,
127.329074193836));
#40625=CARTESIAN_POINT('Ctrl Pts',(-6.72751731262625,-0.755642447592097,
127.338239586222));
#40626=CARTESIAN_POINT('Ctrl Pts',(-6.70289324644896,-0.949498613544085,
127.347404978609));
#40627=CARTESIAN_POINT('Ctrl Pts',(-6.66998776417228,-1.14173211647567,
127.356570370996));
#40628=CARTESIAN_POINT('Ctrl Pts',(-6.63842328888005,-1.32613146982976,
127.365362243399));
#40629=CARTESIAN_POINT('Ctrl Pts',(-6.59923911678114,-1.50903756531875,
127.374154115802));
#40630=CARTESIAN_POINT('Ctrl Pts',(-6.55261329048496,-1.68983669783796,
127.382945988205));
#40631=CARTESIAN_POINT('Ctrl Pts',(-6.50591798061802,-1.87090526406621,
127.391750962589));
#40632=CARTESIAN_POINT('Ctrl Pts',(-6.45175894277092,-2.04986033104845,
127.400555936973));
#40633=CARTESIAN_POINT('Ctrl Pts',(-6.39036327152211,-2.22610562597134,
127.409360911357));
#40634=CARTESIAN_POINT('Ctrl Pts',(-6.32883926742469,-2.40271931919156,
127.418184290417));
#40635=CARTESIAN_POINT('Ctrl Pts',(-6.26004848239057,-2.57661165666901,
127.427007669477));
#40636=CARTESIAN_POINT('Ctrl Pts',(-6.18426591542891,-2.74720659712084,
127.435831048537));
#40637=CARTESIAN_POINT('Ctrl Pts',(-6.17502474468359,-2.76800949462363,
127.43690699985));
#40638=CARTESIAN_POINT('Ctrl Pts',(-6.1656796601793,-2.78876339116494,127.437982951164));
#40639=CARTESIAN_POINT('Ctrl Pts',(-6.15623120611983,-2.80946726921607,
127.439058902477));
#40640=CARTESIAN_POINT('Ctrl Pts',(-6.08030675100585,-2.97583635455899,
127.447704868968));
#40641=CARTESIAN_POINT('Ctrl Pts',(-5.99756667944973,-3.13927409780236,
127.456350835459));
#40642=CARTESIAN_POINT('Ctrl Pts',(-5.90825281290134,-3.29921774044143,
127.464996801949));
#40643=CARTESIAN_POINT('Ctrl Pts',(-5.81905319093026,-3.45895679341762,
127.473631709074));
#40644=CARTESIAN_POINT('Ctrl Pts',(-5.72329668953091,-3.6152103931188,127.482266616198));
#40645=CARTESIAN_POINT('Ctrl Pts',(-5.62127221236195,-3.76743781826952,
127.490901523322));
#40646=CARTESIAN_POINT('Ctrl Pts',(-5.5158606048961,-3.92471907107075,127.499823102394));
#40647=CARTESIAN_POINT('Ctrl Pts',(-5.40375779265452,-4.07770191994871,
127.508744681466));
#40648=CARTESIAN_POINT('Ctrl Pts',(-5.28533431097518,-4.22581710693074,
127.517666260537));
#40649=CARTESIAN_POINT('Ctrl Pts',(-5.17103261878915,-4.36877706951941,
127.526277319513));
#40650=CARTESIAN_POINT('Ctrl Pts',(-5.05084301385447,-4.50720220746502,
127.534888378489));
#40651=CARTESIAN_POINT('Ctrl Pts',(-4.92514314577255,-4.64060922656172,
127.543499437464));
#40652=CARTESIAN_POINT('Ctrl Pts',(-4.79956181846957,-4.77389043668023,
127.552102375814));
#40653=CARTESIAN_POINT('Ctrl Pts',(-4.66848079678642,-4.90216274172892,
127.560705314163));
#40654=CARTESIAN_POINT('Ctrl Pts',(-4.53231775020979,-5.02497610055344,
127.569308252513));
#40655=CARTESIAN_POINT('Ctrl Pts',(-4.39630717474531,-5.14765193682778,
127.577901557562));
#40656=CARTESIAN_POINT('Ctrl Pts',(-4.2552261531301,-5.26488081784157,127.58649486261));
#40657=CARTESIAN_POINT('Ctrl Pts',(-4.10952908426155,-5.37624959480198,
127.595088167659));
#40658=CARTESIAN_POINT('Ctrl Pts',(-4.09329604597001,-5.3886578994777,127.5960456025));
#40659=CARTESIAN_POINT('Ctrl Pts',(-4.0770057429822,-5.40099349734913,127.59700303734));
#40660=CARTESIAN_POINT('Ctrl Pts',(-4.06065883134004,-5.41325584611149,
127.597960472181));
#40661=CARTESIAN_POINT('Ctrl Pts',(-3.91389783709851,-5.52334602922951,
127.606556229728));
#40662=CARTESIAN_POINT('Ctrl Pts',(-3.76274333118558,-5.62739979781851,
127.615151987276));
#40663=CARTESIAN_POINT('Ctrl Pts',(-3.60771671144361,-5.72509118966419,
127.623747744824));
#40664=CARTESIAN_POINT('Ctrl Pts',(-3.45254544659429,-5.82287373090011,
127.632351522505));
#40665=CARTESIAN_POINT('Ctrl Pts',(-3.29349511490486,-5.91428188352603,
127.640955300187));
#40666=CARTESIAN_POINT('Ctrl Pts',(-3.13111243014787,-5.99903525158617,
127.649559077868));
#40667=CARTESIAN_POINT('Ctrl Pts',(-2.96234796388609,-6.08711950112276,
127.658500991536));
#40668=CARTESIAN_POINT('Ctrl Pts',(-2.78998425885458,-6.16801514780056,
127.667442905204));
#40669=CARTESIAN_POINT('Ctrl Pts',(-2.61465742661348,-6.24146261235738,
127.676384818872));
#40670=CARTESIAN_POINT('Ctrl Pts',(-2.44550123567848,-6.31232508776661,
127.685012021203));
#40671=CARTESIAN_POINT('Ctrl Pts',(-2.27358723276122,-6.37625466673425,
127.693639223534));
#40672=CARTESIAN_POINT('Ctrl Pts',(-2.0995022295599,-6.43306920435907,127.702266425864));
#40673=CARTESIAN_POINT('Ctrl Pts',(-1.92525143703901,-6.48993784913477,
127.710901844285));
#40674=CARTESIAN_POINT('Ctrl Pts',(-1.74882580973115,-6.53967784143297,
127.719537262705));
#40675=CARTESIAN_POINT('Ctrl Pts',(-1.57082454858861,-6.58215764301885,
127.728172681126));
#40676=CARTESIAN_POINT('Ctrl Pts',(-1.39256031593683,-6.62470020246084,
127.736820857147));
#40677=CARTESIAN_POINT('Ctrl Pts',(-1.21271609613202,-6.65996107432725,
127.745469033168));
#40678=CARTESIAN_POINT('Ctrl Pts',(-1.03189991720437,-6.68786001355244,
127.754117209189));
#40679=CARTESIAN_POINT('Ctrl Pts',(-1.01277025107528,-6.69081161553794,
127.755032153421));
#40680=CARTESIAN_POINT('Ctrl Pts',(-0.993629709127076,-6.69368086457255,
127.755947097652));
#40681=CARTESIAN_POINT('Ctrl Pts',(-0.97447901319423,-6.69646769967899,
127.756862041884));
#40682=CARTESIAN_POINT('Ctrl Pts',(-0.802300779324919,-6.72152330854014,
127.765088034425));
#40683=CARTESIAN_POINT('Ctrl Pts',(-0.628929604938511,-6.73996702089787,
127.773314026967));
#40684=CARTESIAN_POINT('Ctrl Pts',(-0.454914030333935,-6.75169180465203,
127.781540019508));
#40685=CARTESIAN_POINT('Ctrl Pts',(-0.28108088856713,-6.76340429648589,
127.789757388159));
#40686=CARTESIAN_POINT('Ctrl Pts',(-0.106605046435611,-6.76841186289632,
127.797974756811));
#40687=CARTESIAN_POINT('Ctrl Pts',(0.0679564280944051,-6.7666587710539,
127.806192125462));
#40688=CARTESIAN_POINT('Ctrl Pts',(0.242369826476127,-6.7649071663156,127.814402523525));
#40689=CARTESIAN_POINT('Ctrl Pts',(0.416868356325892,-6.7564063287222,127.822612921587));
#40690=CARTESIAN_POINT('Ctrl Pts',(0.590891413560338,-6.74115244875687,
127.830823319649));
#40691=CARTESIAN_POINT('Ctrl Pts',(0.764801662826502,-6.72590845690196,
127.839028395438));
#40692=CARTESIAN_POINT('Ctrl Pts',(0.938236697782867,-6.70392017363867,
127.847233471227));
#40693=CARTESIAN_POINT('Ctrl Pts',(1.11063740751498,-6.67523584220276,127.855438547016));
#40694=CARTESIAN_POINT('Ctrl Pts',(1.28296084085476,-6.64656436814809,127.863639944985));
#40695=CARTESIAN_POINT('Ctrl Pts',(1.45425051995198,-6.61120288430478,127.871841342955));
#40696=CARTESIAN_POINT('Ctrl Pts',(1.62395384490536,-6.56925132032693,127.880042740924));
#40697=CARTESIAN_POINT('Ctrl Pts',(1.79364387728128,-6.52730304234488,127.888243496492));
#40698=CARTESIAN_POINT('Ctrl Pts',(1.96174745338401,-6.47876578986581,127.89644425206));
#40699=CARTESIAN_POINT('Ctrl Pts',(2.12772316693707,-6.4237904016927,127.904645007627));
#40700=CARTESIAN_POINT('Ctrl Pts',(2.29369803741249,-6.3688152927684,127.912845721539));
#40701=CARTESIAN_POINT('Ctrl Pts',(2.45754472633466,-6.30740222495959,127.921046435451));
#40702=CARTESIAN_POINT('Ctrl Pts',(2.61873808867114,-6.23975158343207,127.929247149363));
#40703=CARTESIAN_POINT('Ctrl Pts',(2.77995984447301,-6.17208902555688,127.937449307792));
#40704=CARTESIAN_POINT('Ctrl Pts',(2.93852701207702,-6.09818684363949,127.945651466222));
#40705=CARTESIAN_POINT('Ctrl Pts',(3.09393543899492,-6.01829315498434,127.953853624651));
#40706=CARTESIAN_POINT('Ctrl Pts',(3.24939940456278,-5.93837091454666,127.962058714304));
#40707=CARTESIAN_POINT('Ctrl Pts',(3.40170206219766,-5.85245306572805,127.970263803957));
#40708=CARTESIAN_POINT('Ctrl Pts',(3.55036477854347,-5.76083318099717,127.97846889361));
#40709=CARTESIAN_POINT('Ctrl Pts',(3.6991973244663,-5.66910863138022,127.986683356608));
#40710=CARTESIAN_POINT('Ctrl Pts',(3.8443813163463,-5.57166922043436,127.994897819606));
#40711=CARTESIAN_POINT('Ctrl Pts',(3.98546711301411,-5.46885188052145,128.003112282604));
#40712=CARTESIAN_POINT('Ctrl Pts',(4.12663649855741,-5.3659736245842,128.011331612411));
#40713=CARTESIAN_POINT('Ctrl Pts',(4.26370256809365,-5.2577113100097,128.019550942219));
#40714=CARTESIAN_POINT('Ctrl Pts',(4.39624969900895,-5.14444142584632,128.027770272026));
#40715=CARTESIAN_POINT('Ctrl Pts',(4.5290022036674,-5.03099603686487,128.036002337187));
#40716=CARTESIAN_POINT('Ctrl Pts',(4.65722151430005,-4.91252781596581,128.044234402348));
#40717=CARTESIAN_POINT('Ctrl Pts',(4.78052878804062,-4.78945023011148,128.052466467508));
#40718=CARTESIAN_POINT('Ctrl Pts',(4.89136621962794,-4.67881925848881,128.059866038769));
#40719=CARTESIAN_POINT('Ctrl Pts',(4.99823527393971,-4.56446466434207,128.067265610031));
#40720=CARTESIAN_POINT('Ctrl Pts',(5.10088968969296,-4.44670815025948,128.074665181292));
#40721=CARTESIAN_POINT('Ctrl Pts',(5.21403054453363,-4.31692247500527,128.082820639699));
#40722=CARTESIAN_POINT('Ctrl Pts',(5.32239936044838,-4.18260420149505,128.090976098106));
#40723=CARTESIAN_POINT('Ctrl Pts',(5.42560704560762,-4.04414109381127,128.099131556512));
#40724=CARTESIAN_POINT('Ctrl Pts',(5.52868911344757,-3.90584651393023,128.107277088654));
#40725=CARTESIAN_POINT('Ctrl Pts',(5.6266223386572,-3.76341743162741,128.115422620796));
#40726=CARTESIAN_POINT('Ctrl Pts',(5.7190551960092,-3.61727752114767,128.123568152938));
#40727=CARTESIAN_POINT('Ctrl Pts',(5.81139498719925,-3.47128475185737,128.131705483739));
#40728=CARTESIAN_POINT('Ctrl Pts',(5.89824524189807,-3.3215888991978,128.139842814539));
#40729=CARTESIAN_POINT('Ctrl Pts',(5.97929539458907,-3.16864570191209,128.14798014534));
#40730=CARTESIAN_POINT('Ctrl Pts',(6.06028097475199,-3.01582435422904,128.156110993142));
#40731=CARTESIAN_POINT('Ctrl Pts',(6.13547548340759,-2.85976113471935,128.164241840944));
#40732=CARTESIAN_POINT('Ctrl Pts',(6.20461230495252,-2.70093967819198,128.172372688746));
#40733=CARTESIAN_POINT('Ctrl Pts',(6.27370856868759,-2.54221139127081,128.18049876674));
#40734=CARTESIAN_POINT('Ctrl Pts',(6.3367540767727,-2.3807284239678,128.188624844733));
#40735=CARTESIAN_POINT('Ctrl Pts',(6.39352872013706,-2.21699785854262,128.196750922727));
#40736=CARTESIAN_POINT('Ctrl Pts',(6.45050467601728,-2.05268673443676,128.204905814309));
#40737=CARTESIAN_POINT('Ctrl Pts',(6.50116504619806,-1.88611237523665,128.213060705892));
#40738=CARTESIAN_POINT('Ctrl Pts',(6.54533639651662,-1.71780687402132,128.221215597474));
#40739=CARTESIAN_POINT('Ctrl Pts',(6.58933549401299,-1.55015770541441,128.22933868783));
#40740=CARTESIAN_POINT('Ctrl Pts',(6.62689601368207,-1.38079123286572,128.237461778186));
#40741=CARTESIAN_POINT('Ctrl Pts',(6.65789680929449,-1.210247527073,128.245584868543));
#40742=CARTESIAN_POINT('Ctrl Pts',(6.68890003923093,-1.03969042940975,128.253708596761));
#40743=CARTESIAN_POINT('Ctrl Pts',(6.71334245362125,-0.867956274295264,
128.26183232498));
#40744=CARTESIAN_POINT('Ctrl Pts',(6.7311542771293,-0.69559406084577,128.269956053198));
#40745=CARTESIAN_POINT('Ctrl Pts',(6.74897088798132,-0.523185521021988,
128.278081964858));
#40746=CARTESIAN_POINT('Ctrl Pts',(6.76015332181594,-0.350148950475839,
128.286207876519));
#40747=CARTESIAN_POINT('Ctrl Pts',(6.76468379518772,-0.177037146171877,
128.294333788179));
#40748=CARTESIAN_POINT('Ctrl Pts',(6.76924324140766,-0.00281827388451997,
128.302511665889));
#40749=CARTESIAN_POINT('Ctrl Pts',(6.76706534206994,0.171476422285105,128.310689543599));
#40750=CARTESIAN_POINT('Ctrl Pts',(6.75818517174349,0.34528565627094,128.318867421309));
#40751=CARTESIAN_POINT('Ctrl Pts',(6.74934738454401,0.518265336480143,128.327006267783));
#40752=CARTESIAN_POINT('Ctrl Pts',(6.73387125710201,0.690763819472348,128.335145114256));
#40753=CARTESIAN_POINT('Ctrl Pts',(6.71184318948325,0.86223546655618,128.34328396073));
#40754=CARTESIAN_POINT('Ctrl Pts',(6.68965666279002,1.03494059625703,128.351481354058));
#40755=CARTESIAN_POINT('Ctrl Pts',(6.66082364023708,1.20660368870575,128.359678747386));
#40756=CARTESIAN_POINT('Ctrl Pts',(6.6254841039516,1.37668056871761,128.367876140715));
#40757=CARTESIAN_POINT('Ctrl Pts',(6.59014456766612,1.54675744872948,128.376073534043));
#40758=CARTESIAN_POINT('Ctrl Pts',(6.54829866667873,1.71524776977647,128.384270927372));
#40759=CARTESIAN_POINT('Ctrl Pts',(6.50013633950522,1.88162604357074,128.3924683207));
#40760=CARTESIAN_POINT('Ctrl Pts',(6.45179842136804,2.04861090187087,128.400695600213));
#40761=CARTESIAN_POINT('Ctrl Pts',(6.39695416720556,2.21396535831026,128.408922879726));
#40762=CARTESIAN_POINT('Ctrl Pts',(6.3357294915854,2.37714551709715,128.417150159238));
#40763=CARTESIAN_POINT('Ctrl Pts',(6.27457521065064,2.54013805519308,128.42536797922));
#40764=CARTESIAN_POINT('Ctrl Pts',(6.20705524254268,2.70096094122537,128.433585799201));
#40765=CARTESIAN_POINT('Ctrl Pts',(6.13334583212878,2.85908340268496,128.441803619182));
#40766=CARTESIAN_POINT('Ctrl Pts',(6.05970637539851,3.01705579852086,128.450013640067));
#40767=CARTESIAN_POINT('Ctrl Pts',(5.97988932671191,3.17233255114162,128.458223660952));
#40768=CARTESIAN_POINT('Ctrl Pts',(5.89411979160669,3.32440083055434,128.466433681837));
#40769=CARTESIAN_POINT('Ctrl Pts',(5.8084230412695,3.47634006351216,128.474636735628));
#40770=CARTESIAN_POINT('Ctrl Pts',(5.71678404734098,3.62507593853215,128.482839789418));
#40771=CARTESIAN_POINT('Ctrl Pts',(5.61947475416967,3.77011836515111,128.491042843209));
#40772=CARTESIAN_POINT('Ctrl Pts',(5.52221150991263,3.91509215447913,128.499242015132));
#40773=CARTESIAN_POINT('Ctrl Pts',(5.41928350913567,4.0563756788621,128.507441187056));
#40774=CARTESIAN_POINT('Ctrl Pts',(5.31100728740936,4.19350576404572,128.51564035898));
#40775=CARTESIAN_POINT('Ctrl Pts',(5.2027626251986,4.33059587961286,128.523837141072));
#40776=CARTESIAN_POINT('Ctrl Pts',(5.08917306910854,4.46353468625805,128.532033923165));
#40777=CARTESIAN_POINT('Ctrl Pts',(4.97059693649293,4.5918901440395,128.540230705257));
#40778=CARTESIAN_POINT('Ctrl Pts',(4.85203381518062,4.72023151743691,128.54842658792));
#40779=CARTESIAN_POINT('Ctrl Pts',(4.72848545144471,4.84399028133397,128.556622470584));
#40780=CARTESIAN_POINT('Ctrl Pts',(4.60034872764433,4.96276944699844,128.564818353247));
#40781=CARTESIAN_POINT('Ctrl Pts',(4.47216607729763,5.08159118528918,128.573017173465));
#40782=CARTESIAN_POINT('Ctrl Pts',(4.33939204282602,5.19542951388512,128.581215993682));
#40783=CARTESIAN_POINT('Ctrl Pts',(4.20245885588674,5.303925769143,128.5894148139));
#40784=CARTESIAN_POINT('Ctrl Pts',(4.06549886044986,5.41244326557449,128.597615239266));
#40785=CARTESIAN_POINT('Ctrl Pts',(3.92437837564445,5.51561638776814,128.605815664632));
#40786=CARTESIAN_POINT('Ctrl Pts',(3.77956062976668,5.61312840098262,128.614016089998));
#40787=CARTESIAN_POINT('Ctrl Pts',(3.63463457808358,5.71071334115129,128.62222264827));
#40788=CARTESIAN_POINT('Ctrl Pts',(3.48600604426765,5.80262852217369,128.630429206542));
#40789=CARTESIAN_POINT('Ctrl Pts',(3.33416555725262,5.88860161981012,128.638635764814));
#40790=CARTESIAN_POINT('Ctrl Pts',(3.25664982541948,5.9324915447719,128.64282527568));
#40791=CARTESIAN_POINT('Ctrl Pts',(3.17829739323455,5.97483359695155,128.647014786547));
#40792=CARTESIAN_POINT('Ctrl Pts',(3.09917575053256,6.01559628526641,128.651204297413));
#40793=CARTESIAN_POINT('Origin',(0.,0.,-3.69717978381041));
#40794=CARTESIAN_POINT('',(3.09917575053245,6.01559628526646,131.045629062141));
#40795=CARTESIAN_POINT('',(3.09917575053269,6.01559628526634,130.651392015122));
#40796=CARTESIAN_POINT('',(3.09917575053259,6.01559628526639,-3.69717978381041));
#40797=CARTESIAN_POINT('',(-6.767,7.73790753694215E-12,129.69717978381));
#40798=CARTESIAN_POINT('Ctrl Pts',(-6.76699924398711,-0.0031987306766745,
129.69717978381));
#40799=CARTESIAN_POINT('Ctrl Pts',(-6.76690738963476,-0.19751903948158,
129.70629472893));
#40800=CARTESIAN_POINT('Ctrl Pts',(-6.75844129896495,-0.391590285911398,
129.71540967405));
#40801=CARTESIAN_POINT('Ctrl Pts',(-6.74168986956949,-0.584727887606004,
129.72452461917));
#40802=CARTESIAN_POINT('Ctrl Pts',(-6.72486379031202,-0.778726173781559,
129.733680183475));
#40803=CARTESIAN_POINT('Ctrl Pts',(-6.6996784308952,-0.971782271623306,
129.742835747779));
#40804=CARTESIAN_POINT('Ctrl Pts',(-6.66627455968819,-1.16321644368282,
129.751991312083));
#40805=CARTESIAN_POINT('Ctrl Pts',(-6.63279655757565,-1.35507545238578,
129.761167194699));
#40806=CARTESIAN_POINT('Ctrl Pts',(-6.5910636168629,-1.54530513563145,129.770343077315));
#40807=CARTESIAN_POINT('Ctrl Pts',(-6.5412670110954,-1.73323826681593,129.779518959932));
#40808=CARTESIAN_POINT('Ctrl Pts',(-6.49133564545543,-1.92167998376446,
129.788719674376));
#40809=CARTESIAN_POINT('Ctrl Pts',(-6.43329700355376,-2.10781251261126,
129.797920388821));
#40810=CARTESIAN_POINT('Ctrl Pts',(-6.36739232471245,-2.2909831913816,129.807121103265));
#40811=CARTESIAN_POINT('Ctrl Pts',(-6.34999085318926,-2.33934757774299,
129.809550459924));
#40812=CARTESIAN_POINT('Ctrl Pts',(-6.33204124098797,-2.38750558883375,
129.811979816583));
#40813=CARTESIAN_POINT('Ctrl Pts',(-6.31354847724027,-2.43544546757612,
129.814409173242));
#40814=CARTESIAN_POINT('Ctrl Pts',(-6.25094052106384,-2.59774775339746,
129.822633852761));
#40815=CARTESIAN_POINT('Ctrl Pts',(-6.18198758564383,-2.75784818275406,
129.83085853228));
#40816=CARTESIAN_POINT('Ctrl Pts',(-6.10686520993706,-2.91521633976974,
129.839083211799));
#40817=CARTESIAN_POINT('Ctrl Pts',(-6.03182179634599,-3.0724190850488,129.847299246249));
#40818=CARTESIAN_POINT('Ctrl Pts',(-5.95062200909514,-3.22689495622112,
129.855515280699));
#40819=CARTESIAN_POINT('Ctrl Pts',(-5.86349028128006,-3.37813124690772,
129.863731315149));
#40820=CARTESIAN_POINT('Ctrl Pts',(-5.77643268612984,-3.5292388640384,129.871940359304));
#40821=CARTESIAN_POINT('Ctrl Pts',(-5.68345337995602,-3.67711208130814,
129.880149403458));
#40822=CARTESIAN_POINT('Ctrl Pts',(-5.58482378685168,-3.82126056031457,
129.888358447613));
#40823=CARTESIAN_POINT('Ctrl Pts',(-5.48625835882553,-3.96531526119484,
129.896562151241));
#40824=CARTESIAN_POINT('Ctrl Pts',(-5.38205016757828,-4.10564975584145,
129.904765854869));
#40825=CARTESIAN_POINT('Ctrl Pts',(-5.27251527509775,-4.24180052263905,
129.912969558497));
#40826=CARTESIAN_POINT('Ctrl Pts',(-5.16302971293989,-4.37788997234302,
129.921169567491));
#40827=CARTESIAN_POINT('Ctrl Pts',(-5.04822245310552,-4.50979916934204,
129.929369576485));
#40828=CARTESIAN_POINT('Ctrl Pts',(-4.92845141551991,-4.63709560445542,
129.937569585479));
#40829=CARTESIAN_POINT('Ctrl Pts',(-4.80868995507916,-4.76438186067728,
129.945768938783));
#40830=CARTESIAN_POINT('Ctrl Pts',(-4.68396574653091,-4.88705582287398,
129.953968292087));
#40831=CARTESIAN_POINT('Ctrl Pts',(-4.55467559393565,-5.0047196958478,129.962167645391));
#40832=CARTESIAN_POINT('Ctrl Pts',(-4.42538628427397,-5.12238280168796,
129.970366945237));
#40833=CARTESIAN_POINT('Ctrl Pts',(-4.29153135427883,-5.2350356412576,129.978566245084));
#40834=CARTESIAN_POINT('Ctrl Pts',(-4.15354281875892,-5.34231888347525,
129.98676554493));
#40835=CARTESIAN_POINT('Ctrl Pts',(-4.01553015040907,-5.44962088847076,
129.994966278753));
#40836=CARTESIAN_POINT('Ctrl Pts',(-3.87338271926515,-5.55155120507676,
130.003167012576));
#40837=CARTESIAN_POINT('Ctrl Pts',(-3.72756384859864,-5.64779220179182,
130.011367746399));
#40838=CARTESIAN_POINT('Ctrl Pts',(-3.58169302239312,-5.74406748935576,
130.019571402159));
#40839=CARTESIAN_POINT('Ctrl Pts',(-3.43214844981436,-5.83464922154886,
130.027775057919));
#40840=CARTESIAN_POINT('Ctrl Pts',(-3.27942055711838,-5.91926429630823,
130.035978713679));
#40841=CARTESIAN_POINT('Ctrl Pts',(-3.12651770480307,-6.00397630307529,
130.044191767254));
#40842=CARTESIAN_POINT('Ctrl Pts',(-2.97042456076769,-6.08270782284415,
130.052404820829));
#40843=CARTESIAN_POINT('Ctrl Pts',(-2.81165512958056,-6.15523228093818,
130.060617874404));
#40844=CARTESIAN_POINT('Ctrl Pts',(-2.65279175095887,-6.2277996533812,130.068835787827));
#40845=CARTESIAN_POINT('Ctrl Pts',(-2.49124925952316,-6.29415250678049,
130.07705370125));
#40846=CARTESIAN_POINT('Ctrl Pts',(-2.32755945122351,-6.35411331351748,
130.085271614674));
#40847=CARTESIAN_POINT('Ctrl Pts',(-2.1636143420384,-6.41416763888714,130.09350234527));
#40848=CARTESIAN_POINT('Ctrl Pts',(-1.99751556403329,-6.46780988428938,
130.101733075865));
#40849=CARTESIAN_POINT('Ctrl Pts',(-1.82980911846274,-6.51491270777979,
130.109963806461));
#40850=CARTESIAN_POINT('Ctrl Pts',(-1.67579080551377,-6.5581710177657,130.117522748137));
#40851=CARTESIAN_POINT('Ctrl Pts',(-1.52041688788452,-6.59591438128047,
130.125081689813));
#40852=CARTESIAN_POINT('Ctrl Pts',(-1.36411511610003,-6.6280825998193,130.132640631489));
#40853=CARTESIAN_POINT('Ctrl Pts',(-1.19551111738506,-6.66278272007554,
130.140794523656));
#40854=CARTESIAN_POINT('Ctrl Pts',(-1.02530602535819,-6.69110210282341,
130.148948415823));
#40855=CARTESIAN_POINT('Ctrl Pts',(-0.854028533119562,-6.71289239185447,
130.157102307989));
#40856=CARTESIAN_POINT('Ctrl Pts',(-0.682960047273748,-6.73465609064505,
130.165246250129));
#40857=CARTESIAN_POINT('Ctrl Pts',(-0.510822124793817,-6.74990650923921,
130.17339019227));
#40858=CARTESIAN_POINT('Ctrl Pts',(-0.338156286058496,-6.75854565170637,
130.18153413441));
#40859=CARTESIAN_POINT('Ctrl Pts',(-0.16566480517129,-6.76717607037327,
130.189669852803));
#40860=CARTESIAN_POINT('Ctrl Pts',(0.00735316824682647,-6.76920848550534,
130.197805571196));
#40861=CARTESIAN_POINT('Ctrl Pts',(0.180348304968705,-6.76459632859899,
130.205941289589));
#40862=CARTESIAN_POINT('Ctrl Pts',(0.353205140885511,-6.75998785887729,
130.214070503889));
#40863=CARTESIAN_POINT('Ctrl Pts',(0.526038812645128,-6.74874540355847,
130.222199718189));
#40864=CARTESIAN_POINT('Ctrl Pts',(0.698297283945808,-6.73087437880354,
130.230328932489));
#40865=CARTESIAN_POINT('Ctrl Pts',(0.870454262849295,-6.71301388341839,
130.238453357165));
#40866=CARTESIAN_POINT('Ctrl Pts',(1.04203635341537,-6.68853263380989,130.24657778184));
#40867=CARTESIAN_POINT('Ctrl Pts',(1.21249394515143,-6.65748807231159,130.254702206516));
#40868=CARTESIAN_POINT('Ctrl Pts',(1.3839863235906,-6.62625505045131,130.26287595165));
#40869=CARTESIAN_POINT('Ctrl Pts',(1.55434013045905,-6.58837877894014,130.271049696784));
#40870=CARTESIAN_POINT('Ctrl Pts',(1.72300276572845,-6.54397054312534,130.279223441918));
#40871=CARTESIAN_POINT('Ctrl Pts',(1.89058533483587,-6.4998466846579,130.28734484478));
#40872=CARTESIAN_POINT('Ctrl Pts',(2.05649797640161,-6.44927439147436,130.295466247642));
#40873=CARTESIAN_POINT('Ctrl Pts',(2.22021101105309,-6.39241363386309,130.303587650505));
#40874=CARTESIAN_POINT('Ctrl Pts',(2.38393670313444,-6.3355484800774,130.311709681271));
#40875=CARTESIAN_POINT('Ctrl Pts',(2.54546210380607,-6.27239401345154,130.319831712037));
#40876=CARTESIAN_POINT('Ctrl Pts',(2.70427501342557,-6.20315932825864,130.327953742803));
#40877=CARTESIAN_POINT('Ctrl Pts',(2.86313044326826,-6.13390610632162,130.336077948144));
#40878=CARTESIAN_POINT('Ctrl Pts',(3.0192716006406,-6.05856957056588,130.344202153486));
#40879=CARTESIAN_POINT('Ctrl Pts',(3.17220854073453,-5.97740595694244,130.352326358827));
#40880=CARTESIAN_POINT('Ctrl Pts',(3.32680091738079,-5.89536380336239,130.360538503069));
#40881=CARTESIAN_POINT('Ctrl Pts',(3.47811896533468,-5.80736786586981,130.368750647312));
#40882=CARTESIAN_POINT('Ctrl Pts',(3.62568515748499,-5.71372874214317,130.376962791554));
#40883=CARTESIAN_POINT('Ctrl Pts',(3.77190423294008,-5.62094444041242,130.38509996797));
#40884=CARTESIAN_POINT('Ctrl Pts',(3.91443940300342,-5.52261981534696,130.393237144387));
#40885=CARTESIAN_POINT('Ctrl Pts',(4.05285832728311,-5.41909848397055,130.401374320803));
#40886=CARTESIAN_POINT('Ctrl Pts',(4.19319013238832,-5.31414653918017,130.409623948959));
#40887=CARTESIAN_POINT('Ctrl Pts',(4.32929078473411,-5.20385345154031,130.417873577114));
#40888=CARTESIAN_POINT('Ctrl Pts',(4.46074768411949,-5.08861661933994,130.42612320527));
#40889=CARTESIAN_POINT('Ctrl Pts',(4.59220458350477,-4.97337978713966,130.434372833425));
#40890=CARTESIAN_POINT('Ctrl Pts',(4.71901749416093,-4.85319952097227,130.44262246158));
#40891=CARTESIAN_POINT('Ctrl Pts',(4.84081577943282,-4.72850838950237,130.450872089736));
#40892=CARTESIAN_POINT('Ctrl Pts',(4.96224849868354,-4.60419150665758,130.459096957413));
#40893=CARTESIAN_POINT('Ctrl Pts',(5.07905975120422,-4.47501932224297,130.467321825091));
#40894=CARTESIAN_POINT('Ctrl Pts',(5.19083848069689,-4.34136900842539,130.475546692768));
#40895=CARTESIAN_POINT('Ctrl Pts',(5.30249127893944,-4.20786926664575,130.483762294212));
#40896=CARTESIAN_POINT('Ctrl Pts',(5.40912261590147,-4.06990171426767,130.491977895656));
#40897=CARTESIAN_POINT('Ctrl Pts',(5.51035759188929,-3.92788088025949,130.500193497099));
#40898=CARTESIAN_POINT('Ctrl Pts',(5.6114988554834,-3.78599151378199,130.508401493427));
#40899=CARTESIAN_POINT('Ctrl Pts',(5.70725349954401,-3.64005662834271,130.516609489755));
#40900=CARTESIAN_POINT('Ctrl Pts',(5.79728625832106,-3.49052446475911,130.524817486083));
#40901=CARTESIAN_POINT('Ctrl Pts',(5.88725375805353,-3.34110068757021,130.533019532955));
#40902=CARTESIAN_POINT('Ctrl Pts',(5.97150744909434,-3.18808513187573,130.541221579826));
#40903=CARTESIAN_POINT('Ctrl Pts',(6.04975480083046,-3.03195577966251,130.549423626698));
#40904=CARTESIAN_POINT('Ctrl Pts',(6.12796114878569,-2.87590824355686,130.557621375469));
#40905=CARTESIAN_POINT('Ctrl Pts',(6.20016726736905,-2.7167504815555,130.565819124241));
#40906=CARTESIAN_POINT('Ctrl Pts',(6.26612605579254,-2.55498595943653,130.574016873012));
#40907=CARTESIAN_POINT('Ctrl Pts',(6.33207226390178,-2.39325229065147,130.582213058228));
#40908=CARTESIAN_POINT('Ctrl Pts',(6.39177337419266,-2.22891318161422,130.590409243444));
#40909=CARTESIAN_POINT('Ctrl Pts',(6.44502990148471,-2.06249328943587,130.598605428659));
#40910=CARTESIAN_POINT('Ctrl Pts',(6.4982824889791,-1.89608570862543,130.60680100754));
#40911=CARTESIAN_POINT('Ctrl Pts',(6.54509133272955,-1.72759799271165,130.61499658642));
#40912=CARTESIAN_POINT('Ctrl Pts',(6.58530645209658,-1.55757116433732,130.6231921653));
#40913=CARTESIAN_POINT('Ctrl Pts',(6.6255259131046,-1.38752597979602,130.631388628979));
#40914=CARTESIAN_POINT('Ctrl Pts',(6.65915014887506,-1.21594170101305,130.639585092657));
#40915=CARTESIAN_POINT('Ctrl Pts',(6.68608004114364,-1.0433708273767,130.647781556336));
#40916=CARTESIAN_POINT('Ctrl Pts',(6.71301774037002,-0.870749925559182,
130.655980396163));
#40917=CARTESIAN_POINT('Ctrl Pts',(6.73325717518532,-0.697142213637369,
130.664179235991));
#40918=CARTESIAN_POINT('Ctrl Pts',(6.7467509524248,-0.523106667855641,130.672378075819));
#40919=CARTESIAN_POINT('Ctrl Pts',(6.76025882429848,-0.348889336995441,
130.680585479568));
#40920=CARTESIAN_POINT('Ctrl Pts',(6.76700693376946,-0.174243637693806,
130.688792883317));
#40921=CARTESIAN_POINT('Ctrl Pts',(6.76699999465041,0.000269075059461636,
130.697000287067));
#40922=CARTESIAN_POINT('Ctrl Pts',(6.7669930518144,0.174875266056849,130.705212087136));
#40923=CARTESIAN_POINT('Ctrl Pts',(6.76022386098969,0.349347970276594,130.713423887205));
#40924=CARTESIAN_POINT('Ctrl Pts',(6.74674916702813,0.523129694440314,130.721635687274));
#40925=CARTESIAN_POINT('Ctrl Pts',(6.73325463643426,0.69716724958432,130.72985957626));
#40926=CARTESIAN_POINT('Ctrl Pts',(6.7130349164852,0.870511435369368,130.738083465246));
#40927=CARTESIAN_POINT('Ctrl Pts',(6.68619834803656,1.04261241634332,130.746307354232));
#40928=CARTESIAN_POINT('Ctrl Pts',(6.66140182273576,1.20163074751253,130.753906085482));
#40929=CARTESIAN_POINT('Ctrl Pts',(6.63095681354871,1.35958760053109,130.761504816732));
#40930=CARTESIAN_POINT('Ctrl Pts',(6.59498663675077,1.51606077090555,130.769103547982));
#40931=CARTESIAN_POINT('Ctrl Pts',(6.55604909223164,1.68544223021088,130.777329138254));
#40932=CARTESIAN_POINT('Ctrl Pts',(6.51052727055085,1.85356040123578,130.785554728526));
#40933=CARTESIAN_POINT('Ctrl Pts',(6.45851629097573,2.01986542106178,130.793780318797));
#40934=CARTESIAN_POINT('Ctrl Pts',(6.40656485515067,2.18598004984698,130.801996492163));
#40935=CARTESIAN_POINT('Ctrl Pts',(6.34813916151968,2.35028532159709,130.810212665529));
#40936=CARTESIAN_POINT('Ctrl Pts',(6.28338531284172,2.51224163056919,130.818428838895));
#40937=CARTESIAN_POINT('Ctrl Pts',(6.21869258501756,2.67404506974153,130.826637257054));
#40938=CARTESIAN_POINT('Ctrl Pts',(6.14768373105114,2.83350363088453,130.834845675212));
#40939=CARTESIAN_POINT('Ctrl Pts',(6.07055464352359,2.99009286143327,130.84305409337));
#40940=CARTESIAN_POINT('Ctrl Pts',(5.99124367379952,3.15111179892206,130.851494717069));
#40941=CARTESIAN_POINT('Ctrl Pts',(5.90546119169844,3.3090963010754,130.859935340768));
#40942=CARTESIAN_POINT('Ctrl Pts',(5.81347385054582,3.46349690183491,130.868375964467));
#40943=CARTESIAN_POINT('Ctrl Pts',(5.72413345520992,3.61345460839659,130.876573708294));
#40944=CARTESIAN_POINT('Ctrl Pts',(5.62894054988741,3.76003148253646,130.884771452121));
#40945=CARTESIAN_POINT('Ctrl Pts',(5.52818643102089,3.90274823475413,130.892969195949));
#40946=CARTESIAN_POINT('Ctrl Pts',(5.42746020013165,4.04542548405532,130.901164670703));
#40947=CARTESIAN_POINT('Ctrl Pts',(5.32117602798296,4.18424444651526,130.909360145457));
#40948=CARTESIAN_POINT('Ctrl Pts',(5.20966860603309,4.31875468339118,130.917555620211));
#40949=CARTESIAN_POINT('Ctrl Pts',(5.09817176159913,4.45325216072028,130.925750317548));
#40950=CARTESIAN_POINT('Ctrl Pts',(4.98145288366333,4.58344145087146,130.933945014885));
#40951=CARTESIAN_POINT('Ctrl Pts',(4.85988705663106,4.70890505285358,130.942139712222));
#40952=CARTESIAN_POINT('Ctrl Pts',(4.73195098717559,4.84094314685721,130.950763824715));
#40953=CARTESIAN_POINT('Ctrl Pts',(4.59864662326234,4.9677466415458,130.959387937208));
#40954=CARTESIAN_POINT('Ctrl Pts',(4.46045520800506,5.08887299285221,130.968012049701));
#40955=CARTESIAN_POINT('Ctrl Pts',(4.32905181572083,5.20404956461711,130.976212542004));
#40956=CARTESIAN_POINT('Ctrl Pts',(4.19323028367595,5.31409314157282,130.984413034306));
#40957=CARTESIAN_POINT('Ctrl Pts',(4.05343801734618,5.41866489455961,130.992613526608));
#40958=CARTESIAN_POINT('Ctrl Pts',(3.91359325594592,5.52327591653951,131.000817098376));
#40959=CARTESIAN_POINT('Ctrl Pts',(3.76977508164834,5.62241081314886,131.009020670143));
#40960=CARTESIAN_POINT('Ctrl Pts',(3.6224597627499,5.71577416167381,131.017224241911));
#40961=CARTESIAN_POINT('Ctrl Pts',(3.47501555347743,5.80921919645517,131.025434991217));
#40962=CARTESIAN_POINT('Ctrl Pts',(3.32406839923682,5.89688241953781,131.033645740524));
#40963=CARTESIAN_POINT('Ctrl Pts',(3.17011952322347,5.97851413049074,131.04185648983));
#40964=CARTESIAN_POINT('Ctrl Pts',(3.14654135573895,5.99101650272455,131.043114013934));
#40965=CARTESIAN_POINT('Ctrl Pts',(3.12289281746731,6.00337748679119,131.044371538037));
#40966=CARTESIAN_POINT('Ctrl Pts',(3.09917575053245,6.01559628526646,131.045629062141));
#40967=CARTESIAN_POINT('Ctrl Pts',(3.09917575053253,6.01559628526642,129.045751582742));
#40968=CARTESIAN_POINT('Ctrl Pts',(2.93382384459265,6.10078395293759,129.054501030655));
#40969=CARTESIAN_POINT('Ctrl Pts',(2.76495772122989,6.17915010267047,129.063250478567));
#40970=CARTESIAN_POINT('Ctrl Pts',(2.59315093316722,6.25042856433173,129.07199992648));
#40971=CARTESIAN_POINT('Ctrl Pts',(2.42134553245632,6.32170645041445,129.08074930374));
#40972=CARTESIAN_POINT('Ctrl Pts',(2.2465997792761,6.3858966531345,129.089498681));
#40973=CARTESIAN_POINT('Ctrl Pts',(2.06950718689943,6.44278115439067,129.09824805826));
#40974=CARTESIAN_POINT('Ctrl Pts',(1.8924159657289,6.49966521519715,129.106997367774));
#40975=CARTESIAN_POINT('Ctrl Pts',(1.71297821457231,6.54924360009537,129.115746677289));
#40976=CARTESIAN_POINT('Ctrl Pts',(1.53180337335883,6.59134792173547,129.124495986804));
#40977=CARTESIAN_POINT('Ctrl Pts',(1.35062987477833,6.63345193135294,129.13324523148));
#40978=CARTESIAN_POINT('Ctrl Pts',(1.16771959103014,6.66808192368227,129.141994476156));
#40979=CARTESIAN_POINT('Ctrl Pts',(0.983693746907582,6.69512028363157,129.150743720832));
#40980=CARTESIAN_POINT('Ctrl Pts',(0.79966920542072,6.72215845218857,129.159492903576));
#40981=CARTESIAN_POINT('Ctrl Pts',(0.614529402874435,6.7416050542457,129.16824208632));
#40982=CARTESIAN_POINT('Ctrl Pts',(0.428903127364318,6.75339404354115,129.176991269065));
#40983=CARTESIAN_POINT('Ctrl Pts',(0.243278104164956,6.76518295330326,129.185740392783));
#40984=CARTESIAN_POINT('Ctrl Pts',(0.0571669005402013,6.76931433552275,
129.194489516502));
#40985=CARTESIAN_POINT('Ctrl Pts',(-0.128798404776425,6.76577415902475,
129.20323864022));
#40986=CARTESIAN_POINT('Ctrl Pts',(-0.314762517257864,6.76223400523447,
129.21198770782));
#40987=CARTESIAN_POINT('Ctrl Pts',(-0.500580446818132,6.75102239665099,
129.220736775419));
#40988=CARTESIAN_POINT('Ctrl Pts',(-0.685621118841091,6.73217741012513,
129.229485843018));
#40989=CARTESIAN_POINT('Ctrl Pts',(-0.870660665412942,6.71333253821792,
129.238234857404));
#40990=CARTESIAN_POINT('Ctrl Pts',(-1.0549226788533,6.68685441030637,129.24698387179));
#40991=CARTESIAN_POINT('Ctrl Pts',(-1.23778137635093,6.65283295028207,129.255732886175));
#40992=CARTESIAN_POINT('Ctrl Pts',(-1.42999922978675,6.61707018861902,129.264929696543));
#40993=CARTESIAN_POINT('Ctrl Pts',(-1.62066601233511,6.57297172934458,129.27412650691));
#40994=CARTESIAN_POINT('Ctrl Pts',(-1.8090662850019,6.52070304311349,129.283323317277));
#40995=CARTESIAN_POINT('Ctrl Pts',(-1.98831342545335,6.4709737491509,129.292073315015));
#40996=CARTESIAN_POINT('Ctrl Pts',(-2.16550875896513,6.41384933989592,129.300823312753));
#40997=CARTESIAN_POINT('Ctrl Pts',(-2.34005036713826,6.34952386240544,129.309573310491));
#40998=CARTESIAN_POINT('Ctrl Pts',(-2.51458843546905,6.28519968948669,129.318323130772));
#40999=CARTESIAN_POINT('Ctrl Pts',(-2.68647261717874,6.21367483971177,129.327072951052));
#41000=CARTESIAN_POINT('Ctrl Pts',(-2.85511905908553,6.13519226743927,129.335822771333));
#41001=CARTESIAN_POINT('Ctrl Pts',(-3.02376230488714,6.05671118253022,129.344572425792));
#41002=CARTESIAN_POINT('Ctrl Pts',(-3.18916767379743,5.97127275992719,129.35332208025));
#41003=CARTESIAN_POINT('Ctrl Pts',(-3.35077334102635,5.87916720438083,129.362071734709));
#41004=CARTESIAN_POINT('Ctrl Pts',(-3.51237616037228,5.78706327195729,129.370821234977));
#41005=CARTESIAN_POINT('Ctrl Pts',(-3.67017916302171,5.68829258362382,129.379570735246));
#41006=CARTESIAN_POINT('Ctrl Pts',(-3.82364636566344,5.58319061741123,129.388320235514));
#41007=CARTESIAN_POINT('Ctrl Pts',(-3.977111067787,5.47809036367774,129.397069593223));
#41008=CARTESIAN_POINT('Ctrl Pts',(-4.12623987481848,5.36665920043287,129.405818950931));
#41009=CARTESIAN_POINT('Ctrl Pts',(-4.27052628213868,5.24927559512385,129.41456830864));
#41010=CARTESIAN_POINT('Ctrl Pts',(-4.41481053024925,5.13189374643082,129.423317535416));
#41011=CARTESIAN_POINT('Ctrl Pts',(-4.55425230136485,5.00855981477394,129.432066762193));
#41012=CARTESIAN_POINT('Ctrl Pts',(-4.6883780063051,4.87969268192113,129.440815988969));
#41013=CARTESIAN_POINT('Ctrl Pts',(-4.82250188228874,4.75082730631831,129.44956509644));
#41014=CARTESIAN_POINT('Ctrl Pts',(-4.95130963052961,4.61642907903532,129.458314203911));
#41015=CARTESIAN_POINT('Ctrl Pts',(-5.07436379033377,4.47695444731678,129.467063311382));
#41016=CARTESIAN_POINT('Ctrl Pts',(-5.19741643562798,4.33748153220595,129.475812311171));
#41017=CARTESIAN_POINT('Ctrl Pts',(-5.31471544462749,4.19293255254619,129.484561310961));
#41018=CARTESIAN_POINT('Ctrl Pts',(-5.42586245275589,4.04379841779655,129.493310310751));
#41019=CARTESIAN_POINT('Ctrl Pts',(-5.5370216001911,3.89464799484404,129.502060266093));
#41020=CARTESIAN_POINT('Ctrl Pts',(-5.64202723081205,3.7409116444392,129.510810221435));
#41021=CARTESIAN_POINT('Ctrl Pts',(-5.74052265232917,3.58311159163312,129.519560176777));
#41022=CARTESIAN_POINT('Ctrl Pts',(-5.83901427066877,3.42531763191853,129.52830979426));
#41023=CARTESIAN_POINT('Ctrl Pts',(-5.93099603115707,3.26346052695673,129.537059411742));
#41024=CARTESIAN_POINT('Ctrl Pts',(-6.01615550622728,3.09809004467126,129.545809029225));
#41025=CARTESIAN_POINT('Ctrl Pts',(-6.10131214578772,2.93272506863885,129.554558355376));
#41026=CARTESIAN_POINT('Ctrl Pts',(-6.17964682328718,2.76384720416959,129.563307681527));
#41027=CARTESIAN_POINT('Ctrl Pts',(-6.25089348288533,2.59203002791667,129.572057007678));
#41028=CARTESIAN_POINT('Ctrl Pts',(-6.32213814889297,2.42021765937114,129.58080608901));
#41029=CARTESIAN_POINT('Ctrl Pts',(-6.38629508412551,2.24546640832015,129.589555170341));
#41030=CARTESIAN_POINT('Ctrl Pts',(-6.44314639819777,2.06836976660151,129.598304251673));
#41031=CARTESIAN_POINT('Ctrl Pts',(-6.50000285283667,1.89125711158388,129.607054124107));
#41032=CARTESIAN_POINT('Ctrl Pts',(-6.54955227673219,1.71179891440371,129.615803996542));
#41033=CARTESIAN_POINT('Ctrl Pts',(-6.59162635926357,1.5306047627855,129.624553868976));
#41034=CARTESIAN_POINT('Ctrl Pts',(-6.63369752055173,1.34942319164813,129.633303133898));
#41035=CARTESIAN_POINT('Ctrl Pts',(-6.66829431424234,1.16650618642819,129.642052398821));
#41036=CARTESIAN_POINT('Ctrl Pts',(-6.69529923745401,0.982474997619684,
129.650801663743));
#41037=CARTESIAN_POINT('Ctrl Pts',(-6.7223055473143,0.798434359178886,129.659551377923));
#41038=CARTESIAN_POINT('Ctrl Pts',(-6.74171916496692,0.6132797062415,129.668301092103));
#41039=CARTESIAN_POINT('Ctrl Pts',(-6.75347414817267,0.427639953656556,
129.677050806283));
#41040=CARTESIAN_POINT('Ctrl Pts',(-6.76248837758729,0.285283364201413,
129.683760465458));
#41041=CARTESIAN_POINT('Ctrl Pts',(-6.76699999999984,0.142641701109623,
129.690470124634));
#41042=CARTESIAN_POINT('Ctrl Pts',(-6.767,7.7379071769556E-12,129.69717978381));
#41043=CARTESIAN_POINT('',(-6.76699999999221,-7.25967800658328E-6,129.302661224348));
#41044=CARTESIAN_POINT('Ctrl Pts',(3.09917575053256,6.01559628526641,128.651204297413));
#41045=CARTESIAN_POINT('Ctrl Pts',(2.9440104223218,6.09553592877141,128.659420340539));
#41046=CARTESIAN_POINT('Ctrl Pts',(2.78588580690729,6.16939841906691,128.667636383664));
#41047=CARTESIAN_POINT('Ctrl Pts',(2.62532466559796,6.2369831970435,128.67585242679));
#41048=CARTESIAN_POINT('Ctrl Pts',(2.46455027994386,6.30465773566566,128.684079381801));
#41049=CARTESIAN_POINT('Ctrl Pts',(2.30133324025139,6.36603778476158,128.692306336812));
#41050=CARTESIAN_POINT('Ctrl Pts',(2.13621222485776,6.42097238199701,128.700533291823));
#41051=CARTESIAN_POINT('Ctrl Pts',(2.07106150047759,6.44264756849515,128.703779347918));
#41052=CARTESIAN_POINT('Ctrl Pts',(2.00561448731159,6.46331988343004,128.707025404012));
#41053=CARTESIAN_POINT('Ctrl Pts',(1.93990468080482,6.48298224811634,128.710271460107));
#41054=CARTESIAN_POINT('Ctrl Pts',(1.77338196479372,6.53281088930136,128.718497661126));
#41055=CARTESIAN_POINT('Ctrl Pts',(1.60470540771669,6.57628906836901,128.726723862145));
#41056=CARTESIAN_POINT('Ctrl Pts',(1.4344001855779,6.61322803989202,128.734950063164));
#41057=CARTESIAN_POINT('Ctrl Pts',(1.26428626546245,6.65012551826583,128.743167023779));
#41058=CARTESIAN_POINT('Ctrl Pts',(1.09254767054565,6.6804983404962,128.751383984395));
#41059=CARTESIAN_POINT('Ctrl Pts',(0.919725847131263,6.70420713926104,128.759600945011));
#41060=CARTESIAN_POINT('Ctrl Pts',(0.747063465898483,6.72789406473162,128.767810324813));
#41061=CARTESIAN_POINT('Ctrl Pts',(0.573320199519717,6.74492916247715,128.776019704614));
#41062=CARTESIAN_POINT('Ctrl Pts',(0.399048922805098,6.7552238273212,128.784229084416));
#41063=CARTESIAN_POINT('Ctrl Pts',(0.224903459104328,6.76551106005805,128.792432537556));
#41064=CARTESIAN_POINT('Ctrl Pts',(0.0502311008960856,6.76906753141212,
128.800635990696));
#41065=CARTESIAN_POINT('Ctrl Pts',(-0.124408803756455,6.76585629832233,
128.808839443837));
#41066=CARTESIAN_POINT('Ctrl Pts',(-0.298957661599014,6.76264673937757,
128.817038620187));
#41067=CARTESIAN_POINT('Ctrl Pts',(-0.473473741869148,6.75267651152258,
128.825237796537));
#41068=CARTESIAN_POINT('Ctrl Pts',(-0.647396243356407,6.73596074098477,
128.833436972887));
#41069=CARTESIAN_POINT('Ctrl Pts',(-0.821286018700192,6.71924811577145,
128.841634606439));
#41070=CARTESIAN_POINT('Ctrl Pts',(-0.994582080518735,6.69579250422001,
128.84983223999));
#41071=CARTESIAN_POINT('Ctrl Pts',(-1.1667269888724,6.66566104249509,128.858029873541));
#41072=CARTESIAN_POINT('Ctrl Pts',(-1.33885949856776,6.63553175097493,128.866226916662));
#41073=CARTESIAN_POINT('Ctrl Pts',(-1.50984066646091,6.59872762784131,128.874423959783));
#41074=CARTESIAN_POINT('Ctrl Pts',(-1.67912156354888,6.55536724942434,128.882621002903));
#41075=CARTESIAN_POINT('Ctrl Pts',(-1.84842103477821,6.51200211334236,128.890818945434));
#41076=CARTESIAN_POINT('Ctrl Pts',(-2.01601951598553,6.46207937778859,128.899016887966));
#41077=CARTESIAN_POINT('Ctrl Pts',(-2.18138154705541,6.40576799034793,128.907214830497));
#41078=CARTESIAN_POINT('Ctrl Pts',(-2.34679177665886,6.34944018966972,128.915415162505));
#41079=CARTESIAN_POINT('Ctrl Pts',(-2.50996391824188,6.28672014358343,128.923615494514));
#41080=CARTESIAN_POINT('Ctrl Pts',(-2.6703808069506,6.21782561237205,128.931815826522));
#41081=CARTESIAN_POINT('Ctrl Pts',(-2.83096489341449,6.14885927443848,128.940024705493));
#41082=CARTESIAN_POINT('Ctrl Pts',(-2.98878765973918,6.07370573598786,128.948233584464));
#41083=CARTESIAN_POINT('Ctrl Pts',(-3.14335404596476,5.99263000207063,128.956442463434));
#41084=CARTESIAN_POINT('Ctrl Pts',(-3.29800340701176,5.91151074481881,128.964655749122));
#41085=CARTESIAN_POINT('Ctrl Pts',(-3.44939259242023,5.82446313292807,128.972869034809));
#41086=CARTESIAN_POINT('Ctrl Pts',(-3.59705413084859,5.73179645309785,128.981082320497));
#41087=CARTESIAN_POINT('Ctrl Pts',(-3.74493167990867,5.63899421333603,128.989307621209));
#41088=CARTESIAN_POINT('Ctrl Pts',(-3.88907038817019,5.54055668076361,128.997532921921));
#41089=CARTESIAN_POINT('Ctrl Pts',(-4.02903354369501,5.43683526546284,129.005758222633));
#41090=CARTESIAN_POINT('Ctrl Pts',(-4.15561333441668,5.34303175701167,129.013197014927));
#41091=CARTESIAN_POINT('Ctrl Pts',(-4.2787782140976,5.24490719771872,129.020635807221));
#41092=CARTESIAN_POINT('Ctrl Pts',(-4.39823092866461,5.14274767980484,129.028074599515));
#41093=CARTESIAN_POINT('Ctrl Pts',(-4.52725775511892,5.03240009635888,129.036109609567));
#41094=CARTESIAN_POINT('Ctrl Pts',(-4.65235748891922,4.9169981106864,129.04414461962));
#41095=CARTESIAN_POINT('Ctrl Pts',(-4.77309623590166,4.7968574424118,129.052179629672));
#41096=CARTESIAN_POINT('Ctrl Pts',(-4.89369434429776,4.67685671607107,129.060205280406));
#41097=CARTESIAN_POINT('Ctrl Pts',(-5.00994130901634,4.55212855192056,129.068230931139));
#41098=CARTESIAN_POINT('Ctrl Pts',(-5.12143488514761,4.42302992497147,129.076256581873));
#41099=CARTESIAN_POINT('Ctrl Pts',(-5.23282341484566,4.29405293149011,129.084274671041));
#41100=CARTESIAN_POINT('Ctrl Pts',(-5.3394672239266,4.16071395224508,129.092292760209));
#41101=CARTESIAN_POINT('Ctrl Pts',(-5.44099976391248,4.02340783032299,129.100310849377));
#41102=CARTESIAN_POINT('Ctrl Pts',(-5.54768044892983,3.87913968588614,129.108735490827));
#41103=CARTESIAN_POINT('Ctrl Pts',(-5.64871771618113,3.73049188693583,129.117160132278));
#41104=CARTESIAN_POINT('Ctrl Pts',(-5.74373245937411,3.57796400696434,129.125584773729));
#41105=CARTESIAN_POINT('Ctrl Pts',(-5.83405496340395,3.43296861371881,129.13359336993));
#41106=CARTESIAN_POINT('Ctrl Pts',(-5.91893522435928,3.28446750234395,129.141601966131));
#41107=CARTESIAN_POINT('Ctrl Pts',(-5.99809093790158,3.13292101730365,129.149610562332));
#41108=CARTESIAN_POINT('Ctrl Pts',(-6.07723035421531,2.98140573389866,129.157617509658));
#41109=CARTESIAN_POINT('Ctrl Pts',(-6.15064739374005,2.8268466578194,129.165624456983));
#41110=CARTESIAN_POINT('Ctrl Pts',(-6.21810531290707,2.66972944651643,129.173631404309));
#41111=CARTESIAN_POINT('Ctrl Pts',(-6.28556289144914,2.51261302856794,129.181638311204));
#41112=CARTESIAN_POINT('Ctrl Pts',(-6.34706126145097,2.35293884734312,129.189645218099));
#41113=CARTESIAN_POINT('Ctrl Pts',(-6.40241158852347,2.19121310034885,129.197652124993));
#41114=CARTESIAN_POINT('Ctrl Pts',(-6.45777275425353,2.02945568434587,129.205660599795));
#41115=CARTESIAN_POINT('Ctrl Pts',(-6.50698336058093,1.86564625967157,129.213669074596));
#41116=CARTESIAN_POINT('Ctrl Pts',(-6.54990431716319,1.70030657118269,129.221677549397));
#41117=CARTESIAN_POINT('Ctrl Pts',(-6.59286143806111,1.53482757087132,129.229692771974));
#41118=CARTESIAN_POINT('Ctrl Pts',(-6.62951823469096,1.36781609729384,129.237707994551));
#41119=CARTESIAN_POINT('Ctrl Pts',(-6.65978655532315,1.19980499979664,129.245723217129));
#41120=CARTESIAN_POINT('Ctrl Pts',(-6.69006970683263,1.0317115801911,129.253742367006));
#41121=CARTESIAN_POINT('Ctrl Pts',(-6.71395809635258,0.86261793319884,129.261761516884));
#41122=CARTESIAN_POINT('Ctrl Pts',(-6.73141547101049,0.69306187071619,129.269780666762));
#41123=CARTESIAN_POINT('Ctrl Pts',(-6.74889317667775,0.523308341778371,
129.27780915581));
#41124=CARTESIAN_POINT('Ctrl Pts',(-6.75992489399972,0.353091696664028,
129.285837644859));
#41125=CARTESIAN_POINT('Ctrl Pts',(-6.76452646095415,0.182950154553431,
129.293866133908));
#41126=CARTESIAN_POINT('Ctrl Pts',(-6.76617640361321,0.12194402529639,129.296744837337));
#41127=CARTESIAN_POINT('Ctrl Pts',(-6.76700013301525,0.0609475105471824,
129.299623540766));
#41128=CARTESIAN_POINT('Ctrl Pts',(-6.76699999998389,-1.47668897061706E-5,
129.302502244194));
#41129=CARTESIAN_POINT('Ctrl Pts',(-6.767,7.17729152692933E-12,129.30282021619));
#41130=CARTESIAN_POINT('Ctrl Pts',(-6.7670000000002,-0.186007249408519,
129.311569727996));
#41131=CARTESIAN_POINT('Ctrl Pts',(-6.75932637295478,-0.372014355520398,
129.320319239802));
#41132=CARTESIAN_POINT('Ctrl Pts',(-6.74400518266987,-0.557389537147947,
129.329068751608));
#41133=CARTESIAN_POINT('Ctrl Pts',(-6.72868405709722,-0.742763935804469,
129.337818226458));
#41134=CARTESIAN_POINT('Ctrl Pts',(-6.70571545653085,-0.927506129688286,
129.346567701309));
#41135=CARTESIAN_POINT('Ctrl Pts',(-6.67517739415759,-1.11098863924319,
129.35531717616));
#41136=CARTESIAN_POINT('Ctrl Pts',(-6.64463945823193,-1.29447038906025,
129.364066614782));
#41137=CARTESIAN_POINT('Ctrl Pts',(-6.60653217027261,-1.47669218227756,
129.372816053404));
#41138=CARTESIAN_POINT('Ctrl Pts',(-6.56098496116824,-1.65703510503676,
129.381565492025));
#41139=CARTESIAN_POINT('Ctrl Pts',(-6.51543793687637,-1.83737729603595,
129.390314895146));
#41140=CARTESIAN_POINT('Ctrl Pts',(-6.46245112202766,-2.01584035396648,
129.399064298266));
#41141=CARTESIAN_POINT('Ctrl Pts',(-6.40220448416374,-2.19181813637757,
129.407813701386));
#41142=CARTESIAN_POINT('Ctrl Pts',(-6.34195808575326,-2.36779521935571,
129.416563069731));
#41143=CARTESIAN_POINT('Ctrl Pts',(-6.2744520148938,-2.54128677544468,129.425312438077));
#41144=CARTESIAN_POINT('Ctrl Pts',(-6.19991555136335,-2.71170355237495,
129.434061806422));
#41145=CARTESIAN_POINT('Ctrl Pts',(-6.12537937789198,-2.88211966612733,
129.442811140719));
#41146=CARTESIAN_POINT('Ctrl Pts',(-6.04381298133785,-3.04946076210112,
129.451560475016));
#41147=CARTESIAN_POINT('Ctrl Pts',(-5.95549339426482,-3.21315848206528,
129.460309809313));
#41148=CARTESIAN_POINT('Ctrl Pts',(-5.86717414355344,-3.37685557859318,
129.469059110289));
#41149=CARTESIAN_POINT('Ctrl Pts',(-5.77210188986428,-3.53690907467001,
129.477808411264));
#41150=CARTESIAN_POINT('Ctrl Pts',(-5.67059953467265,-3.69277536784603,
129.48655771224));
#41151=CARTESIAN_POINT('Ctrl Pts',(-5.56909755761984,-3.84864108035476,
129.495306980621));
#41152=CARTESIAN_POINT('Ctrl Pts',(-5.46116568338311,-4.00031938103949,
129.504056249001));
#41153=CARTESIAN_POINT('Ctrl Pts',(-5.3471704868638,-4.14729511662876,129.512805517382));
#41154=CARTESIAN_POINT('Ctrl Pts',(-5.23317570555785,-4.29427031687715,
129.521554753895));
#41155=CARTESIAN_POINT('Ctrl Pts',(-5.11311782179073,-4.43654275986821,
129.530303990407));
#41156=CARTESIAN_POINT('Ctrl Pts',(-4.98740459172281,-4.57362924147358,
129.53905322692));
#41157=CARTESIAN_POINT('Ctrl Pts',(-4.86169180911101,-4.71071523514156,
129.547802432291));
#41158=CARTESIAN_POINT('Ctrl Pts',(-4.73032391415706,-4.84261509316256,
129.556551637662));
#41159=CARTESIAN_POINT('Ctrl Pts',(-4.59374707237571,-4.96888084331267,
129.565300843033));
#41160=CARTESIAN_POINT('Ctrl Pts',(-4.45717070537693,-5.09514615452469,
129.57405001799));
#41161=CARTESIAN_POINT('Ctrl Pts',(-4.31538563819814,-5.2157772025338,129.582799192946));
#41162=CARTESIAN_POINT('Ctrl Pts',(-4.16887341290967,-5.33036429028401,
129.591548367902));
#41163=CARTESIAN_POINT('Ctrl Pts',(-4.02236168477664,-5.44495098920936,
129.60029751317));
#41164=CARTESIAN_POINT('Ctrl Pts',(-3.87112305634771,-5.55349359238527,
129.609046658438));
#41165=CARTESIAN_POINT('Ctrl Pts',(-3.71567117317071,-5.65562346102251,
129.617795803706));
#41166=CARTESIAN_POINT('Ctrl Pts',(-3.56021980457659,-5.75775299158547,
129.626544920012));
#41167=CARTESIAN_POINT('Ctrl Pts',(-3.40055544862767,-5.85346967275132,
129.635294036318));
#41168=CARTESIAN_POINT('Ctrl Pts',(-3.23722036323803,-5.94244842803344,
129.644043152624));
#41169=CARTESIAN_POINT('Ctrl Pts',(-3.07388580496466,-6.03142689616261,
129.652792240695));
#41170=CARTESIAN_POINT('Ctrl Pts',(-2.90688079258145,-6.11366734484614,
129.661541328766));
#41171=CARTESIAN_POINT('Ctrl Pts',(-2.73677251095072,-6.188890467871,129.670290416837));
#41172=CARTESIAN_POINT('Ctrl Pts',(-2.56666476417092,-6.26411335438088,
129.679039477399));
#41173=CARTESIAN_POINT('Ctrl Pts',(-2.39345402972529,-6.33231884350126,
129.687788537962));
#41174=CARTESIAN_POINT('Ctrl Pts',(-2.21772856474462,-6.39327529620896,
129.696537598524));
#41175=CARTESIAN_POINT('Ctrl Pts',(-2.04200363768691,-6.45423156231948,
129.705286632304));
#41176=CARTESIAN_POINT('Ctrl Pts',(-1.86376426620512,-6.50793874251936,
129.714035666084));
#41177=CARTESIAN_POINT('Ctrl Pts',(-1.68361578195104,-6.55421443796016,
129.722784699864));
#41178=CARTESIAN_POINT('Ctrl Pts',(-1.50346783420284,-6.60048999558585,
129.731533707588));
#41179=CARTESIAN_POINT('Ctrl Pts',(-1.32141106257663,-6.63933404145413,
129.740282715312));
#41180=CARTESIAN_POINT('Ctrl Pts',(-1.1380637595946,-6.67061465526959,129.749031723037));
#41181=CARTESIAN_POINT('Ctrl Pts',(-0.954716987423112,-6.70189517852425,
129.757780705431));
#41182=CARTESIAN_POINT('Ctrl Pts',(-0.770079973813634,-6.72561226535785,
129.766529687826));
#41183=CARTESIAN_POINT('Ctrl Pts',(-0.584779770556007,-6.74168536939751,
129.775278670221));
#41184=CARTESIAN_POINT('Ctrl Pts',(-0.391490647557431,-6.75845143942374,
129.784404850897));
#41185=CARTESIAN_POINT('Ctrl Pts',(-0.197480213107819,-6.76689975924016,
129.793531031573));
#41186=CARTESIAN_POINT('Ctrl Pts',(-0.00346532630124065,-6.76699911271707,
129.802657212249));
#41187=CARTESIAN_POINT('Ctrl Pts',(0.1844865952926,-6.76709536139783,129.811498199779));
#41188=CARTESIAN_POINT('Ctrl Pts',(0.372442378181765,-6.75935659726789,
129.820339187309));
#41189=CARTESIAN_POINT('Ctrl Pts',(0.559750217718619,-6.74380965729045,
129.829180174839));
#41190=CARTESIAN_POINT('Ctrl Pts',(0.745129914454193,-6.72842275717292,
129.837930153437));
#41191=CARTESIAN_POINT('Ctrl Pts',(0.929874656310534,-6.70538772273523,
129.846680132035));
#41192=CARTESIAN_POINT('Ctrl Pts',(1.11335688289404,-6.67478280180805,129.855430110632));
#41193=CARTESIAN_POINT('Ctrl Pts',(1.29683723118487,-6.64417819418096,129.864179999657));
#41194=CARTESIAN_POINT('Ctrl Pts',(1.4790548072987,-6.60600390230157,129.872929888682));
#41195=CARTESIAN_POINT('Ctrl Pts',(1.65939064804448,-6.56038959797225,129.881679777707));
#41196=CARTESIAN_POINT('Ctrl Pts',(1.83972470263903,-6.51477574543358,129.890429580068));
#41197=CARTESIAN_POINT('Ctrl Pts',(2.01817678125484,-6.46172209820213,129.899179382429));
#41198=CARTESIAN_POINT('Ctrl Pts',(2.19414072347314,-6.40140886724139,129.90792918479));
#41199=CARTESIAN_POINT('Ctrl Pts',(2.37010298131733,-6.3410962136151,129.916678903396));
#41200=CARTESIAN_POINT('Ctrl Pts',(2.5435768792655,-6.27352420826118,129.925428622001));
#41201=CARTESIAN_POINT('Ctrl Pts',(2.71397317789611,-6.19892237325654,129.934178340607));
#41202=CARTESIAN_POINT('Ctrl Pts',(2.8843679020684,-6.12432122757133,129.942927978365));
#41203=CARTESIAN_POINT('Ctrl Pts',(3.05168482125896,-6.04269049717599,129.951677616123));
#41204=CARTESIAN_POINT('Ctrl Pts',(3.21535561997029,-5.95430745235124,129.960427253881));
#41205=CARTESIAN_POINT('Ctrl Pts',(3.37902496074928,-5.8659251948172,129.9691768137));
#41206=CARTESIAN_POINT('Ctrl Pts',(3.53904799384529,-5.77079087940444,129.977926373519));
#41207=CARTESIAN_POINT('Ctrl Pts',(3.69488118814646,-5.66922763747245,129.986675933338));
#41208=CARTESIAN_POINT('Ctrl Pts',(3.85071304610505,-5.56766526649279,129.995425418126));
#41209=CARTESIAN_POINT('Ctrl Pts',(4.0023548970565,-5.45967423580947,130.004174902913));
#41210=CARTESIAN_POINT('Ctrl Pts',(4.14929168607347,-5.34562133936567,130.012924387701));
#41211=CARTESIAN_POINT('Ctrl Pts',(4.29622726385449,-5.23156938308783,130.021673800364));
#41212=CARTESIAN_POINT('Ctrl Pts',(4.43845763091759,-5.11145583677469,130.030423213027));
#41213=CARTESIAN_POINT('Ctrl Pts',(4.57549970660654,-4.98568866204494,130.039172625691));
#41214=CARTESIAN_POINT('Ctrl Pts',(4.7125406981499,-4.85992248226457,130.047921969137));
#41215=CARTESIAN_POINT('Ctrl Pts',(4.84439326931013,-4.7285029573431,130.056671312583));
#41216=CARTESIAN_POINT('Ctrl Pts',(4.97060959434401,-4.59187644222003,130.06542065603));
#41217=CARTESIAN_POINT('Ctrl Pts',(5.09682496280234,-4.45525096256986,130.074169933166));
#41218=CARTESIAN_POINT('Ctrl Pts',(5.21740397615573,-4.31341878218648,130.082919210302));
#41219=CARTESIAN_POINT('Ctrl Pts',(5.33193710451683,-4.16686161438999,130.091668487438));
#41220=CARTESIAN_POINT('Ctrl Pts',(5.44646940289147,-4.02030550864834,130.100417701171));
#41221=CARTESIAN_POINT('Ctrl Pts',(5.55495572749443,-3.86902470980452,130.109166914904));
#41222=CARTESIAN_POINT('Ctrl Pts',(5.65702762491248,-3.71353301466098,130.117916128637));
#41223=CARTESIAN_POINT('Ctrl Pts',(5.75909881654965,-3.55804239467199,130.126665281873));
#41224=CARTESIAN_POINT('Ctrl Pts',(5.85475551250611,-3.39834117619848,130.13541443511));
#41225=CARTESIAN_POINT('Ctrl Pts',(5.94367283727941,-3.23497174692253,130.144163588346));
#41226=CARTESIAN_POINT('Ctrl Pts',(6.03258957676174,-3.07160339301236,130.152912683991));
#41227=CARTESIAN_POINT('Ctrl Pts',(6.11476689685163,-2.9045671282976,130.161661779637));
#41228=CARTESIAN_POINT('Ctrl Pts',(6.18992570525154,-2.73443024476146,130.170410875282));
#41229=CARTESIAN_POINT('Ctrl Pts',(6.26508404388601,-2.56429442463265,130.179159916243));
#41230=CARTESIAN_POINT('Ctrl Pts',(6.33322384283229,-2.39105828656222,130.187908957204));
#41231=CARTESIAN_POINT('Ctrl Pts',(6.39411368719956,-2.21531017132304,130.196657998165));
#41232=CARTESIAN_POINT('Ctrl Pts',(6.45500317120823,-2.03956309619728,130.205406987348));
#41233=CARTESIAN_POINT('Ctrl Pts',(6.50864269270015,-1.86130434438837,130.21415597653));
#41234=CARTESIAN_POINT('Ctrl Pts',(6.55485008446284,-1.68113930720138,130.222904965713));
#41235=CARTESIAN_POINT('Ctrl Pts',(6.60199664749362,-1.49731239212026,130.231831779242));
#41236=CARTESIAN_POINT('Ctrl Pts',(6.64140563640871,-1.31150116499851,130.240758592771));
#41237=CARTESIAN_POINT('Ctrl Pts',(6.67293772282143,-1.12436255155832,130.249685406301));
#41238=CARTESIAN_POINT('Ctrl Pts',(6.70384494949846,-0.940932395053107,
130.258435320456));
#41239=CARTESIAN_POINT('Ctrl Pts',(6.7271844934891,-0.756227260508516,130.267185234612));
#41240=CARTESIAN_POINT('Ctrl Pts',(6.74287707373917,-0.57087456454353,130.275935148767));
#41241=CARTESIAN_POINT('Ctrl Pts',(6.7585693453866,-0.385525513634243,130.284684890851));
#41242=CARTESIAN_POINT('Ctrl Pts',(6.76661493004098,-0.199529212419925,
130.293434632935));
#41243=CARTESIAN_POINT('Ctrl Pts',(6.76698649908906,-0.0135174386020487,
130.302184375019));
#41244=CARTESIAN_POINT('Ctrl Pts',(6.76735806132393,0.172490924444134,130.310933956665));
#41245=CARTESIAN_POINT('Ctrl Pts',(6.76005588896298,0.358514472899743,130.319683538311));
#41246=CARTESIAN_POINT('Ctrl Pts',(6.74510478454598,0.543921359660529,130.328433119957));
#41247=CARTESIAN_POINT('Ctrl Pts',(6.73015393440706,0.729325093148722,130.337182552796));
#41248=CARTESIAN_POINT('Ctrl Pts',(6.70755443556921,0.914111900254591,130.345931985635));
#41249=CARTESIAN_POINT('Ctrl Pts',(6.67738304682348,1.09765415591358,130.354681418474));
#41250=CARTESIAN_POINT('Ctrl Pts',(6.64721213111895,1.28119353391092,130.363430714135));
#41251=CARTESIAN_POINT('Ctrl Pts',(6.60946960955534,1.46348811672471,130.372180009797));
#41252=CARTESIAN_POINT('Ctrl Pts',(6.56428366991229,1.64391876348039,130.380929305458));
#41253=CARTESIAN_POINT('Ctrl Pts',(6.51909837867768,1.82434682109535,130.389678475569));
#41254=CARTESIAN_POINT('Ctrl Pts',(6.46646995271977,2.00291071820265,130.39842764568));
#41255=CARTESIAN_POINT('Ctrl Pts',(6.4065771328161,2.17900400212526,130.407176815791));
#41256=CARTESIAN_POINT('Ctrl Pts',(6.34668509279124,2.35509499309484,130.415925871976));
#41257=CARTESIAN_POINT('Ctrl Pts',(6.27952894037595,2.52871516397952,130.424674928162));
#41258=CARTESIAN_POINT('Ctrl Pts',(6.20533675061519,2.69927486771253,130.433423984348));
#41259=CARTESIAN_POINT('Ctrl Pts',(6.12832117907992,2.87632521635762,130.44250598563));
#41260=CARTESIAN_POINT('Ctrl Pts',(6.04372366626158,3.05007728919842,130.451587986912));
#41261=CARTESIAN_POINT('Ctrl Pts',(5.95185378007948,3.21989527478047,130.460669988195));
#41262=CARTESIAN_POINT('Ctrl Pts',(5.8633445081745,3.38350129286615,130.469419768502));
#41263=CARTESIAN_POINT('Ctrl Pts',(5.76808562057333,3.54345567124836,130.478169548809));
#41264=CARTESIAN_POINT('Ctrl Pts',(5.66640068804559,3.69921508465195,130.486919329116));
#41265=CARTESIAN_POINT('Ctrl Pts',(5.56471941107996,3.85496889852178,130.49566879487));
#41266=CARTESIAN_POINT('Ctrl Pts',(5.45661270815184,4.00652780919541,130.504418260623));
#41267=CARTESIAN_POINT('Ctrl Pts',(5.34244776449182,4.15337704569142,130.513167726377));
#41268=CARTESIAN_POINT('Ctrl Pts',(5.22828631819664,4.30022178356166,130.521916924096));
#41269=CARTESIAN_POINT('Ctrl Pts',(5.10806717844139,4.44235690972598,130.530666121816));
#41270=CARTESIAN_POINT('Ctrl Pts',(4.98219864544791,4.57929969070567,130.539415319535));
#41271=CARTESIAN_POINT('Ctrl Pts',(4.85633329944115,4.71623900429907,130.548164295726));
#41272=CARTESIAN_POINT('Ctrl Pts',(4.72481904033759,4.84798602483508,130.556913271916));
#41273=CARTESIAN_POINT('Ctrl Pts',(4.5881025073733,4.97409332259004,130.565662248106));
#41274=CARTESIAN_POINT('Ctrl Pts',(4.45137708685779,5.10020881822015,130.574411793042));
#41275=CARTESIAN_POINT('Ctrl Pts',(4.30944892636194,5.22068366307815,130.583161337978));
#41276=CARTESIAN_POINT('Ctrl Pts',(4.16280009466809,5.33510865604735,130.591910882915));
#41277=CARTESIAN_POINT('Ctrl Pts',(4.01615988348944,5.44952692272776,130.600659913523));
#41278=CARTESIAN_POINT('Ctrl Pts',(3.86479978232394,5.55789587288512,130.609408944131));
#41279=CARTESIAN_POINT('Ctrl Pts',(3.70923383581239,5.65984746713765,130.618157974739));
#41280=CARTESIAN_POINT('Ctrl Pts',(3.55366577799716,5.76180044505275,130.626907124087));
#41281=CARTESIAN_POINT('Ctrl Pts',(3.39389200027019,5.85733573570955,130.635656273435));
#41282=CARTESIAN_POINT('Ctrl Pts',(3.23045513626223,5.94612887621829,130.644405422783));
#41283=CARTESIAN_POINT('Ctrl Pts',(3.18695122151704,5.96976399206622,130.646734286896));
#41284=CARTESIAN_POINT('Ctrl Pts',(3.14318791262733,5.99292165435297,130.649063151009));
#41285=CARTESIAN_POINT('Ctrl Pts',(3.09917575053269,6.01559628526634,130.651392015122));
#41286=CARTESIAN_POINT('Origin',(0.,0.,-3.69717978381041));
#41287=CARTESIAN_POINT('',(3.09917575053245,6.01559628526646,133.045751582742));
#41288=CARTESIAN_POINT('',(3.09917575053271,6.01559628526633,132.65155107452));
#41289=CARTESIAN_POINT('',(3.09917575053259,6.01559628526639,-3.69717978381041));
#41290=CARTESIAN_POINT('',(-6.767,7.88350220065452E-12,131.69717978381));
#41291=CARTESIAN_POINT('Ctrl Pts',(-6.767,7.88350217244735E-12,131.69717978381));
#41292=CARTESIAN_POINT('Ctrl Pts',(-6.76700000000022,-0.186007249407913,
131.705929295616));
#41293=CARTESIAN_POINT('Ctrl Pts',(-6.75932637295481,-0.372014355519894,
131.714678807422));
#41294=CARTESIAN_POINT('Ctrl Pts',(-6.7440051826699,-0.557389537147543,
131.723428319228));
#41295=CARTESIAN_POINT('Ctrl Pts',(-6.72868405709726,-0.742763935804164,
131.732177794078));
#41296=CARTESIAN_POINT('Ctrl Pts',(-6.70571545653088,-0.927506129688081,
131.740927268929));
#41297=CARTESIAN_POINT('Ctrl Pts',(-6.67517739415761,-1.11098863924309,
131.74967674378));
#41298=CARTESIAN_POINT('Ctrl Pts',(-6.64463945823194,-1.29447038906024,
131.758426182402));
#41299=CARTESIAN_POINT('Ctrl Pts',(-6.60653217027259,-1.47669218227765,
131.767175621024));
#41300=CARTESIAN_POINT('Ctrl Pts',(-6.56098496116819,-1.65703510503695,
131.775925059646));
#41301=CARTESIAN_POINT('Ctrl Pts',(-6.51543793687633,-1.83737729603611,
131.784674462766));
#41302=CARTESIAN_POINT('Ctrl Pts',(-6.46245112202762,-2.0158403539666,131.793423865886));
#41303=CARTESIAN_POINT('Ctrl Pts',(-6.40220448416371,-2.19181813637767,
131.802173269006));
#41304=CARTESIAN_POINT('Ctrl Pts',(-6.34195808575328,-2.36779521935566,
131.810922637351));
#41305=CARTESIAN_POINT('Ctrl Pts',(-6.27445201489388,-2.54128677544449,
131.819672005697));
#41306=CARTESIAN_POINT('Ctrl Pts',(-6.19991555136349,-2.71170355237462,
131.828421374042));
#41307=CARTESIAN_POINT('Ctrl Pts',(-6.12537937789215,-2.88211966612697,
131.837170708339));
#41308=CARTESIAN_POINT('Ctrl Pts',(-6.04381298133804,-3.04946076210074,
131.845920042636));
#41309=CARTESIAN_POINT('Ctrl Pts',(-5.95549339426504,-3.21315848206488,
131.854669376933));
#41310=CARTESIAN_POINT('Ctrl Pts',(-5.86717414355368,-3.37685557859276,
131.863418677909));
#41311=CARTESIAN_POINT('Ctrl Pts',(-5.77210188986455,-3.53690907466958,
131.872167978884));
#41312=CARTESIAN_POINT('Ctrl Pts',(-5.67059953467294,-3.69277536784558,
131.88091727986));
#41313=CARTESIAN_POINT('Ctrl Pts',(-5.56909755762016,-3.8486410803543,131.889666548241));
#41314=CARTESIAN_POINT('Ctrl Pts',(-5.46116568338346,-4.00031938103901,
131.898415816621));
#41315=CARTESIAN_POINT('Ctrl Pts',(-5.34717048686418,-4.14729511662827,
131.907165085002));
#41316=CARTESIAN_POINT('Ctrl Pts',(-5.23317570555834,-4.29427031687655,
131.915914321515));
#41317=CARTESIAN_POINT('Ctrl Pts',(-5.11311782179134,-4.4365427598675,131.924663558027));
#41318=CARTESIAN_POINT('Ctrl Pts',(-4.98740459172355,-4.57362924147277,
131.93341279454));
#41319=CARTESIAN_POINT('Ctrl Pts',(-4.86169180911188,-4.71071523514066,
131.942161999911));
#41320=CARTESIAN_POINT('Ctrl Pts',(-4.73032391415806,-4.84261509316157,
131.950911205282));
#41321=CARTESIAN_POINT('Ctrl Pts',(-4.59374707237685,-4.96888084331161,
131.959660410653));
#41322=CARTESIAN_POINT('Ctrl Pts',(-4.45717070537813,-5.09514615452364,
131.96840958561));
#41323=CARTESIAN_POINT('Ctrl Pts',(-4.31538563819939,-5.21577720253277,
131.977158760566));
#41324=CARTESIAN_POINT('Ctrl Pts',(-4.16887341291097,-5.33036429028299,
131.985907935522));
#41325=CARTESIAN_POINT('Ctrl Pts',(-4.02236168477799,-5.44495098920836,
131.99465708079));
#41326=CARTESIAN_POINT('Ctrl Pts',(-3.87112305634911,-5.5534935923843,132.003406226058));
#41327=CARTESIAN_POINT('Ctrl Pts',(-3.71567117317216,-5.65562346102156,
132.012155371326));
#41328=CARTESIAN_POINT('Ctrl Pts',(-3.56021980457788,-5.75775299158468,
132.020904487632));
#41329=CARTESIAN_POINT('Ctrl Pts',(-3.40055544862878,-5.85346967275069,
132.029653603938));
#41330=CARTESIAN_POINT('Ctrl Pts',(-3.23722036323895,-5.94244842803293,
132.038402720244));
#41331=CARTESIAN_POINT('Ctrl Pts',(-3.07388580496573,-6.03142689616206,
132.047151808315));
#41332=CARTESIAN_POINT('Ctrl Pts',(-2.90688079258268,-6.11366734484555,
132.055900896386));
#41333=CARTESIAN_POINT('Ctrl Pts',(-2.73677251095211,-6.18889046787039,
132.064649984457));
#41334=CARTESIAN_POINT('Ctrl Pts',(-2.56666476417235,-6.26411335438029,
132.073399045019));
#41335=CARTESIAN_POINT('Ctrl Pts',(-2.39345402972676,-6.3323188435007,132.082148105582));
#41336=CARTESIAN_POINT('Ctrl Pts',(-2.21772856474614,-6.39327529620844,
132.090897166144));
#41337=CARTESIAN_POINT('Ctrl Pts',(-2.04200363768847,-6.45423156231899,
132.099646199924));
#41338=CARTESIAN_POINT('Ctrl Pts',(-1.86376426620672,-6.5079387425189,132.108395233704));
#41339=CARTESIAN_POINT('Ctrl Pts',(-1.68361578195268,-6.55421443795974,
132.117144267484));
#41340=CARTESIAN_POINT('Ctrl Pts',(-1.50346783420465,-6.60048999558543,
132.125893275208));
#41341=CARTESIAN_POINT('Ctrl Pts',(-1.3214110625786,-6.63933404145373,132.134642282932));
#41342=CARTESIAN_POINT('Ctrl Pts',(-1.13806375959673,-6.67061465526923,
132.143391290656));
#41343=CARTESIAN_POINT('Ctrl Pts',(-0.954716987425285,-6.70189517852394,
132.152140273051));
#41344=CARTESIAN_POINT('Ctrl Pts',(-0.770079973815841,-6.7256122653576,
132.160889255446));
#41345=CARTESIAN_POINT('Ctrl Pts',(-0.584779770558248,-6.74168536939732,
132.169638237841));
#41346=CARTESIAN_POINT('Ctrl Pts',(-0.391490647559707,-6.7584514394236,
132.178764418517));
#41347=CARTESIAN_POINT('Ctrl Pts',(-0.19748021311013,-6.7668997592401,132.187890599193));
#41348=CARTESIAN_POINT('Ctrl Pts',(-0.00346532630358167,-6.76699911271707,
132.197016779869));
#41349=CARTESIAN_POINT('Ctrl Pts',(0.184486595290358,-6.76709536139789,
132.205857767399));
#41350=CARTESIAN_POINT('Ctrl Pts',(0.372442378179628,-6.75935659726801,
132.214698754929));
#41351=CARTESIAN_POINT('Ctrl Pts',(0.559750217716585,-6.74380965729062,
132.223539742459));
#41352=CARTESIAN_POINT('Ctrl Pts',(0.745129914452264,-6.72842275717314,
132.232289721057));
#41353=CARTESIAN_POINT('Ctrl Pts',(0.929874656308712,-6.70538772273549,
132.241039699655));
#41354=CARTESIAN_POINT('Ctrl Pts',(1.11335688289232,-6.67478280180833,132.249789678252));
#41355=CARTESIAN_POINT('Ctrl Pts',(1.29683723118313,-6.64417819418129,132.258539567277));
#41356=CARTESIAN_POINT('Ctrl Pts',(1.47905480729694,-6.60600390230196,132.267289456302));
#41357=CARTESIAN_POINT('Ctrl Pts',(1.6593906480427,-6.5603895979727,132.276039345327));
#41358=CARTESIAN_POINT('Ctrl Pts',(1.83972470263724,-6.51477574543409,132.284789147688));
#41359=CARTESIAN_POINT('Ctrl Pts',(2.01817678125304,-6.4617220982027,132.293538950049));
#41360=CARTESIAN_POINT('Ctrl Pts',(2.19414072347133,-6.40140886724202,132.30228875241));
#41361=CARTESIAN_POINT('Ctrl Pts',(2.37010298131551,-6.34109621361578,132.311038471016));
#41362=CARTESIAN_POINT('Ctrl Pts',(2.54357687926368,-6.27352420826192,132.319788189621));
#41363=CARTESIAN_POINT('Ctrl Pts',(2.71397317789427,-6.19892237325734,132.328537908226));
#41364=CARTESIAN_POINT('Ctrl Pts',(2.88436790206668,-6.12432122757214,132.337287545985));
#41365=CARTESIAN_POINT('Ctrl Pts',(3.05168482125735,-6.0426904971768,132.346037183743));
#41366=CARTESIAN_POINT('Ctrl Pts',(3.2153556199688,-5.95430745235204,132.354786821501));
#41367=CARTESIAN_POINT('Ctrl Pts',(3.37902496074778,-5.86592519481806,132.36353638132));
#41368=CARTESIAN_POINT('Ctrl Pts',(3.53904799384379,-5.77079087940536,132.372285941139));
#41369=CARTESIAN_POINT('Ctrl Pts',(3.69488118814496,-5.66922763747342,132.381035500958));
#41370=CARTESIAN_POINT('Ctrl Pts',(3.85071304610356,-5.56766526649382,132.389784985746));
#41371=CARTESIAN_POINT('Ctrl Pts',(4.00235489705502,-5.45967423581056,132.398534470533));
#41372=CARTESIAN_POINT('Ctrl Pts',(4.14929168607199,-5.34562133936682,132.407283955321));
#41373=CARTESIAN_POINT('Ctrl Pts',(4.29622726385312,-5.23156938308896,132.416033367984));
#41374=CARTESIAN_POINT('Ctrl Pts',(4.43845763091632,-5.11145583677579,132.424782780647));
#41375=CARTESIAN_POINT('Ctrl Pts',(4.57549970660538,-4.985688662046,132.433532193311));
#41376=CARTESIAN_POINT('Ctrl Pts',(4.71254069814875,-4.85992248226568,132.442281536757));
#41377=CARTESIAN_POINT('Ctrl Pts',(4.84439326930899,-4.72850295734427,132.451030880203));
#41378=CARTESIAN_POINT('Ctrl Pts',(4.97060959434289,-4.59187644222125,132.45978022365));
#41379=CARTESIAN_POINT('Ctrl Pts',(5.09682496280114,-4.45525096257122,132.468529500786));
#41380=CARTESIAN_POINT('Ctrl Pts',(5.21740397615447,-4.313418782188,132.477278777922));
#41381=CARTESIAN_POINT('Ctrl Pts',(5.33193710451552,-4.16686161439166,132.486028055058));
#41382=CARTESIAN_POINT('Ctrl Pts',(5.44646940289019,-4.02030550865008,132.494777268791));
#41383=CARTESIAN_POINT('Ctrl Pts',(5.55495572749318,-3.86902470980632,132.503526482524));
#41384=CARTESIAN_POINT('Ctrl Pts',(5.65702762491127,-3.71353301466283,132.512275696257));
#41385=CARTESIAN_POINT('Ctrl Pts',(5.75909881654833,-3.55804239467412,132.521024849493));
#41386=CARTESIAN_POINT('Ctrl Pts',(5.85475551250471,-3.39834117620089,132.52977400273));
#41387=CARTESIAN_POINT('Ctrl Pts',(5.94367283727794,-3.23497174692523,132.538523155966));
#41388=CARTESIAN_POINT('Ctrl Pts',(6.03258957676021,-3.07160339301535,132.547272251611));
#41389=CARTESIAN_POINT('Ctrl Pts',(6.11476689685006,-2.90456712830089,132.556021347257));
#41390=CARTESIAN_POINT('Ctrl Pts',(6.18992570524996,-2.73443024476505,132.564770442902));
#41391=CARTESIAN_POINT('Ctrl Pts',(6.26508404388457,-2.5642944246362,132.573519483863));
#41392=CARTESIAN_POINT('Ctrl Pts',(6.33322384283097,-2.39105828656571,132.582268524824));
#41393=CARTESIAN_POINT('Ctrl Pts',(6.39411368719837,-2.21531017132647,132.591017565785));
#41394=CARTESIAN_POINT('Ctrl Pts',(6.45500317120708,-2.03956309620089,132.599766554968));
#41395=CARTESIAN_POINT('Ctrl Pts',(6.50864269269907,-1.86130434439216,132.60851554415));
#41396=CARTESIAN_POINT('Ctrl Pts',(6.55485008446182,-1.68113930720535,132.617264533333));
#41397=CARTESIAN_POINT('Ctrl Pts',(6.60199664749274,-1.49731239212417,132.626191346862));
#41398=CARTESIAN_POINT('Ctrl Pts',(6.64140563640796,-1.31150116500233,132.635118160391));
#41399=CARTESIAN_POINT('Ctrl Pts',(6.6729377228208,-1.12436255156207,132.644044973921));
#41400=CARTESIAN_POINT('Ctrl Pts',(6.70384494949795,-0.940932395056772,
132.652794888076));
#41401=CARTESIAN_POINT('Ctrl Pts',(6.7271844934887,-0.756227260512096,132.661544802232));
#41402=CARTESIAN_POINT('Ctrl Pts',(6.74287707373887,-0.570874564547019,
132.670294716387));
#41403=CARTESIAN_POINT('Ctrl Pts',(6.7585693453864,-0.385525513637769,132.679044458471));
#41404=CARTESIAN_POINT('Ctrl Pts',(6.76661493004088,-0.199529212423483,
132.687794200555));
#41405=CARTESIAN_POINT('Ctrl Pts',(6.76698649908906,-0.0135174386056353,
132.696543942639));
#41406=CARTESIAN_POINT('Ctrl Pts',(6.76735806132403,0.172490924440647,132.705293524285));
#41407=CARTESIAN_POINT('Ctrl Pts',(6.76005588896316,0.358514472896359,132.714043105931));
#41408=CARTESIAN_POINT('Ctrl Pts',(6.74510478454624,0.543921359657251,132.722792687577));
#41409=CARTESIAN_POINT('Ctrl Pts',(6.73015393440741,0.729325093145551,132.731542120416));
#41410=CARTESIAN_POINT('Ctrl Pts',(6.70755443556963,0.91411190025153,132.740291553255));
#41411=CARTESIAN_POINT('Ctrl Pts',(6.67738304682397,1.09765415591064,132.749040986094));
#41412=CARTESIAN_POINT('Ctrl Pts',(6.6472121311195,1.28119353390808,132.757790281755));
#41413=CARTESIAN_POINT('Ctrl Pts',(6.60946960955595,1.46348811672199,132.766539577417));
#41414=CARTESIAN_POINT('Ctrl Pts',(6.56428366991294,1.64391876347778,132.775288873078));
#41415=CARTESIAN_POINT('Ctrl Pts',(6.51909837867838,1.82434682109285,132.784038043189));
#41416=CARTESIAN_POINT('Ctrl Pts',(6.46646995272051,2.00291071820027,132.7927872133));
#41417=CARTESIAN_POINT('Ctrl Pts',(6.40657713281687,2.179004002123,132.801536383411));
#41418=CARTESIAN_POINT('Ctrl Pts',(6.34668509279213,2.35509499309245,132.810285439596));
#41419=CARTESIAN_POINT('Ctrl Pts',(6.27952894037695,2.52871516397701,132.819034495782));
#41420=CARTESIAN_POINT('Ctrl Pts',(6.20533675061634,2.6992748677099,132.827783551968));
#41421=CARTESIAN_POINT('Ctrl Pts',(6.1283211790811,2.87632521635512,132.83686555325));
#41422=CARTESIAN_POINT('Ctrl Pts',(6.04372366626278,3.05007728919604,132.845947554532));
#41423=CARTESIAN_POINT('Ctrl Pts',(5.9518537800807,3.21989527477821,132.855029555815));
#41424=CARTESIAN_POINT('Ctrl Pts',(5.86334450817586,3.38350129286379,132.863779336122));
#41425=CARTESIAN_POINT('Ctrl Pts',(5.76808562057483,3.54345567124591,132.872529116429));
#41426=CARTESIAN_POINT('Ctrl Pts',(5.66640068804725,3.69921508464941,132.881278896736));
#41427=CARTESIAN_POINT('Ctrl Pts',(5.56471941108171,3.85496889851926,132.890028362489));
#41428=CARTESIAN_POINT('Ctrl Pts',(5.45661270815367,4.00652780919292,132.898777828243));
#41429=CARTESIAN_POINT('Ctrl Pts',(5.34244776449373,4.15337704568896,132.907527293996));
#41430=CARTESIAN_POINT('Ctrl Pts',(5.22828631819872,4.30022178355912,132.916276491716));
#41431=CARTESIAN_POINT('Ctrl Pts',(5.10806717844365,4.44235690972338,132.925025689436));
#41432=CARTESIAN_POINT('Ctrl Pts',(4.98219864545034,4.57929969070303,132.933774887155));
#41433=CARTESIAN_POINT('Ctrl Pts',(4.8563332994435,4.71623900429666,132.942523863345));
#41434=CARTESIAN_POINT('Ctrl Pts',(4.72481904033984,4.84798602483289,132.951272839536));
#41435=CARTESIAN_POINT('Ctrl Pts',(4.58810250737544,4.97409332258807,132.960021815726));
#41436=CARTESIAN_POINT('Ctrl Pts',(4.45137708686001,5.10020881821822,132.968771360662));
#41437=CARTESIAN_POINT('Ctrl Pts',(4.30944892636423,5.22068366307626,132.977520905598));
#41438=CARTESIAN_POINT('Ctrl Pts',(4.16280009467045,5.33510865604551,132.986270450534));
#41439=CARTESIAN_POINT('Ctrl Pts',(4.01615988349198,5.44952692272589,132.995019481143));
#41440=CARTESIAN_POINT('Ctrl Pts',(3.86479978232666,5.55789587288323,133.003768511751));
#41441=CARTESIAN_POINT('Ctrl Pts',(3.70923383581529,5.65984746713575,133.012517542359));
#41442=CARTESIAN_POINT('Ctrl Pts',(3.55366577800013,5.76180044505091,133.021266691707));
#41443=CARTESIAN_POINT('Ctrl Pts',(3.39389200027324,5.85733573570779,133.030015841055));
#41444=CARTESIAN_POINT('Ctrl Pts',(3.23045513626535,5.94612887621659,133.038764990403));
#41445=CARTESIAN_POINT('Ctrl Pts',(3.18695122151905,5.96976399206515,133.041093854516));
#41446=CARTESIAN_POINT('Ctrl Pts',(3.14318791262822,5.99292165435252,133.043422718629));
#41447=CARTESIAN_POINT('Ctrl Pts',(3.09917575053245,6.01559628526646,133.045751582742));
#41448=CARTESIAN_POINT('Ctrl Pts',(3.09917575053245,6.01559628526646,131.045629062141));
#41449=CARTESIAN_POINT('Ctrl Pts',(2.94405850634437,6.09551115635822,131.053853674147));
#41450=CARTESIAN_POINT('Ctrl Pts',(2.78600859645521,6.1693398725509,131.062078286153));
#41451=CARTESIAN_POINT('Ctrl Pts',(2.62555104399233,6.23688790306438,131.070302898159));
#41452=CARTESIAN_POINT('Ctrl Pts',(2.514788762354,6.28351564893866,131.075980267516));
#41453=CARTESIAN_POINT('Ctrl Pts',(2.4028796157962,6.32715167023281,131.081657636872));
#41454=CARTESIAN_POINT('Ctrl Pts',(2.29000000142994,6.36774599002276,131.087335006229));
#41455=CARTESIAN_POINT('Ctrl Pts',(2.12793907730266,6.42602713331344,131.095485988403));
#41456=CARTESIAN_POINT('Ctrl Pts',(1.96339721235476,6.47820904559648,131.103636970578));
#41457=CARTESIAN_POINT('Ctrl Pts',(1.79687807751048,6.52407220795128,131.111787952752));
#41458=CARTESIAN_POINT('Ctrl Pts',(1.63055237007467,6.56988209599231,131.119929466805));
#41459=CARTESIAN_POINT('Ctrl Pts',(1.46225431362094,6.60938774845269,131.128070980858));
#41460=CARTESIAN_POINT('Ctrl Pts',(1.29250714134153,6.6424178045032,131.136212494911));
#41461=CARTESIAN_POINT('Ctrl Pts',(1.1229214251043,6.67541644381757,131.144346265114));
#41462=CARTESIAN_POINT('Ctrl Pts',(0.951889693599731,6.70195167961719,131.152480035317));
#41463=CARTESIAN_POINT('Ctrl Pts',(0.77994991477165,6.72190204707326,131.16061380552));
#41464=CARTESIAN_POINT('Ctrl Pts',(0.608137515021744,6.74183763459049,131.168741549938));
#41465=CARTESIAN_POINT('Ctrl Pts',(0.435418769161226,6.75519802525391,131.176869294356));
#41466=CARTESIAN_POINT('Ctrl Pts',(0.262341400720126,6.76191289425324,131.184997038774));
#41467=CARTESIAN_POINT('Ctrl Pts',(0.0893558659115955,6.76862420039038,
131.193120470668));
#41468=CARTESIAN_POINT('Ctrl Pts',(-0.0839875479063557,6.76869699295374,
131.201243902562));
#41469=CARTESIAN_POINT('Ctrl Pts',(-0.257136441490172,6.76211282444014,
131.209367334456));
#41470=CARTESIAN_POINT('Ctrl Pts',(-0.431383723550725,6.75548688855122,
131.217542298207));
#41471=CARTESIAN_POINT('Ctrl Pts',(-0.605433635510642,6.74211920427105,
131.225717261958));
#41472=CARTESIAN_POINT('Ctrl Pts',(-0.778723130219089,6.72204427882336,
131.233892225709));
#41473=CARTESIAN_POINT('Ctrl Pts',(-0.950881212740323,6.70210042315198,
131.242013814882));
#41474=CARTESIAN_POINT('Ctrl Pts',(-1.12228841344074,6.67553671810307,131.250135404055));
#41475=CARTESIAN_POINT('Ctrl Pts',(-1.29239808495552,6.64243902418406,131.258256993228));
#41476=CARTESIAN_POINT('Ctrl Pts',(-1.46253021443577,6.60933696069065,131.266379654617));
#41477=CARTESIAN_POINT('Ctrl Pts',(-1.63136411424499,6.56969926004439,131.274502316007));
#41478=CARTESIAN_POINT('Ctrl Pts',(-1.79836377829489,6.52366283010679,131.282624977396));
#41479=CARTESIAN_POINT('Ctrl Pts',(-1.96541729140136,6.47761155571825,131.290750257938));
#41480=CARTESIAN_POINT('Ctrl Pts',(-2.130635038348,6.42515754064479,131.29887553848));
#41481=CARTESIAN_POINT('Ctrl Pts',(-2.29349665427035,6.36648742218586,131.307000819023));
#41482=CARTESIAN_POINT('Ctrl Pts',(-2.45813261370486,6.30717810496019,131.31521462281));
#41483=CARTESIAN_POINT('Ctrl Pts',(-2.6203604408427,6.24151657467816,131.323428426598));
#41484=CARTESIAN_POINT('Ctrl Pts',(-2.77966465711112,6.16974500234875,131.331642230386));
#41485=CARTESIAN_POINT('Ctrl Pts',(-2.93752468753957,6.09862408127577,131.339781571241));
#41486=CARTESIAN_POINT('Ctrl Pts',(-3.09251359962079,6.02150366498666,131.347920912096));
#41487=CARTESIAN_POINT('Ctrl Pts',(-3.24415618652469,5.93866480258262,131.356060252952));
#41488=CARTESIAN_POINT('Ctrl Pts',(-3.39787973156745,5.85468916054131,131.364311288206));
#41489=CARTESIAN_POINT('Ctrl Pts',(-3.54816410673956,5.76483718973923,131.37256232346));
#41490=CARTESIAN_POINT('Ctrl Pts',(-3.69454655158716,5.66944572054054,131.380813358714));
#41491=CARTESIAN_POINT('Ctrl Pts',(-3.84092899643477,5.57405425134184,131.389064393968));
#41492=CARTESIAN_POINT('Ctrl Pts',(-3.98340923647753,5.47312356037056,131.397315429222));
#41493=CARTESIAN_POINT('Ctrl Pts',(-4.12156135075643,5.36703093264338,131.405566464476));
#41494=CARTESIAN_POINT('Ctrl Pts',(-4.25809289771122,5.26218280447902,131.413720712517));
#41495=CARTESIAN_POINT('Ctrl Pts',(-4.39083963367724,5.15195354324774,131.421874960558));
#41496=CARTESIAN_POINT('Ctrl Pts',(-4.51934434987102,5.03664726254369,131.430029208599));
#41497=CARTESIAN_POINT('Ctrl Pts',(-4.64769529331749,4.92147896092782,131.438173699013));
#41498=CARTESIAN_POINT('Ctrl Pts',(-4.77181405209426,4.80124597537327,131.446318189427));
#41499=CARTESIAN_POINT('Ctrl Pts',(-4.89127328872895,4.67629496663403,131.454462679841));
#41500=CARTESIAN_POINT('Ctrl Pts',(-5.01061475687302,4.55146714043063,131.462599141036));
#41501=CARTESIAN_POINT('Ctrl Pts',(-5.12530559718819,4.42193081397343,131.470735602231));
#41502=CARTESIAN_POINT('Ctrl Pts',(-5.23495242298611,4.28807207601176,131.478872063426));
#41503=CARTESIAN_POINT('Ctrl Pts',(-5.34451425144837,4.15431710426494,131.487002217301));
#41504=CARTESIAN_POINT('Ctrl Pts',(-5.44903962045856,4.01624667499518,131.495132371177));
#41505=CARTESIAN_POINT('Ctrl Pts',(-5.54817283983348,3.87428279031541,131.503262525053));
#41506=CARTESIAN_POINT('Ctrl Pts',(-5.64725193114259,3.73239641981848,131.511388239756));
#41507=CARTESIAN_POINT('Ctrl Pts',(-5.74094452676531,3.58662112671041,131.519513954459));
#41508=CARTESIAN_POINT('Ctrl Pts',(-5.82893598936872,3.43741097802432,131.527639669162));
#41509=CARTESIAN_POINT('Ctrl Pts',(-5.91690213338752,3.28824376293273,131.535763045779));
#41510=CARTESIAN_POINT('Ctrl Pts',(-5.99917022374606,3.13564397445797,131.543886422396));
#41511=CARTESIAN_POINT('Ctrl Pts',(-6.07546961088446,2.98009362390167,131.552009799013));
#41512=CARTESIAN_POINT('Ctrl Pts',(-6.15176159262743,2.82455837060762,131.560132387199));
#41513=CARTESIAN_POINT('Ctrl Pts',(-6.22208586332717,2.6660734540278,131.568254975385));
#41514=CARTESIAN_POINT('Ctrl Pts',(-6.28621832596571,2.50514433881421,131.576377563571));
#41515=CARTESIAN_POINT('Ctrl Pts',(-6.35035679321795,2.34420015608053,131.584500912261));
#41516=CARTESIAN_POINT('Ctrl Pts',(-6.40830216323169,2.18081165940008,131.592624260951));
#41517=CARTESIAN_POINT('Ctrl Pts',(-6.45987898538334,2.01550303750769,131.600747609641));
#41518=CARTESIAN_POINT('Ctrl Pts',(-6.51149544134953,1.85006738546904,131.608877200656));
#41519=CARTESIAN_POINT('Ctrl Pts',(-6.5567334623823,1.68270901015757,131.617006791671));
#41520=CARTESIAN_POINT('Ctrl Pts',(-6.59546767552983,1.51396669086249,131.625136382686));
#41521=CARTESIAN_POINT('Ctrl Pts',(-6.63421667542437,1.34515995435631,131.633269077165));
#41522=CARTESIAN_POINT('Ctrl Pts',(-6.66645684959307,1.17496858031579,131.641401771643));
#41523=CARTESIAN_POINT('Ctrl Pts',(-6.69211428126259,1.00393996161192,131.649534466122));
#41524=CARTESIAN_POINT('Ctrl Pts',(-6.71780393099843,0.832696582075747,
131.657677372834));
#41525=CARTESIAN_POINT('Ctrl Pts',(-6.73689427888086,0.660614220954811,
131.665820279546));
#41526=CARTESIAN_POINT('Ctrl Pts',(-6.74936337392912,0.488244863428358,
131.673963186258));
#41527=CARTESIAN_POINT('Ctrl Pts',(-6.76112933129812,0.325595488752011,
131.681646910928));
#41528=CARTESIAN_POINT('Ctrl Pts',(-6.76700018369326,0.162690847753514,
131.689330635598));
#41529=CARTESIAN_POINT('Ctrl Pts',(-6.76699999999569,-7.64039950798852E-6,
131.697014360268));
#41530=CARTESIAN_POINT('',(-6.76699999999398,6.3820334706712E-6,131.30295982093));
#41531=CARTESIAN_POINT('Ctrl Pts',(3.09917575053269,6.01559628526634,130.651392015122));
#41532=CARTESIAN_POINT('Ctrl Pts',(2.93382384459278,6.10078395293753,130.660141463035));
#41533=CARTESIAN_POINT('Ctrl Pts',(2.76495772123,6.17915010267042,130.668890910947));
#41534=CARTESIAN_POINT('Ctrl Pts',(2.5931509331673,6.25042856433169,130.67764035886));
#41535=CARTESIAN_POINT('Ctrl Pts',(2.42134553245638,6.32170645041443,130.68638973612));
#41536=CARTESIAN_POINT('Ctrl Pts',(2.24659977927614,6.38589665313449,130.69513911338));
#41537=CARTESIAN_POINT('Ctrl Pts',(2.06950718689944,6.44278115439067,130.70388849064));
#41538=CARTESIAN_POINT('Ctrl Pts',(1.89241596572888,6.49966521519716,130.712637800154));
#41539=CARTESIAN_POINT('Ctrl Pts',(1.71297821457226,6.54924360009538,130.721387109669));
#41540=CARTESIAN_POINT('Ctrl Pts',(1.53180337335875,6.59134792173549,130.730136419184));
#41541=CARTESIAN_POINT('Ctrl Pts',(1.3506298747781,6.63345193135299,130.73888566386));
#41542=CARTESIAN_POINT('Ctrl Pts',(1.16771959102975,6.66808192368234,130.747634908536));
#41543=CARTESIAN_POINT('Ctrl Pts',(0.983693746907036,6.69512028363166,130.756384153212));
#41544=CARTESIAN_POINT('Ctrl Pts',(0.799669205420017,6.72215845218865,130.765133335956));
#41545=CARTESIAN_POINT('Ctrl Pts',(0.614529402873574,6.74160505424578,130.7738825187));
#41546=CARTESIAN_POINT('Ctrl Pts',(0.428903127363299,6.75339404354122,130.782631701445));
#41547=CARTESIAN_POINT('Ctrl Pts',(0.243278104163778,6.76518295330331,130.791380825163));
#41548=CARTESIAN_POINT('Ctrl Pts',(0.0571669005388655,6.76931433552276,
130.800129948882));
#41549=CARTESIAN_POINT('Ctrl Pts',(-0.128798404777917,6.76577415902472,
130.8088790726));
#41550=CARTESIAN_POINT('Ctrl Pts',(-0.314762517259383,6.7622340052344,130.8176281402));
#41551=CARTESIAN_POINT('Ctrl Pts',(-0.500580446819676,6.75102239665087,
130.826377207799));
#41552=CARTESIAN_POINT('Ctrl Pts',(-0.685621118842659,6.73217741012497,
130.835126275398));
#41553=CARTESIAN_POINT('Ctrl Pts',(-0.87066066541428,6.71333253821774,130.843875289784));
#41554=CARTESIAN_POINT('Ctrl Pts',(-1.0549226788544,6.68685441030619,130.85262430417));
#41555=CARTESIAN_POINT('Ctrl Pts',(-1.23778137635181,6.6528329502819,130.861373318555));
#41556=CARTESIAN_POINT('Ctrl Pts',(-1.42999922978765,6.61707018861883,130.870570128923));
#41557=CARTESIAN_POINT('Ctrl Pts',(-1.62066601233604,6.57297172934435,130.87976693929));
#41558=CARTESIAN_POINT('Ctrl Pts',(-1.80906628500285,6.52070304311322,130.888963749658));
#41559=CARTESIAN_POINT('Ctrl Pts',(-1.9883134254542,6.47097374915064,130.897713747395));
#41560=CARTESIAN_POINT('Ctrl Pts',(-2.16550875896587,6.41384933989567,130.906463745133));
#41561=CARTESIAN_POINT('Ctrl Pts',(-2.3400503671389,6.34952386240521,130.915213742871));
#41562=CARTESIAN_POINT('Ctrl Pts',(-2.51458843546972,6.28519968948643,130.923963563152));
#41563=CARTESIAN_POINT('Ctrl Pts',(-2.68647261717942,6.21367483971148,130.932713383433));
#41564=CARTESIAN_POINT('Ctrl Pts',(-2.85511905908623,6.13519226743894,130.941463203713));
#41565=CARTESIAN_POINT('Ctrl Pts',(-3.02376230488774,6.05671118252992,130.950212858172));
#41566=CARTESIAN_POINT('Ctrl Pts',(-3.18916767379794,5.97127275992692,130.95896251263));
#41567=CARTESIAN_POINT('Ctrl Pts',(-3.35077334102676,5.8791672043806,130.967712167089));
#41568=CARTESIAN_POINT('Ctrl Pts',(-3.51237616037259,5.78706327195709,130.976461667357));
#41569=CARTESIAN_POINT('Ctrl Pts',(-3.67017916302193,5.68829258362367,130.985211167626));
#41570=CARTESIAN_POINT('Ctrl Pts',(-3.82364636566359,5.58319061741113,130.993960667894));
#41571=CARTESIAN_POINT('Ctrl Pts',(-3.97711106778695,5.47809036367777,131.002710025603));
#41572=CARTESIAN_POINT('Ctrl Pts',(-4.12623987481825,5.36665920043303,131.011459383311));
#41573=CARTESIAN_POINT('Ctrl Pts',(-4.27052628213828,5.24927559512417,131.02020874102));
#41574=CARTESIAN_POINT('Ctrl Pts',(-4.41481053024869,5.1318937464313,131.028957967796));
#41575=CARTESIAN_POINT('Ctrl Pts',(-4.55425230136413,5.00855981477459,131.037707194573));
#41576=CARTESIAN_POINT('Ctrl Pts',(-4.68837800630424,4.87969268192195,131.046456421349));
#41577=CARTESIAN_POINT('Ctrl Pts',(-4.82250188228764,4.75082730631941,131.05520552882));
#41578=CARTESIAN_POINT('Ctrl Pts',(-4.95130963052831,4.6164290790367,131.063954636291));
#41579=CARTESIAN_POINT('Ctrl Pts',(-5.07436379033227,4.47695444731848,131.072703743762));
#41580=CARTESIAN_POINT('Ctrl Pts',(-5.19741643562654,4.33748153220766,131.081452743551));
#41581=CARTESIAN_POINT('Ctrl Pts',(-5.31471544462612,4.19293255254792,131.090201743341));
#41582=CARTESIAN_POINT('Ctrl Pts',(-5.42586245275459,4.04379841779829,131.098950743131));
#41583=CARTESIAN_POINT('Ctrl Pts',(-5.53702160018986,3.89464799484579,131.107700698473));
#41584=CARTESIAN_POINT('Ctrl Pts',(-5.64202723081088,3.74091164444097,131.116450653815));
#41585=CARTESIAN_POINT('Ctrl Pts',(-5.74052265232807,3.58311159163489,131.125200609157));
#41586=CARTESIAN_POINT('Ctrl Pts',(-5.83901427066773,3.42531763192031,131.13395022664));
#41587=CARTESIAN_POINT('Ctrl Pts',(-5.93099603115609,3.26346052695851,131.142699844122));
#41588=CARTESIAN_POINT('Ctrl Pts',(-6.01615550622637,3.09809004467304,131.151449461605));
#41589=CARTESIAN_POINT('Ctrl Pts',(-6.10131214578692,2.93272506864051,131.160198787756));
#41590=CARTESIAN_POINT('Ctrl Pts',(-6.1796468232865,2.76384720417114,131.168948113907));
#41591=CARTESIAN_POINT('Ctrl Pts',(-6.25089348288475,2.59203002791808,131.177697440058));
#41592=CARTESIAN_POINT('Ctrl Pts',(-6.32213814889253,2.42021765937231,131.18644652139));
#41593=CARTESIAN_POINT('Ctrl Pts',(-6.38629508412519,2.24546640832106,131.195195602721));
#41594=CARTESIAN_POINT('Ctrl Pts',(-6.44314639819756,2.06836976660215,131.203944684053));
#41595=CARTESIAN_POINT('Ctrl Pts',(-6.50000285283649,1.8912571115845,131.212694556487));
#41596=CARTESIAN_POINT('Ctrl Pts',(-6.54955227673203,1.71179891440431,131.221444428922));
#41597=CARTESIAN_POINT('Ctrl Pts',(-6.59162635926344,1.53060476278608,131.230194301356));
#41598=CARTESIAN_POINT('Ctrl Pts',(-6.63369752055156,1.34942319164893,131.238943566278));
#41599=CARTESIAN_POINT('Ctrl Pts',(-6.66829431424215,1.16650618642922,131.247692831201));
#41600=CARTESIAN_POINT('Ctrl Pts',(-6.69529923745382,0.982474997620944,
131.256442096123));
#41601=CARTESIAN_POINT('Ctrl Pts',(-6.72230554731415,0.798434359180123,
131.265191810303));
#41602=CARTESIAN_POINT('Ctrl Pts',(-6.74171916496681,0.613279706242714,
131.273941524483));
#41603=CARTESIAN_POINT('Ctrl Pts',(-6.7534741481726,0.427639953657744,131.282691238662));
#41604=CARTESIAN_POINT('Ctrl Pts',(-6.76248837758727,0.285283364202196,
131.289400897838));
#41605=CARTESIAN_POINT('Ctrl Pts',(-6.76699999999984,0.142641701109999,
131.296110557014));
#41606=CARTESIAN_POINT('Ctrl Pts',(-6.767,7.70785566012505E-12,131.30282021619));
#41607=CARTESIAN_POINT('Ctrl Pts',(-6.76699999998758,1.29644361483994E-5,
131.303099416223));
#41608=CARTESIAN_POINT('Ctrl Pts',(-6.76700032597589,-0.170141975692278,
131.311122812505));
#41609=CARTESIAN_POINT('Ctrl Pts',(-6.76057857050752,-0.340538674351975,
131.319146208787));
#41610=CARTESIAN_POINT('Ctrl Pts',(-6.74770595799441,-0.510640092870492,
131.327169605069));
#41611=CARTESIAN_POINT('Ctrl Pts',(-6.73484484324927,-0.680589577456409,
131.335185834884));
#41612=CARTESIAN_POINT('Ctrl Pts',(-6.71554436537688,-0.850243933885984,
131.3432020647));
#41613=CARTESIAN_POINT('Ctrl Pts',(-6.68982777624885,-1.01906492635622,
131.351218294515));
#41614=CARTESIAN_POINT('Ctrl Pts',(-6.66412844176742,-1.18777264771769,
131.35922914581));
#41615=CARTESIAN_POINT('Ctrl Pts',(-6.63202162055116,-1.35564774722754,
131.367239997104));
#41616=CARTESIAN_POINT('Ctrl Pts',(-6.59358247779592,-1.52215607232066,
131.375250848398));
#41617=CARTESIAN_POINT('Ctrl Pts',(-6.55454584916757,-1.69125255013695,
131.383386217831));
#41618=CARTESIAN_POINT('Ctrl Pts',(-6.50897843464434,-1.85893901713537,
131.391521587263));
#41619=CARTESIAN_POINT('Ctrl Pts',(-6.45701324385285,-2.02466514977389,
131.399656956696));
#41620=CARTESIAN_POINT('Ctrl Pts',(-6.40586949160468,-2.18777157043,131.407663726465));
#41621=CARTESIAN_POINT('Ctrl Pts',(-6.34852886718192,-2.34897880902788,
131.415670496235));
#41622=CARTESIAN_POINT('Ctrl Pts',(-6.28516872439752,-2.50777652629879,
131.423677266004));
#41623=CARTESIAN_POINT('Ctrl Pts',(-6.22180617553912,-2.66658027384431,
131.431684339828));
#41624=CARTESIAN_POINT('Ctrl Pts',(-6.15242379264544,-2.82297396783599,
131.439691413651));
#41625=CARTESIAN_POINT('Ctrl Pts',(-6.07724728556253,-2.97646676953109,
131.447698487474));
#41626=CARTESIAN_POINT('Ctrl Pts',(-6.0020528154004,-3.12999624762236,131.45570747455));
#41627=CARTESIAN_POINT('Ctrl Pts',(-5.92106163175092,-3.28062311585741,
131.463716461627));
#41628=CARTESIAN_POINT('Ctrl Pts',(-5.83454555268109,-3.42788086048646,
131.471725448703));
#41629=CARTESIAN_POINT('Ctrl Pts',(-5.74562916691742,-3.57922413180548,
131.479956637543));
#41630=CARTESIAN_POINT('Ctrl Pts',(-5.65087709593312,-3.72700825724675,
131.488187826382));
#41631=CARTESIAN_POINT('Ctrl Pts',(-5.5506316478381,-3.87075926789798,131.496419015222));
#41632=CARTESIAN_POINT('Ctrl Pts',(-5.45293581359008,-4.01085415675773,
131.504440854376));
#41633=CARTESIAN_POINT('Ctrl Pts',(-5.35002292236622,-4.14711833637079,
131.512462693529));
#41634=CARTESIAN_POINT('Ctrl Pts',(-5.24224991833763,-4.2791476714048,131.520484532683));
#41635=CARTESIAN_POINT('Ctrl Pts',(-5.13025801062407,-4.41634545333438,
131.528820396365));
#41636=CARTESIAN_POINT('Ctrl Pts',(-5.01301810471143,-4.54896979008951,
131.537156260048));
#41637=CARTESIAN_POINT('Ctrl Pts',(-4.89097127108512,-4.67661084819124,
131.54549212373));
#41638=CARTESIAN_POINT('Ctrl Pts',(-4.7689244374589,-4.80425190629289,131.553827987412));
#41639=CARTESIAN_POINT('Ctrl Pts',(-4.64207105328817,-4.92690943361687,
131.562163851094));
#41640=CARTESIAN_POINT('Ctrl Pts',(-4.51088814299665,-5.04422215622709,
131.570499714777));
#41641=CARTESIAN_POINT('Ctrl Pts',(-4.38132322710275,-5.16008795768324,
131.578732764909));
#41642=CARTESIAN_POINT('Ctrl Pts',(-4.24710187528017,-5.27112797062188,
131.586965815041));
#41643=CARTESIAN_POINT('Ctrl Pts',(-4.10861753179622,-5.37694625018855,
131.595198865173));
#41644=CARTESIAN_POINT('Ctrl Pts',(-3.97029810187795,-5.48263851645035,
131.603422111007));
#41645=CARTESIAN_POINT('Ctrl Pts',(-3.82772607081388,-5.58312121613811,
131.611645356842));
#41646=CARTESIAN_POINT('Ctrl Pts',(-3.68133079907053,-5.67803597626986,
131.619868602677));
#41647=CARTESIAN_POINT('Ctrl Pts',(-3.53508056026301,-5.77285670490625,
131.628083701791));
#41648=CARTESIAN_POINT('Ctrl Pts',(-3.38501492242836,-5.86212028590153,
131.636298800904));
#41649=CARTESIAN_POINT('Ctrl Pts',(-3.23159539184113,-5.94550924845225,
131.644513900018));
#41650=CARTESIAN_POINT('Ctrl Pts',(-3.07829715692509,-6.02883228249866,
131.652722504157));
#41651=CARTESIAN_POINT('Ctrl Pts',(-2.92165062406743,-6.10628977884796,
131.660931108295));
#41652=CARTESIAN_POINT('Ctrl Pts',(-2.76214536475003,-6.17760811188197,
131.669139712434));
#41653=CARTESIAN_POINT('Ctrl Pts',(-2.60273430706811,-6.24888432527905,
131.677343468683));
#41654=CARTESIAN_POINT('Ctrl Pts',(-2.44046821240763,-6.3140284524504,131.685547224932));
#41655=CARTESIAN_POINT('Ctrl Pts',(-2.27586036665872,-6.37281323996491,
131.693750981181));
#41656=CARTESIAN_POINT('Ctrl Pts',(-2.11130122422227,-6.43158063454252,
131.701952310145));
#41657=CARTESIAN_POINT('Ctrl Pts',(-1.94440204645033,-6.48399231353383,
131.71015363911));
#41658=CARTESIAN_POINT('Ctrl Pts',(-1.77569540740306,-6.52986943362022,
131.718354968074));
#41659=CARTESIAN_POINT('Ctrl Pts',(-1.60701203461207,-6.57574022681373,
131.726555165997));
#41660=CARTESIAN_POINT('Ctrl Pts',(-1.4365220423951,-6.61507816117883,131.734755363919));
#41661=CARTESIAN_POINT('Ctrl Pts',(-1.26477247141517,-6.6477544776827,131.742955561842));
#41662=CARTESIAN_POINT('Ctrl Pts',(-1.0930154618235,-6.68043220942406,131.751156114922));
#41663=CARTESIAN_POINT('Ctrl Pts',(-0.919999116764714,-6.7064476814748,
131.759356668002));
#41664=CARTESIAN_POINT('Ctrl Pts',(-0.746280015309969,-6.72572339148355,
131.767557221082));
#41665=CARTESIAN_POINT('Ctrl Pts',(-0.57252190863849,-6.74500342947489,
131.775759615435));
#41666=CARTESIAN_POINT('Ctrl Pts',(-0.398061087323339,-6.75754065189055,
131.783962009788));
#41667=CARTESIAN_POINT('Ctrl Pts',(-0.22345864827241,-6.76330948815092,
131.792164404141));
#41668=CARTESIAN_POINT('Ctrl Pts',(-0.0486929252473757,-6.76908371928731,
131.800374469175));
#41669=CARTESIAN_POINT('Ctrl Pts',(0.126214321559992,-6.7680769063473,131.808584534209));
#41670=CARTESIAN_POINT('Ctrl Pts',(0.300701650334965,-6.7603156374156,131.816794599243));
#41671=CARTESIAN_POINT('Ctrl Pts',(0.475272485650197,-6.75255065407826,
131.825008593468));
#41672=CARTESIAN_POINT('Ctrl Pts',(0.649422645394069,-6.73802479931206,
131.833222587694));
#41673=CARTESIAN_POINT('Ctrl Pts',(0.822596479925594,-6.71681651016417,
131.841436581919));
#41674=CARTESIAN_POINT('Ctrl Pts',(0.996006408070551,-6.69557930705459,
131.849661774554));
#41675=CARTESIAN_POINT('Ctrl Pts',(1.16843699709867,-6.66764151965963,131.857886967189));
#41676=CARTESIAN_POINT('Ctrl Pts',(1.33934224092393,-6.63313284667787,131.866112159824));
#41677=CARTESIAN_POINT('Ctrl Pts',(1.49303696064819,-6.60209927097665,131.873509057944));
#41678=CARTESIAN_POINT('Ctrl Pts',(1.64549806404139,-6.56575230628646,131.880905956064));
#41679=CARTESIAN_POINT('Ctrl Pts',(1.79634011081175,-6.52422035237076,131.888302854184));
#41680=CARTESIAN_POINT('Ctrl Pts',(1.97265391974131,-6.47567515463612,131.896948820675));
#41681=CARTESIAN_POINT('Ctrl Pts',(2.14715575700586,-6.4199353649967,131.905594787166));
#41682=CARTESIAN_POINT('Ctrl Pts',(2.31925160685557,-6.35715038237243,131.914240753657));
#41683=CARTESIAN_POINT('Ctrl Pts',(2.49112732271792,-6.29444571027618,131.922875660781));
#41684=CARTESIAN_POINT('Ctrl Pts',(2.66060290294181,-6.2247139191908,131.931510567906));
#41685=CARTESIAN_POINT('Ctrl Pts',(2.82709861373037,-6.14815439203049,131.94014547503));
#41686=CARTESIAN_POINT('Ctrl Pts',(2.99912184773473,-6.06905315036136,131.949067054102));
#41687=CARTESIAN_POINT('Ctrl Pts',(3.16796363672579,-5.98266308812476,131.957988633173));
#41688=CARTESIAN_POINT('Ctrl Pts',(3.33300311075027,-5.88925965327808,131.966910212245));
#41689=CARTESIAN_POINT('Ctrl Pts',(3.49229830196621,-5.79910717247266,131.97552127122));
#41690=CARTESIAN_POINT('Ctrl Pts',(3.64805107999634,-5.70242143368215,131.984132330196));
#41691=CARTESIAN_POINT('Ctrl Pts',(3.79972431851457,-5.59949855820046,131.992743389172));
#41692=CARTESIAN_POINT('Ctrl Pts',(3.95125452216798,-5.49667274374104,132.001346327521));
#41693=CARTESIAN_POINT('Ctrl Pts',(4.09871260509386,-5.38762169024554,132.009949265871));
#41694=CARTESIAN_POINT('Ctrl Pts',(4.24158791781282,-5.27268631111925,132.01855220422));
#41695=CARTESIAN_POINT('Ctrl Pts',(4.38430324323248,-5.15787963302991,132.027145509269));
#41696=CARTESIAN_POINT('Ctrl Pts',(4.52244579881903,-5.03720196508959,132.035738814318));
#41697=CARTESIAN_POINT('Ctrl Pts',(4.6555355275429,-4.91103634193292,132.044332119367));
#41698=CARTESIAN_POINT('Ctrl Pts',(4.6703639017783,-4.89697942639369,132.045289554207));
#41699=CARTESIAN_POINT('Ctrl Pts',(4.68512958405555,-4.88285442823404,132.046246989047));
#41700=CARTESIAN_POINT('Ctrl Pts',(4.6998319347832,-4.86866190906619,132.047204423888));
#41701=CARTESIAN_POINT('Ctrl Pts',(4.83182821996074,-4.74124284240334,132.055800181436));
#41702=CARTESIAN_POINT('Ctrl Pts',(4.95856227028189,-4.60852753844506,132.064395938983));
#41703=CARTESIAN_POINT('Ctrl Pts',(5.0796294711552,-4.47097902430459,132.072991696531));
#41704=CARTESIAN_POINT('Ctrl Pts',(5.20080963184321,-4.33330217272376,132.081595474212));
#41705=CARTESIAN_POINT('Ctrl Pts',(5.31631218759829,-4.19078333891176,132.090199251894));
#41706=CARTESIAN_POINT('Ctrl Pts',(5.42577349237088,-4.04391777976327,132.098803029576));
#41707=CARTESIAN_POINT('Ctrl Pts',(5.53953672213847,-3.891280275715,132.107744943244));
#41708=CARTESIAN_POINT('Ctrl Pts',(5.6467740307585,-3.73394778668705,132.116686856912));
#41709=CARTESIAN_POINT('Ctrl Pts',(5.74712813021583,-3.57250713853478,132.12562877058));
#41710=CARTESIAN_POINT('Ctrl Pts',(5.84395025944658,-3.41674840637513,132.13425597291));
#41711=CARTESIAN_POINT('Ctrl Pts',(5.93436532832941,-3.25716604273515,132.142883175241));
#41712=CARTESIAN_POINT('Ctrl Pts',(6.01810032870807,-3.09431049405257,132.151510377572));
#41713=CARTESIAN_POINT('Ctrl Pts',(6.10191507385792,-2.93129985038691,132.160145795992));
#41714=CARTESIAN_POINT('Ctrl Pts',(6.17903692088215,-2.76501007464464,132.168781214413));
#41715=CARTESIAN_POINT('Ctrl Pts',(6.24924085912893,-2.59601188067265,132.177416632833));
#41716=CARTESIAN_POINT('Ctrl Pts',(6.31954851369482,-2.42676401594067,132.186064808854));
#41717=CARTESIAN_POINT('Ctrl Pts',(6.38291772654913,-2.25480002161542,132.194712984876));
#41718=CARTESIAN_POINT('Ctrl Pts',(6.43917272794045,-2.08070747096941,132.203361160897));
#41719=CARTESIAN_POINT('Ctrl Pts',(6.44512429378552,-2.06228913921792,132.204276105128));
#41720=CARTESIAN_POINT('Ctrl Pts',(6.45099627827213,-2.04384699361859,132.20519104936));
#41721=CARTESIAN_POINT('Ctrl Pts',(6.45678850658372,-2.0253817371667,132.206105993592));
#41722=CARTESIAN_POINT('Ctrl Pts',(6.50886471542337,-1.85936608661941,132.214331986133));
#41723=CARTESIAN_POINT('Ctrl Pts',(6.55460232139394,-1.69112279244775,132.222557978675));
#41724=CARTESIAN_POINT('Ctrl Pts',(6.59380855299048,-1.52117644161011,132.230783971216));
#41725=CARTESIAN_POINT('Ctrl Pts',(6.63297368192087,-1.35140825755458,132.239001339867));
#41726=CARTESIAN_POINT('Ctrl Pts',(6.66562099211021,-1.17994091854675,132.247218708519));
#41727=CARTESIAN_POINT('Ctrl Pts',(6.69160700651859,-1.00731557632714,132.25543607717));
#41728=CARTESIAN_POINT('Ctrl Pts',(6.71757097763852,-0.834836667883547,
132.263646475233));
#41729=CARTESIAN_POINT('Ctrl Pts',(6.73688485389486,-0.661202064928187,
132.271856873295));
#41730=CARTESIAN_POINT('Ctrl Pts',(6.74945586139615,-0.486964654841808,
132.280067271357));
#41731=CARTESIAN_POINT('Ctrl Pts',(6.76201871992094,-0.312840191673998,
132.288272347146));
#41732=CARTESIAN_POINT('Ctrl Pts',(6.76784739065311,-0.138114055824268,
132.296477422935));
#41733=CARTESIAN_POINT('Ctrl Pts',(6.76690072919752,0.0366540746184688,
132.304682498724));
#41734=CARTESIAN_POINT('Ctrl Pts',(6.7659544920707,0.211343867503229,132.312883896693));
#41735=CARTESIAN_POINT('Ctrl Pts',(6.75823897519756,0.386075259944744,132.321085294663));
#41736=CARTESIAN_POINT('Ctrl Pts',(6.74376509872549,0.560286795500323,132.329286692632));
#41737=CARTESIAN_POINT('Ctrl Pts',(6.729292355968,0.734484685357088,132.3374874482));
#41738=CARTESIAN_POINT('Ctrl Pts',(6.70806232900693,0.908162441941088,132.345688203768));
#41739=CARTESIAN_POINT('Ctrl Pts',(6.68013797862818,1.08076157707862,132.353888959336));
#41740=CARTESIAN_POINT('Ctrl Pts',(6.65221377009181,1.25335983549483,132.362089673247));
#41741=CARTESIAN_POINT('Ctrl Pts',(6.61759536205288,1.42487912943406,132.370290387159));
#41742=CARTESIAN_POINT('Ctrl Pts',(6.57639721507449,1.5947691587062,132.378491101071));
#41743=CARTESIAN_POINT('Ctrl Pts',(6.53519181123308,1.76468911332114,132.386693259501));
#41744=CARTESIAN_POINT('Ctrl Pts',(6.4874044438204,1.93297888321195,132.39489541793));
#41745=CARTESIAN_POINT('Ctrl Pts',(6.43320003320356,2.09910131551333,132.40309757636));
#41746=CARTESIAN_POINT('Ctrl Pts',(6.37897625143767,2.26528311535249,132.411302666013));
#41747=CARTESIAN_POINT('Ctrl Pts',(6.31833096923049,2.42929569418225,132.419507755666));
#41748=CARTESIAN_POINT('Ctrl Pts',(6.25147803739596,2.59061987716377,132.427712845319));
#41749=CARTESIAN_POINT('Ctrl Pts',(6.18454873399093,2.75212835395074,132.435927308317));
#41750=CARTESIAN_POINT('Ctrl Pts',(6.11139775071242,2.91094196781649,132.444141771314));
#41751=CARTESIAN_POINT('Ctrl Pts',(6.03228635158229,3.06656328363105,132.452356234312));
#41752=CARTESIAN_POINT('Ctrl Pts',(5.95312808144862,3.22227680015656,132.46057556412));
#41753=CARTESIAN_POINT('Ctrl Pts',(5.86800253047451,3.37479393606735,132.468794893927));
#41754=CARTESIAN_POINT('Ctrl Pts',(5.77721541901727,3.52364456241959,132.477014223735));
#41755=CARTESIAN_POINT('Ctrl Pts',(5.68628763843497,3.672725823793,132.485246288895));
#41756=CARTESIAN_POINT('Ctrl Pts',(5.58968096518597,3.81812892439933,132.493478354056));
#41757=CARTESIAN_POINT('Ctrl Pts',(5.48774346832688,3.95941417710192,132.501710419217));
#41758=CARTESIAN_POINT('Ctrl Pts',(5.3961147266374,4.08641150706691,132.509109990478));
#41759=CARTESIAN_POINT('Ctrl Pts',(5.30017950148412,4.21008203931098,132.516509561739));
#41760=CARTESIAN_POINT('Ctrl Pts',(5.20021631297347,4.33013155669485,132.523909133));
#41761=CARTESIAN_POINT('Ctrl Pts',(5.09002475574849,4.46246470314334,132.532065838405));
#41762=CARTESIAN_POINT('Ctrl Pts',(4.97459879515334,4.59080481309166,132.54022254381));
#41763=CARTESIAN_POINT('Ctrl Pts',(4.85425964675934,4.71470595921357,132.548379249216));
#41764=CARTESIAN_POINT('Ctrl Pts',(4.73406400826925,4.83845934758739,132.556526227379));
#41765=CARTESIAN_POINT('Ctrl Pts',(4.60896709600273,4.95778404897345,132.564673205542));
#41766=CARTESIAN_POINT('Ctrl Pts',(4.47933159729462,5.07226551370076,132.572820183705));
#41767=CARTESIAN_POINT('Ctrl Pts',(4.34985683951493,5.18660502767299,132.580957060061));
#41768=CARTESIAN_POINT('Ctrl Pts',(4.21585497965262,5.29611302958615,132.589093936417));
#41769=CARTESIAN_POINT('Ctrl Pts',(4.07772660760713,5.40041060601996,132.597230812773));
#41770=CARTESIAN_POINT('Ctrl Pts',(3.93969708384112,5.50463354437739,132.605361866168));
#41771=CARTESIAN_POINT('Ctrl Pts',(3.79754721515286,5.60365325874456,132.613492919562));
#41772=CARTESIAN_POINT('Ctrl Pts',(3.65171221038628,5.69712970999571,132.621623972956));
#41773=CARTESIAN_POINT('Ctrl Pts',(3.50596741225155,5.79054834113817,132.629749996865));
#41774=CARTESIAN_POINT('Ctrl Pts',(3.35654232549878,5.87843034232569,132.637876020775));
#41775=CARTESIAN_POINT('Ctrl Pts',(3.20390264998644,5.96047790109232,132.646002044684));
#41776=CARTESIAN_POINT('Ctrl Pts',(3.16915822380653,5.97915387992443,132.647851721296));
#41777=CARTESIAN_POINT('Ctrl Pts',(3.1342473592408,5.99752773909303,132.649701397908));
#41778=CARTESIAN_POINT('Ctrl Pts',(3.09917575053271,6.01559628526633,132.65155107452));
#41779=CARTESIAN_POINT('Origin',(0.,0.,-3.69717978381041));
#41780=CARTESIAN_POINT('',(3.09917575053244,6.01559628526647,135.045784814338));
#41781=CARTESIAN_POINT('',(3.09917575053266,6.01559628526635,134.651234928213));
#41782=CARTESIAN_POINT('',(3.09917575053259,6.01559628526639,-3.69717978381041));
#41783=CARTESIAN_POINT('',(-6.76699999998776,1.28714121708955E-5,133.697456813947));
#41784=CARTESIAN_POINT('Ctrl Pts',(-6.76699999998776,1.28714121708955E-5,
133.697456813947));
#41785=CARTESIAN_POINT('Ctrl Pts',(-6.76700032527401,-0.171002714082819,
133.705521296298));
#41786=CARTESIAN_POINT('Ctrl Pts',(-6.76051347811588,-0.342244911284379,
133.713585778649));
#41787=CARTESIAN_POINT('Ctrl Pts',(-6.7475138736617,-0.513172022564486,
133.721650260999));
#41788=CARTESIAN_POINT('Ctrl Pts',(-6.73452560713797,-0.683950055485557,
133.72970770971));
#41789=CARTESIAN_POINT('Ctrl Pts',(-6.71503591741793,-0.854413179796611,
133.73776515842));
#41790=CARTESIAN_POINT('Ctrl Pts',(-6.68907126218211,-1.02401887162759,
133.745822607131));
#41791=CARTESIAN_POINT('Ctrl Pts',(-6.66312357564471,-1.19351372093789,
133.753874790051));
#41792=CARTESIAN_POINT('Ctrl Pts',(-6.63070940404323,-1.36215188586963,
133.761926972972));
#41793=CARTESIAN_POINT('Ctrl Pts',(-6.59190709710128,-1.52939524753605,
133.769979155893));
#41794=CARTESIAN_POINT('Ctrl Pts',(-6.55311856901176,-1.69657922042424,
133.778028479451));
#41795=CARTESIAN_POINT('Ctrl Pts',(-6.50794650233443,-1.86236901246893,
133.78607780301));
#41796=CARTESIAN_POINT('Ctrl Pts',(-6.45652048573947,-2.02623597274024,
133.794127126569));
#41797=CARTESIAN_POINT('Ctrl Pts',(-6.40510272581285,-2.19007662346568,
133.802175157774));
#41798=CARTESIAN_POINT('Ctrl Pts',(-6.34743312544498,-2.35199470073605,
133.810223188979));
#41799=CARTESIAN_POINT('Ctrl Pts',(-6.28369131190787,-2.51147615888616,
133.818271220184));
#41800=CARTESIAN_POINT('Ctrl Pts',(-6.21994712371109,-2.67096355841392,
133.826319551213));
#41801=CARTESIAN_POINT('Ctrl Pts',(-6.1501304108429,-2.82801381168899,133.834367882243));
#41802=CARTESIAN_POINT('Ctrl Pts',(-6.074469112433,-2.9821324588451,133.842416213272));
#41803=CARTESIAN_POINT('Ctrl Pts',(-5.99879002679068,-3.13628733779016,
133.850466436385));
#41804=CARTESIAN_POINT('Ctrl Pts',(-5.91726378593629,-3.28750890436765,
133.858516659499));
#41805=CARTESIAN_POINT('Ctrl Pts',(-5.83016440604902,-3.4353270584384,133.866566882612));
#41806=CARTESIAN_POINT('Ctrl Pts',(-5.74298475381357,-3.58328144436692,
133.874624524955));
#41807=CARTESIAN_POINT('Ctrl Pts',(-5.65022189619028,-3.72782583301491,
133.882682167298));
#41808=CARTESIAN_POINT('Ctrl Pts',(-5.55219368370658,-3.86851835960601,
133.890739809641));
#41809=CARTESIAN_POINT('Ctrl Pts',(-5.45411471478756,-4.0092837330944,133.89880162402));
#41810=CARTESIAN_POINT('Ctrl Pts',(-5.3507651851877,-4.14619297502003,133.906863438399));
#41811=CARTESIAN_POINT('Ctrl Pts',(-5.24250308656071,-4.27883750420618,
133.914925252778));
#41812=CARTESIAN_POINT('Ctrl Pts',(-5.13410347514908,-4.41165051634998,
133.922997307144));
#41813=CARTESIAN_POINT('Ctrl Pts',(-5.02077908181994,-4.54018772098142,
133.93106936151));
#41814=CARTESIAN_POINT('Ctrl Pts',(-4.90292507915519,-4.66407704355225,
133.939141415877));
#41815=CARTESIAN_POINT('Ctrl Pts',(-4.84317738311493,-4.72688442743595,
133.943233654068));
#41816=CARTESIAN_POINT('Ctrl Pts',(-4.78226606659154,-4.78849787873628,
133.947325892259));
#41817=CARTESIAN_POINT('Ctrl Pts',(-4.72024576960563,-4.84887294889443,
133.951418130451));
#41818=CARTESIAN_POINT('Ctrl Pts',(-4.58921478455554,-4.97642804456073,
133.960063848503));
#41819=CARTESIAN_POINT('Ctrl Pts',(-4.45289322364292,-5.0987828514879,133.968709566555));
#41820=CARTESIAN_POINT('Ctrl Pts',(-4.31171019670708,-5.21550037672439,
133.977355284608));
#41821=CARTESIAN_POINT('Ctrl Pts',(-4.17070842000576,-5.33206806044465,
133.98598990332));
#41822=CARTESIAN_POINT('Ctrl Pts',(-4.02485785635243,-5.4430127002739,133.994624522033));
#41823=CARTESIAN_POINT('Ctrl Pts',(-3.8746235271258,-5.5479348881402,134.003259140745));
#41824=CARTESIAN_POINT('Ctrl Pts',(-3.7190835050056,-5.65656252009112,134.012198700647));
#41825=CARTESIAN_POINT('Ctrl Pts',(-3.55884464090013,-5.75873431260608,
134.02113826055));
#41826=CARTESIAN_POINT('Ctrl Pts',(-3.3944618206614,-5.85405141317294,134.030077820452));
#41827=CARTESIAN_POINT('Ctrl Pts',(-3.23612701624646,-5.94586158198338,
134.038688473723));
#41828=CARTESIAN_POINT('Ctrl Pts',(-3.07394802526566,-6.03131224641852,
134.047299126993));
#41829=CARTESIAN_POINT('Ctrl Pts',(-2.90845186068453,-6.11008975172057,
134.055909780264));
#41830=CARTESIAN_POINT('Ctrl Pts',(-2.74311234929429,-6.18879268884391,
134.064512282975));
#41831=CARTESIAN_POINT('Ctrl Pts',(-2.57446219895012,-6.260834929767,134.073114785686));
#41832=CARTESIAN_POINT('Ctrl Pts',(-2.40305368239629,-6.32594830831881,
134.081717288397));
#41833=CARTESIAN_POINT('Ctrl Pts',(-2.23183808267917,-6.39098840307312,
134.090310109165));
#41834=CARTESIAN_POINT('Ctrl Pts',(-2.05787059461596,-6.44911508474629,
134.098902929932));
#41835=CARTESIAN_POINT('Ctrl Pts',(-1.8817243613191,-6.50010787818312,134.1074957507));
#41836=CARTESIAN_POINT('Ctrl Pts',(-1.8609647276262,-6.50611761051127,134.108508453658));
#41837=CARTESIAN_POINT('Ctrl Pts',(-1.84017485500911,-6.51202831013581,
134.109521156616));
#41838=CARTESIAN_POINT('Ctrl Pts',(-1.81935569972229,-6.517839660339,134.110533859574));
#41839=CARTESIAN_POINT('Ctrl Pts',(-1.64265432386261,-6.56716315893246,
134.119129117334));
#41840=CARTESIAN_POINT('Ctrl Pts',(-1.46405013740167,-6.60926775687536,
134.127724375094));
#41841=CARTESIAN_POINT('Ctrl Pts',(-1.28414726211396,-6.64403904332336,
134.136319632854));
#41842=CARTESIAN_POINT('Ctrl Pts',(-1.10407591541294,-6.67884289160653,
134.144922939708));
#41843=CARTESIAN_POINT('Ctrl Pts',(-0.922703752168723,-6.70629966298467,
134.153526246563));
#41844=CARTESIAN_POINT('Ctrl Pts',(-0.740641937071527,-6.7263465953704,
134.162129553417));
#41845=CARTESIAN_POINT('Ctrl Pts',(-0.551031775985763,-6.74722468052463,
134.171089556357));
#41846=CARTESIAN_POINT('Ctrl Pts',(-0.36067393837606,-6.76006537669041,
134.180049559297));
#41847=CARTESIAN_POINT('Ctrl Pts',(-0.170259600931682,-6.76485777147536,
134.189009562237));
#41848=CARTESIAN_POINT('Ctrl Pts',(0.0130745613519903,-6.76947197067393,
134.197636405442));
#41849=CARTESIAN_POINT('Ctrl Pts',(0.196460802399278,-6.76662564682148,
134.206263248647));
#41850=CARTESIAN_POINT('Ctrl Pts',(0.379286276252665,-6.75636225498947,
134.214890091852));
#41851=CARTESIAN_POINT('Ctrl Pts',(0.562286485044416,-6.74608905394925,
134.223525180138));
#41852=CARTESIAN_POINT('Ctrl Pts',(0.744724553152227,-6.72838466137047,
134.232160268424));
#41853=CARTESIAN_POINT('Ctrl Pts',(0.925994478508959,-6.70334418225492,
134.24079535671));
#41854=CARTESIAN_POINT('Ctrl Pts',(1.10753362608138,-6.67826651300287,134.249443269835));
#41855=CARTESIAN_POINT('Ctrl Pts',(1.28790086302661,-6.64583103379531,134.25809118296));
#41856=CARTESIAN_POINT('Ctrl Pts',(1.46650059224313,-6.60618384643892,134.266739096085));
#41857=CARTESIAN_POINT('Ctrl Pts',(1.48653676300824,-6.60173603557317,134.267709260289));
#41858=CARTESIAN_POINT('Ctrl Pts',(1.50655070520403,-6.59719751376894,134.268679424493));
#41859=CARTESIAN_POINT('Ctrl Pts',(1.52654159070996,-6.59256852613856,134.269649588698));
#41860=CARTESIAN_POINT('Ctrl Pts',(1.6960166402935,-6.55332574682559,134.277874268216));
#41861=CARTESIAN_POINT('Ctrl Pts',(1.86420083684811,-6.50749201675033,134.286098947735));
#41862=CARTESIAN_POINT('Ctrl Pts',(2.03054439742182,-6.45516680265498,134.294323627254));
#41863=CARTESIAN_POINT('Ctrl Pts',(2.19671311209436,-6.40289658827937,134.302539661704));
#41864=CARTESIAN_POINT('Ctrl Pts',(2.3610447044058,-6.34414858412145,134.310755696154));
#41865=CARTESIAN_POINT('Ctrl Pts',(2.52300007342333,-6.27907315051401,134.318971730604));
#41866=CARTESIAN_POINT('Ctrl Pts',(2.68481764897097,-6.21405308382559,134.327180774759));
#41867=CARTESIAN_POINT('Ctrl Pts',(2.84426269701035,-6.14271644234302,134.335389818914));
#41868=CARTESIAN_POINT('Ctrl Pts',(3.00081167785889,-6.0652632485347,134.343598863068));
#41869=CARTESIAN_POINT('Ctrl Pts',(3.15725881323326,-5.98786044315566,134.351802566696));
#41870=CARTESIAN_POINT('Ctrl Pts',(3.31081331424066,-5.90434917007936,134.360006270324));
#41871=CARTESIAN_POINT('Ctrl Pts',(3.46097193714386,-5.81497740754878,134.368209973952));
#41872=CARTESIAN_POINT('Ctrl Pts',(3.61106293435191,-5.72564589463857,134.376409982946));
#41873=CARTESIAN_POINT('Ctrl Pts',(3.75776079303372,-5.63045933349806,134.38460999194));
#41874=CARTESIAN_POINT('Ctrl Pts',(3.90058710925378,-5.5297114936607,134.392810000934));
#41875=CARTESIAN_POINT('Ctrl Pts',(4.04340200478046,-5.42897170983302,134.401009354238));
#41876=CARTESIAN_POINT('Ctrl Pts',(4.18234567677989,-5.32267173236167,134.409208707542));
#41877=CARTESIAN_POINT('Ctrl Pts',(4.31696864292013,-5.21114869640508,134.417408060846));
#41878=CARTESIAN_POINT('Ctrl Pts',(4.45159073135833,-5.09962638754579,134.425607360692));
#41879=CARTESIAN_POINT('Ctrl Pts',(4.58189189326765,-4.98288131590588,134.433806660539));
#41880=CARTESIAN_POINT('Ctrl Pts',(4.70745579587629,-4.86129087073287,134.442005960386));
#41881=CARTESIAN_POINT('Ctrl Pts',(4.83304165836984,-4.73967916059336,134.450206694209));
#41882=CARTESIAN_POINT('Ctrl Pts',(4.9538883533594,-4.61322063800784,134.458407428032));
#41883=CARTESIAN_POINT('Ctrl Pts',(5.06961644808113,-4.48232953600528,134.466608161855));
#41884=CARTESIAN_POINT('Ctrl Pts',(5.18538577694114,-4.35139179725636,134.474811817615));
#41885=CARTESIAN_POINT('Ctrl Pts',(5.29603263517155,-4.21601860139181,134.483015473375));
#41886=CARTESIAN_POINT('Ctrl Pts',(5.40121788135593,-4.07665725786715,134.491219129135));
#41887=CARTESIAN_POINT('Ctrl Pts',(5.50652362400182,-3.93713626696442,134.49943218271));
#41888=CARTESIAN_POINT('Ctrl Pts',(5.60635503863194,-3.79361828734885,134.507645236285));
#41889=CARTESIAN_POINT('Ctrl Pts',(5.70041574739976,-3.64658049503873,134.51585828986));
#41890=CARTESIAN_POINT('Ctrl Pts',(5.79453211399928,-3.49945569716798,134.524076203283));
#41891=CARTESIAN_POINT('Ctrl Pts',(5.88287078699965,-3.34880724365436,134.532294116706));
#41892=CARTESIAN_POINT('Ctrl Pts',(5.9651814579846,-3.19513680040727,134.540512030129));
#41893=CARTESIAN_POINT('Ctrl Pts',(6.04762050585149,-3.04122668310437,134.548742760725));
#41894=CARTESIAN_POINT('Ctrl Pts',(6.12401260637912,-2.8842854790704,134.556973491321));
#41895=CARTESIAN_POINT('Ctrl Pts',(6.19415515056027,-2.72483595300481,134.565204221917));
#41896=CARTESIAN_POINT('Ctrl Pts',(6.25857268850193,-2.57840063311418,134.572763163592));
#41897=CARTESIAN_POINT('Ctrl Pts',(6.31771970627631,-2.42985014992169,134.580322105268));
#41898=CARTESIAN_POINT('Ctrl Pts',(6.37147664884281,-2.27959959494004,134.587881046944));
#41899=CARTESIAN_POINT('Ctrl Pts',(6.42946470215801,-2.11752309324662,134.596034939111));
#41900=CARTESIAN_POINT('Ctrl Pts',(6.48135939587856,-1.95296701905082,134.604188831277));
#41901=CARTESIAN_POINT('Ctrl Pts',(6.52693973994569,-1.7864340545113,134.612342723444));
#41902=CARTESIAN_POINT('Ctrl Pts',(6.57246446325864,-1.62010430671513,134.620486665584));
#41903=CARTESIAN_POINT('Ctrl Pts',(6.61169007900027,-1.45180281922105,134.628630607725));
#41904=CARTESIAN_POINT('Ctrl Pts',(6.64444366253621,-1.28205203302455,134.636774549865));
#41905=CARTESIAN_POINT('Ctrl Pts',(6.67716417152547,-1.11247266105808,134.644910268258));
#41906=CARTESIAN_POINT('Ctrl Pts',(6.70342559035815,-0.941447260260673,
134.653045986651));
#41907=CARTESIAN_POINT('Ctrl Pts',(6.72310481979071,-0.76951321113216,134.661181705044));
#41908=CARTESIAN_POINT('Ctrl Pts',(6.74276831668116,-0.597716614523205,
134.669310919344));
#41909=CARTESIAN_POINT('Ctrl Pts',(6.75586006022769,-0.42501317753814,134.677440133644));
#41910=CARTESIAN_POINT('Ctrl Pts',(6.76230804334633,-0.251950246861532,
134.685569347944));
#41911=CARTESIAN_POINT('Ctrl Pts',(6.76875222739921,-0.0789892825583523,
134.69369377262));
#41912=CARTESIAN_POINT('Ctrl Pts',(6.76856043284408,0.0943303891482489,
134.701818197295));
#41913=CARTESIAN_POINT('Ctrl Pts',(6.7617125052461,0.267456531792584,134.709942621971));
#41914=CARTESIAN_POINT('Ctrl Pts',(6.75482300634381,0.441633660951844,134.718116367105));
#41915=CARTESIAN_POINT('Ctrl Pts',(6.74119625329659,0.615614530761113,134.726290112239));
#41916=CARTESIAN_POINT('Ctrl Pts',(6.72086498424807,0.788836398442758,134.734463857373));
#41917=CARTESIAN_POINT('Ctrl Pts',(6.70066391069721,0.960949003971931,134.742585260235));
#41918=CARTESIAN_POINT('Ctrl Pts',(6.67384400370626,1.13231193478869,134.750706663097));
#41919=CARTESIAN_POINT('Ctrl Pts',(6.64048941823838,1.30237831917767,134.75882806596));
#41920=CARTESIAN_POINT('Ctrl Pts',(6.6071322539696,1.47245785220396,134.766950096726));
#41921=CARTESIAN_POINT('Ctrl Pts',(6.56723947525108,1.64124027997104,134.775072127492));
#41922=CARTESIAN_POINT('Ctrl Pts',(6.52094632601134,1.80818915306979,134.783194158258));
#41923=CARTESIAN_POINT('Ctrl Pts',(6.47464078234438,1.97518272469717,134.791318363599));
#41924=CARTESIAN_POINT('Ctrl Pts',(6.42193155378337,2.14034141163114,134.799442568941));
#41925=CARTESIAN_POINT('Ctrl Pts',(6.36300367972833,2.30314419256888,134.807566774282));
#41926=CARTESIAN_POINT('Ctrl Pts',(6.30343795221144,2.46770920095981,134.815778918524));
#41927=CARTESIAN_POINT('Ctrl Pts',(6.23751829741433,2.62986664224246,134.823991062767));
#41928=CARTESIAN_POINT('Ctrl Pts',(6.16548532028607,2.7891001712626,134.832203207009));
#41929=CARTESIAN_POINT('Ctrl Pts',(6.09410992484852,2.9468800736605,134.840340383426));
#41930=CARTESIAN_POINT('Ctrl Pts',(6.01673257818537,3.10178892693418,134.848477559842));
#41931=CARTESIAN_POINT('Ctrl Pts',(5.9336329117574,3.25335049887181,134.856614736258));
#41932=CARTESIAN_POINT('Ctrl Pts',(5.84938484918781,3.40700657650256,134.864864364414));
#41933=CARTESIAN_POINT('Ctrl Pts',(5.75925535132503,3.55722184325435,134.873113992569));
#41934=CARTESIAN_POINT('Ctrl Pts',(5.66358006671869,3.70353207463723,134.881363620725));
#41935=CARTESIAN_POINT('Ctrl Pts',(5.56790478211242,3.84984230602,134.88961324888));
#41936=CARTESIAN_POINT('Ctrl Pts',(5.46668398524656,3.99224722506152,134.897862877036));
#41937=CARTESIAN_POINT('Ctrl Pts',(5.36029402924288,4.13031922737978,134.906112505191));
#41938=CARTESIAN_POINT('Ctrl Pts',(5.2542144966466,4.26798836477511,134.914338062675));
#41939=CARTESIAN_POINT('Ctrl Pts',(5.14267895516024,4.40176148366843,134.922563620159));
#41940=CARTESIAN_POINT('Ctrl Pts',(5.0260033245659,4.53117860842546,134.930789177643));
#41941=CARTESIAN_POINT('Ctrl Pts',(4.90945576977456,4.66045367093616,134.939005705865));
#41942=CARTESIAN_POINT('Ctrl Pts',(4.78777959814272,4.7853819955667,134.947222234086));
#41943=CARTESIAN_POINT('Ctrl Pts',(4.66133283063708,4.90553414441536,134.955438762308));
#41944=CARTESIAN_POINT('Ctrl Pts',(4.53502820507165,5.02555122726039,134.963646054127));
#41945=CARTESIAN_POINT('Ctrl Pts',(4.40396392947557,5.14080258849623,134.971853345946));
#41946=CARTESIAN_POINT('Ctrl Pts',(4.26853673551919,5.25089355610292,134.980060637764));
#41947=CARTESIAN_POINT('Ctrl Pts',(4.1331977895448,5.3609127854904,134.988262581492));
#41948=CARTESIAN_POINT('Ctrl Pts',(3.99350186251409,5.46577809063417,134.99646452522));
#41949=CARTESIAN_POINT('Ctrl Pts',(3.84988120676472,5.56513285499995,135.004666468948));
#41950=CARTESIAN_POINT('Ctrl Pts',(3.70633385705389,5.66443690727178,135.012864226287));
#41951=CARTESIAN_POINT('Ctrl Pts',(3.55886606330543,5.75823581780362,135.021061983626));
#41952=CARTESIAN_POINT('Ctrl Pts',(3.40794169440871,5.8462143655113,135.029259740964));
#41953=CARTESIAN_POINT('Ctrl Pts',(3.3065303706811,5.90533020643143,135.034768098755));
#41954=CARTESIAN_POINT('Ctrl Pts',(3.20355908066341,5.96181902526415,135.040276456547));
#41955=CARTESIAN_POINT('Ctrl Pts',(3.09917575053244,6.01559628526647,135.045784814338));
#41956=CARTESIAN_POINT('Ctrl Pts',(3.09917575053245,6.01559628526646,133.045751582742));
#41957=CARTESIAN_POINT('Ctrl Pts',(2.93382384459245,6.10078395293769,133.054501030655));
#41958=CARTESIAN_POINT('Ctrl Pts',(2.76495772122957,6.17915010267061,133.063250478567));
#41959=CARTESIAN_POINT('Ctrl Pts',(2.59315093316678,6.25042856433191,133.07199992648));
#41960=CARTESIAN_POINT('Ctrl Pts',(2.42134553245588,6.32170645041462,133.08074930374));
#41961=CARTESIAN_POINT('Ctrl Pts',(2.24659977927565,6.38589665313466,133.089498681));
#41962=CARTESIAN_POINT('Ctrl Pts',(2.06950718689898,6.44278115439082,133.09824805826));
#41963=CARTESIAN_POINT('Ctrl Pts',(1.89241596572832,6.49966521519733,133.106997367774));
#41964=CARTESIAN_POINT('Ctrl Pts',(1.7129782145716,6.54924360009556,133.115746677289));
#41965=CARTESIAN_POINT('Ctrl Pts',(1.53180337335799,6.59134792173567,133.124495986804));
#41966=CARTESIAN_POINT('Ctrl Pts',(1.35062987477748,6.63345193135311,133.13324523148));
#41967=CARTESIAN_POINT('Ctrl Pts',(1.16771959102929,6.66808192368242,133.141994476156));
#41968=CARTESIAN_POINT('Ctrl Pts',(0.983693746906729,6.6951202836317,133.150743720832));
#41969=CARTESIAN_POINT('Ctrl Pts',(0.799669205419863,6.72215845218867,133.159492903576));
#41970=CARTESIAN_POINT('Ctrl Pts',(0.614529402873576,6.74160505424578,133.16824208632));
#41971=CARTESIAN_POINT('Ctrl Pts',(0.428903127363458,6.75339404354121,133.176991269065));
#41972=CARTESIAN_POINT('Ctrl Pts',(0.243278104164094,6.76518295330329,133.185740392783));
#41973=CARTESIAN_POINT('Ctrl Pts',(0.0571669005393355,6.76931433552276,
133.194489516502));
#41974=CARTESIAN_POINT('Ctrl Pts',(-0.12879840477729,6.76577415902473,133.20323864022));
#41975=CARTESIAN_POINT('Ctrl Pts',(-0.314762517258985,6.76223400523442,
133.21198770782));
#41976=CARTESIAN_POINT('Ctrl Pts',(-0.500580446819504,6.75102239665089,
133.220736775419));
#41977=CARTESIAN_POINT('Ctrl Pts',(-0.685621118842714,6.73217741012497,
133.229485843018));
#41978=CARTESIAN_POINT('Ctrl Pts',(-0.870660665414561,6.71333253821771,
133.238234857404));
#41979=CARTESIAN_POINT('Ctrl Pts',(-1.05492267885491,6.68685441030611,133.24698387179));
#41980=CARTESIAN_POINT('Ctrl Pts',(-1.23778137635253,6.65283295028177,133.255732886175));
#41981=CARTESIAN_POINT('Ctrl Pts',(-1.42999922978835,6.61707018861868,133.264929696543));
#41982=CARTESIAN_POINT('Ctrl Pts',(-1.6206660123367,6.57297172934419,133.27412650691));
#41983=CARTESIAN_POINT('Ctrl Pts',(-1.80906628500347,6.52070304311305,133.283323317278));
#41984=CARTESIAN_POINT('Ctrl Pts',(-1.98831342545479,6.47097374915045,133.292073315015));
#41985=CARTESIAN_POINT('Ctrl Pts',(-2.16550875896643,6.41384933989548,133.300823312753));
#41986=CARTESIAN_POINT('Ctrl Pts',(-2.34005036713943,6.34952386240501,133.309573310491));
#41987=CARTESIAN_POINT('Ctrl Pts',(-2.51458843547021,6.28519968948623,133.318323130772));
#41988=CARTESIAN_POINT('Ctrl Pts',(-2.68647261717989,6.21367483971128,133.327072951053));
#41989=CARTESIAN_POINT('Ctrl Pts',(-2.85511905908666,6.13519226743874,133.335822771333));
#41990=CARTESIAN_POINT('Ctrl Pts',(-3.02376230488826,6.05671118252966,133.344572425792));
#41991=CARTESIAN_POINT('Ctrl Pts',(-3.18916767379853,5.9712727599266,133.35332208025));
#41992=CARTESIAN_POINT('Ctrl Pts',(-3.35077334102743,5.87916720438021,133.362071734709));
#41993=CARTESIAN_POINT('Ctrl Pts',(-3.51237616037334,5.78706327195664,133.370821234977));
#41994=CARTESIAN_POINT('Ctrl Pts',(-3.67017916302276,5.68829258362314,133.379570735246));
#41995=CARTESIAN_POINT('Ctrl Pts',(-3.82364636566447,5.58319061741052,133.388320235514));
#41996=CARTESIAN_POINT('Ctrl Pts',(-3.9771110677879,5.47809036367708,133.397069593223));
#41997=CARTESIAN_POINT('Ctrl Pts',(-4.12623987481926,5.36665920043226,133.405818950931));
#41998=CARTESIAN_POINT('Ctrl Pts',(-4.27052628213935,5.2492755951233,133.41456830864));
#41999=CARTESIAN_POINT('Ctrl Pts',(-4.41481053024981,5.13189374643034,133.423317535416));
#42000=CARTESIAN_POINT('Ctrl Pts',(-4.5542523013653,5.00855981477353,133.432066762193));
#42001=CARTESIAN_POINT('Ctrl Pts',(-4.68837800630545,4.87969268192079,133.440815988969));
#42002=CARTESIAN_POINT('Ctrl Pts',(-4.8225018822888,4.75082730631824,133.44956509644));
#42003=CARTESIAN_POINT('Ctrl Pts',(-4.95130963052941,4.61642907903552,133.458314203911));
#42004=CARTESIAN_POINT('Ctrl Pts',(-5.07436379033332,4.47695444731729,133.467063311382));
#42005=CARTESIAN_POINT('Ctrl Pts',(-5.19741643562746,4.33748153220656,133.475812311171));
#42006=CARTESIAN_POINT('Ctrl Pts',(-5.31471544462691,4.19293255254692,133.484561310961));
#42007=CARTESIAN_POINT('Ctrl Pts',(-5.42586245275525,4.0437984177974,133.493310310751));
#42008=CARTESIAN_POINT('Ctrl Pts',(-5.53702160019049,3.89464799484491,133.502060266093));
#42009=CARTESIAN_POINT('Ctrl Pts',(-5.64202723081146,3.74091164444008,133.510810221435));
#42010=CARTESIAN_POINT('Ctrl Pts',(-5.74052265232861,3.58311159163402,133.519560176777));
#42011=CARTESIAN_POINT('Ctrl Pts',(-5.83901427066824,3.42531763191944,133.52830979426));
#42012=CARTESIAN_POINT('Ctrl Pts',(-5.93099603115656,3.26346052695765,133.537059411742));
#42013=CARTESIAN_POINT('Ctrl Pts',(-6.0161555062268,3.0980900446722,133.545809029225));
#42014=CARTESIAN_POINT('Ctrl Pts',(-6.10131214578732,2.93272506863969,133.554558355376));
#42015=CARTESIAN_POINT('Ctrl Pts',(-6.17964682328686,2.76384720417033,133.563307681527));
#42016=CARTESIAN_POINT('Ctrl Pts',(-6.25089348288508,2.59203002791729,133.572057007678));
#42017=CARTESIAN_POINT('Ctrl Pts',(-6.32213814889278,2.42021765937165,133.58080608901));
#42018=CARTESIAN_POINT('Ctrl Pts',(-6.38629508412537,2.24546640832054,133.589555170341));
#42019=CARTESIAN_POINT('Ctrl Pts',(-6.44314639819768,2.06836976660178,133.598304251673));
#42020=CARTESIAN_POINT('Ctrl Pts',(-6.50000285283659,1.89125711158416,133.607054124107));
#42021=CARTESIAN_POINT('Ctrl Pts',(-6.54955227673212,1.71179891440399,133.615803996542));
#42022=CARTESIAN_POINT('Ctrl Pts',(-6.59162635926351,1.53060476278579,133.624553868976));
#42023=CARTESIAN_POINT('Ctrl Pts',(-6.63369752055164,1.34942319164854,133.633303133898));
#42024=CARTESIAN_POINT('Ctrl Pts',(-6.66829431424224,1.16650618642873,133.642052398821));
#42025=CARTESIAN_POINT('Ctrl Pts',(-6.69529923745391,0.982474997620353,
133.650801663743));
#42026=CARTESIAN_POINT('Ctrl Pts',(-6.72230554731422,0.798434359179557,
133.659551377923));
#42027=CARTESIAN_POINT('Ctrl Pts',(-6.74171916496686,0.61327970624217,133.668301092103));
#42028=CARTESIAN_POINT('Ctrl Pts',(-6.75347414817263,0.427639953657228,
133.677050806282));
#42029=CARTESIAN_POINT('Ctrl Pts',(-6.76248837758727,0.285283364201958,
133.683760465458));
#42030=CARTESIAN_POINT('Ctrl Pts',(-6.76699999999983,0.142641701110043,
133.690470124634));
#42031=CARTESIAN_POINT('Ctrl Pts',(-6.767,8.02940689021197E-12,133.69717978381));
#42032=CARTESIAN_POINT('',(-6.76699974091591,0.00187255015161877,133.302820216163));
#42033=CARTESIAN_POINT('Ctrl Pts',(3.09917575053271,6.01559628526633,132.65155107452));
#42034=CARTESIAN_POINT('Ctrl Pts',(2.94514351274779,6.09495217178293,132.659674734604));
#42035=CARTESIAN_POINT('Ctrl Pts',(2.78800879566836,6.16841517401018,132.667798394687));
#42036=CARTESIAN_POINT('Ctrl Pts',(2.62826910112264,6.23574298156074,132.67592205477));
#42037=CARTESIAN_POINT('Ctrl Pts',(2.46854044018786,6.30306613861515,132.684045153733));
#42038=CARTESIAN_POINT('Ctrl Pts',(2.3062074966978,6.36425480178092,132.692168252695));
#42039=CARTESIAN_POINT('Ctrl Pts',(2.14178848258467,6.4191145102629,132.700291351658));
#42040=CARTESIAN_POINT('Ctrl Pts',(1.97734954609699,6.47398086600319,132.708415434882));
#42041=CARTESIAN_POINT('Ctrl Pts',(1.81082438261073,6.52251662403311,132.716539518107));
#42042=CARTESIAN_POINT('Ctrl Pts',(1.64274707558439,6.56457698908764,132.724663601331));
#42043=CARTESIAN_POINT('Ctrl Pts',(1.47461742592983,6.60665045257937,132.732790214558));
#42044=CARTESIAN_POINT('Ctrl Pts',(1.30493502492591,6.64224441901035,132.740916827784));
#42045=CARTESIAN_POINT('Ctrl Pts',(1.13424482946422,6.67126507244568,132.74904344101));
#42046=CARTESIAN_POINT('Ctrl Pts',(0.963371144075798,6.70031692273774,132.757178790249));
#42047=CARTESIAN_POINT('Ctrl Pts',(0.791487861200154,6.72278128436248,132.765314139487));
#42048=CARTESIAN_POINT('Ctrl Pts',(0.619146654162468,6.73861606122796,132.773449488726));
#42049=CARTESIAN_POINT('Ctrl Pts',(0.446707403851209,6.7544598463474,132.781589466087));
#42050=CARTESIAN_POINT('Ctrl Pts',(0.273810074801987,6.76366651217163,132.789729443449));
#42051=CARTESIAN_POINT('Ctrl Pts',(0.101006745760999,6.76624612597789,132.79786942081));
#42052=CARTESIAN_POINT('Ctrl Pts',(-0.072052076187581,6.76882955379071,
132.806021433278));
#42053=CARTESIAN_POINT('Ctrl Pts',(-0.245016255431909,6.76476636325331,
132.814173445746));
#42054=CARTESIAN_POINT('Ctrl Pts',(-0.417337295311639,6.75411863842663,
132.822325458214));
#42055=CARTESIAN_POINT('Ctrl Pts',(-0.553939800715431,6.7456779634563,132.828787729612));
#42056=CARTESIAN_POINT('Ctrl Pts',(-0.690138208722745,6.73310055831335,
132.83525000101));
#42057=CARTESIAN_POINT('Ctrl Pts',(-0.825664237599166,6.7164400962675,132.841712272407));
#42058=CARTESIAN_POINT('Ctrl Pts',(-0.998183374532949,6.6952320039409,132.849938481744));
#42059=CARTESIAN_POINT('Ctrl Pts',(-1.17012601879114,6.66734297938474,132.858164691081));
#42060=CARTESIAN_POINT('Ctrl Pts',(-1.34093539900288,6.63281096185479,132.866390900418));
#42061=CARTESIAN_POINT('Ctrl Pts',(-1.51155288219382,6.59831773956709,132.874607867961));
#42062=CARTESIAN_POINT('Ctrl Pts',(-1.68103928824092,6.55719645582258,132.882824835504));
#42063=CARTESIAN_POINT('Ctrl Pts',(-1.84884276455914,6.50953680625107,132.891041803048));
#42064=CARTESIAN_POINT('Ctrl Pts',(-2.01649140036118,6.46192113458098,132.899251188391));
#42065=CARTESIAN_POINT('Ctrl Pts',(-2.18245985631306,6.40777920993767,132.907460573734));
#42066=CARTESIAN_POINT('Ctrl Pts',(-2.34620618877694,6.34725180844,132.915669959078));
#42067=CARTESIAN_POINT('Ctrl Pts',(-2.50983427910421,6.2867681141153,132.923873416378));
#42068=CARTESIAN_POINT('Ctrl Pts',(-2.67124310701897,6.21990825107323,132.932076873679));
#42069=CARTESIAN_POINT('Ctrl Pts',(-2.82990553760095,6.14686291113243,132.940280330979));
#42070=CARTESIAN_POINT('Ctrl Pts',(-2.98848522445533,6.07385566492112,132.948479510111));
#42071=CARTESIAN_POINT('Ctrl Pts',(-3.14432104231472,5.99466951775266,132.956678689243));
#42072=CARTESIAN_POINT('Ctrl Pts',(-3.29690542633323,5.90954343497148,132.964877868375));
#42073=CARTESIAN_POINT('Ctrl Pts',(-3.44946106016427,5.82443339177951,132.973075502605));
#42074=CARTESIAN_POINT('Ctrl Pts',(-3.59876616457057,5.73338581144675,132.981273136835));
#42075=CARTESIAN_POINT('Ctrl Pts',(-3.74433713061009,5.63668594586701,132.989470771064));
#42076=CARTESIAN_POINT('Ctrl Pts',(-3.88989758917809,5.53999306018931,132.99766781358));
#42077=CARTESIAN_POINT('Ctrl Pts',(-4.0317241469153,5.43764889952437,133.005864856096));
#42078=CARTESIAN_POINT('Ctrl Pts',(-4.16936163849881,5.32998241342451,133.014061898611));
#42079=CARTESIAN_POINT('Ctrl Pts',(-4.30701421064042,5.22230413060646,133.022259839254));
#42080=CARTESIAN_POINT('Ctrl Pts',(-4.44047651962785,5.10930258158499,133.030457779897));
#42081=CARTESIAN_POINT('Ctrl Pts',(-4.56932595567727,4.99134744440557,133.03865572054));
#42082=CARTESIAN_POINT('Ctrl Pts',(-4.69821292765836,4.87335794498053,133.046856049375));
#42083=CARTESIAN_POINT('Ctrl Pts',(-4.82248408550876,4.75041222512862,133.055056378211));
#42084=CARTESIAN_POINT('Ctrl Pts',(-4.94175316984594,4.62291732657178,133.063256707047));
#42085=CARTESIAN_POINT('Ctrl Pts',(-5.06114653566438,4.49528957502179,133.071465580839));
#42086=CARTESIAN_POINT('Ctrl Pts',(-5.17552716924335,4.36310343651924,133.07967445463));
#42087=CARTESIAN_POINT('Ctrl Pts',(-5.28454802155997,4.2268003510725,133.087883328422));
#42088=CARTESIAN_POINT('Ctrl Pts',(-5.39362738416555,4.0904241132632,133.096096607825));
#42089=CARTESIAN_POINT('Ctrl Pts',(-5.49734101822078,3.94992681204619,133.104309887229));
#42090=CARTESIAN_POINT('Ctrl Pts',(-5.59538491806513,3.80577937073201,133.112523166632));
#42091=CARTESIAN_POINT('Ctrl Pts',(-5.69357222252262,3.66142109112916,133.120748459247));
#42092=CARTESIAN_POINT('Ctrl Pts',(-5.78607302992193,3.51340230612826,133.128973751863));
#42093=CARTESIAN_POINT('Ctrl Pts',(-5.87262841582157,3.36222017269617,133.137199044478));
#42094=CARTESIAN_POINT('Ctrl Pts',(-5.95090736495183,3.22549409367369,133.144637833591));
#42095=CARTESIAN_POINT('Ctrl Pts',(-6.02432405458796,3.08618118257169,133.152076622703));
#42096=CARTESIAN_POINT('Ctrl Pts',(-6.09272106997221,2.94466279283667,133.159515411815));
#42097=CARTESIAN_POINT('Ctrl Pts',(-6.17384614171449,2.77680913057368,133.168338491258));
#42098=CARTESIAN_POINT('Ctrl Pts',(-6.24811056664241,2.60543610680238,133.177161570701));
#42099=CARTESIAN_POINT('Ctrl Pts',(-6.3152199428182,2.43110799304172,133.185984650144));
#42100=CARTESIAN_POINT('Ctrl Pts',(-6.3822040503645,2.25710528602949,133.194791260129));
#42101=CARTESIAN_POINT('Ctrl Pts',(-6.44205964745616,2.08015874708851,133.203597870113));
#42102=CARTESIAN_POINT('Ctrl Pts',(-6.49453917221377,1.90085505512149,133.212404480098));
#42103=CARTESIAN_POINT('Ctrl Pts',(-6.5468758864848,1.7220392953073,133.221187124998));
#42104=CARTESIAN_POINT('Ctrl Pts',(-6.59187649572117,1.54087944384467,133.229969769898));
#42105=CARTESIAN_POINT('Ctrl Pts',(-6.62934246164935,1.35797920682642,133.238752414798));
#42106=CARTESIAN_POINT('Ctrl Pts',(-6.66674524472862,1.1753874139589,133.247520248589));
#42107=CARTESIAN_POINT('Ctrl Pts',(-6.69663866505402,0.991061356626386,
133.256288082379));
#42108=CARTESIAN_POINT('Ctrl Pts',(-6.71887386000849,0.805619670374654,
133.265055916169));
#42109=CARTESIAN_POINT('Ctrl Pts',(-6.74105530833422,0.620626231394264,
133.273802556464));
#42110=CARTESIAN_POINT('Ctrl Pts',(-6.75561542493228,0.434522816148734,
133.282549196759));
#42111=CARTESIAN_POINT('Ctrl Pts',(-6.76245635510104,0.24793758358425,133.291295837054));
#42112=CARTESIAN_POINT('Ctrl Pts',(-6.76546084101675,0.165990729941485,
133.295137296757));
#42113=CARTESIAN_POINT('Ctrl Pts',(-6.76697702831058,0.0839510964780675,
133.29897875646));
#42114=CARTESIAN_POINT('Ctrl Pts',(-6.76699974091591,0.0018725501516181,
133.302820216163));
#42115=CARTESIAN_POINT('Ctrl Pts',(-6.76699974091606,0.00187254958292456,
133.30282021619));
#42116=CARTESIAN_POINT('Ctrl Pts',(-6.76704976530886,-0.178905068379914,
133.311281013386));
#42117=CARTESIAN_POINT('Ctrl Pts',(-6.75985133561909,-0.35959956883799,
133.319741810583));
#42118=CARTESIAN_POINT('Ctrl Pts',(-6.74545066451291,-0.539614985542796,
133.328202607779));
#42119=CARTESIAN_POINT('Ctrl Pts',(-6.73103955054426,-0.719760943124762,
133.336669540449));
#42120=CARTESIAN_POINT('Ctrl Pts',(-6.70941580134513,-0.899226511591429,
133.345136473119));
#42121=CARTESIAN_POINT('Ctrl Pts',(-6.68067734035097,-1.07742251420748,
133.353603405789));
#42122=CARTESIAN_POINT('Ctrl Pts',(-6.6519146210961,-1.25576893284921,133.362077485434));
#42123=CARTESIAN_POINT('Ctrl Pts',(-6.61602526000546,-1.43284332815699,
133.370551565079));
#42124=CARTESIAN_POINT('Ctrl Pts',(-6.57315804405913,-1.60806788657095,
133.379025644724));
#42125=CARTESIAN_POINT('Ctrl Pts',(-6.53021695282447,-1.78359441852084,
133.387514328189));
#42126=CARTESIAN_POINT('Ctrl Pts',(-6.48027404540615,-1.95726442568419,
133.396003011653));
#42127=CARTESIAN_POINT('Ctrl Pts',(-6.42352818474407,-2.12851466046127,
133.404491695118));
#42128=CARTESIAN_POINT('Ctrl Pts',(-6.36673137777479,-2.29991864331735,
133.412987999703));
#42129=CARTESIAN_POINT('Ctrl Pts',(-6.30311954325868,-2.46889821573112,
133.421484304289));
#42130=CARTESIAN_POINT('Ctrl Pts',(-6.23293949359794,-2.6349106757435,133.429980608874));
#42131=CARTESIAN_POINT('Ctrl Pts',(-6.16262828771194,-2.80123338870822,
133.438492791808));
#42132=CARTESIAN_POINT('Ctrl Pts',(-6.08572446155392,-2.9645776087454,133.447004974741));
#42133=CARTESIAN_POINT('Ctrl Pts',(-6.0025214309379,-3.12442402230095,133.455517157674));
#42134=CARTESIAN_POINT('Ctrl Pts',(-5.93148826083242,-3.26089017504536,
133.462784288857));
#42135=CARTESIAN_POINT('Ctrl Pts',(-5.85586467189241,-3.39480726791467,
133.47005142004));
#42136=CARTESIAN_POINT('Ctrl Pts',(-5.77585773945136,-3.52586959112499,
133.477318551222));
#42137=CARTESIAN_POINT('Ctrl Pts',(-5.68610278694159,-3.67290050752998,
133.485471107435));
#42138=CARTESIAN_POINT('Ctrl Pts',(-5.59058952644183,-3.81673194255564,
133.493623663649));
#42139=CARTESIAN_POINT('Ctrl Pts',(-5.48957310309481,-3.95687706983399,
133.501776219862));
#42140=CARTESIAN_POINT('Ctrl Pts',(-5.38867370970947,-4.09685983560386,
133.509919331142));
#42141=CARTESIAN_POINT('Ctrl Pts',(-5.28228405618291,-4.23316450129326,
133.518062442423));
#42142=CARTESIAN_POINT('Ctrl Pts',(-5.17070470433181,-4.36532952485845,
133.526205553703));
#42143=CARTESIAN_POINT('Ctrl Pts',(-5.05923116168047,-4.49736921810807,
133.53434094298));
#42144=CARTESIAN_POINT('Ctrl Pts',(-4.94257795262434,-4.62527680712845,
133.542476332258));
#42145=CARTESIAN_POINT('Ctrl Pts',(-4.82108838239013,-4.74862041114921,
133.550611721535));
#42146=CARTESIAN_POINT('Ctrl Pts',(-4.69968849119311,-4.8718729675547,133.558741105574));
#42147=CARTESIAN_POINT('Ctrl Pts',(-4.57345960279974,-4.99056798781283,
133.566870489612));
#42148=CARTESIAN_POINT('Ctrl Pts',(-4.44278466535951,-5.10430733961489,
133.574999873651));
#42149=CARTESIAN_POINT('Ctrl Pts',(-4.31217873926266,-5.21798662400374,
133.583124964443));
#42150=CARTESIAN_POINT('Ctrl Pts',(-4.17713171543183,-5.32671521265316,
133.591250055235));
#42151=CARTESIAN_POINT('Ctrl Pts',(-4.03806268885521,-5.43013247728593,
133.599375146027));
#42152=CARTESIAN_POINT('Ctrl Pts',(-3.89846280565517,-5.53394450803778,
133.607531252052));
#42153=CARTESIAN_POINT('Ctrl Pts',(-3.75481042015292,-5.63240432611419,
133.615687358077));
#42154=CARTESIAN_POINT('Ctrl Pts',(-3.60756260607739,-5.72518829762237,
133.623843464102));
#42155=CARTESIAN_POINT('Ctrl Pts',(-3.46090743782367,-5.81759883042525,
133.631966743276));
#42156=CARTESIAN_POINT('Ctrl Pts',(-3.31068605227303,-5.9043789422125,133.640090022449));
#42157=CARTESIAN_POINT('Ctrl Pts',(-3.15737835205038,-5.98525278847967,
133.648213301623));
#42158=CARTESIAN_POINT('Ctrl Pts',(-3.00405023761226,-6.06613740378271,
133.656337662479));
#42159=CARTESIAN_POINT('Ctrl Pts',(-2.84763531352529,-6.14111401635927,
133.664462023336));
#42160=CARTESIAN_POINT('Ctrl Pts',(-2.68863718791606,-6.20995322621313,
133.672586384193));
#42161=CARTESIAN_POINT('Ctrl Pts',(-2.52958764015158,-6.27881469960325,
133.680713372578));
#42162=CARTESIAN_POINT('Ctrl Pts',(-2.36795356277147,-6.34153467239499,
133.688840360963));
#42163=CARTESIAN_POINT('Ctrl Pts',(-2.20425754950671,-6.39793229531563,
133.696967349349));
#42164=CARTESIAN_POINT('Ctrl Pts',(-2.03950326015197,-6.45469452244793,
133.705146877789));
#42165=CARTESIAN_POINT('Ctrl Pts',(-1.87266063744718,-6.50505224733347,
133.713326406229));
#42166=CARTESIAN_POINT('Ctrl Pts',(-1.70427601599646,-6.54887259467607,
133.721505934669));
#42167=CARTESIAN_POINT('Ctrl Pts',(-1.53668437201362,-6.5924865778758,133.729646943073));
#42168=CARTESIAN_POINT('Ctrl Pts',(-1.36756559221563,-6.62962460870949,
133.737787951476));
#42169=CARTESIAN_POINT('Ctrl Pts',(-1.19746623968315,-6.66020747460761,
133.74592895988));
#42170=CARTESIAN_POINT('Ctrl Pts',(-1.02615962271941,-6.69100739956948,
133.754127748338));
#42171=CARTESIAN_POINT('Ctrl Pts',(-0.853858836676677,-6.71515871580873,
133.762326536797));
#42172=CARTESIAN_POINT('Ctrl Pts',(-0.681124613291064,-6.7326338279435,
133.770525325255));
#42173=CARTESIAN_POINT('Ctrl Pts',(-0.508390389905324,-6.75010894007828,
133.778724113713));
#42174=CARTESIAN_POINT('Ctrl Pts',(-0.335223103855506,-6.7609078896523,
133.786922902172));
#42175=CARTESIAN_POINT('Ctrl Pts',(-0.16218029837062,-6.76505628585753,
133.79512169063));
#42176=CARTESIAN_POINT('Ctrl Pts',(0.0115856305573594,-6.76922201767252,
133.803354740762));
#42177=CARTESIAN_POINT('Ctrl Pts',(0.185766191311162,-6.76669456557975,
133.811587790894));
#42178=CARTESIAN_POINT('Ctrl Pts',(0.359805115405753,-6.75742771170568,
133.819820841026));
#42179=CARTESIAN_POINT('Ctrl Pts',(0.533636785894009,-6.74817189323013,
133.828044086861));
#42180=CARTESIAN_POINT('Ctrl Pts',(0.707326801414873,-6.73219267276864,
133.836267332696));
#42181=CARTESIAN_POINT('Ctrl Pts',(0.880315921941427,-6.70949572453671,
133.844490578531));
#42182=CARTESIAN_POINT('Ctrl Pts',(1.05313366316287,-6.68682126203801,133.852705677644));
#42183=CARTESIAN_POINT('Ctrl Pts',(1.22525153954443,-6.65744237198378,133.860920776758));
#42184=CARTESIAN_POINT('Ctrl Pts',(1.39611236930303,-6.62141671036336,133.869135875871));
#42185=CARTESIAN_POINT('Ctrl Pts',(1.56683811405107,-6.58541953114518,133.87734448001));
#42186=CARTESIAN_POINT('Ctrl Pts',(1.73630844280544,-6.54278612089831,133.885553084149));
#42187=CARTESIAN_POINT('Ctrl Pts',(1.90397324675609,-6.49362571108292,133.893761688288));
#42188=CARTESIAN_POINT('Ctrl Pts',(2.07153903015424,-6.44449433473683,133.901965444537));
#42189=CARTESIAN_POINT('Ctrl Pts',(2.23730107020929,-6.38884373853091,133.910169200786));
#42190=CARTESIAN_POINT('Ctrl Pts',(2.40072128168432,-6.32683383120404,133.918372957035));
#42191=CARTESIAN_POINT('Ctrl Pts',(2.56409314123769,-6.26484227104583,133.926574285999));
#42192=CARTESIAN_POINT('Ctrl Pts',(2.72512421659101,-6.19649527106696,133.934775614963));
#42193=CARTESIAN_POINT('Ctrl Pts',(2.88329313691535,-6.12200209789386,133.942976943928));
#42194=CARTESIAN_POINT('Ctrl Pts',(3.04144024423566,-6.04751919804047,133.95117714185));
#42195=CARTESIAN_POINT('Ctrl Pts',(3.19672565830619,-5.96689196502827,133.959377339773));
#42196=CARTESIAN_POINT('Ctrl Pts',(3.34864947854664,-5.88037717071187,133.967577537696));
#42197=CARTESIAN_POINT('Ctrl Pts',(3.50057987872931,-5.7938586293705,133.975778090776));
#42198=CARTESIAN_POINT('Ctrl Pts',(3.64914808363584,-5.70145219596756,133.983978643855));
#42199=CARTESIAN_POINT('Ctrl Pts',(3.79388017451233,-5.60345984383241,133.992179196935));
#42200=CARTESIAN_POINT('Ctrl Pts',(3.93864476214154,-5.50544548943627,134.000381591288));
#42201=CARTESIAN_POINT('Ctrl Pts',(4.07957122360723,-5.40184291910736,134.008583985642));
#42202=CARTESIAN_POINT('Ctrl Pts',(4.21621588135013,-5.29299656544862,134.016786379995));
#42203=CARTESIAN_POINT('Ctrl Pts',(4.35298832586857,-5.1840484213153,134.024996445029));
#42204=CARTESIAN_POINT('Ctrl Pts',(4.48547068592351,-5.06984691987039,134.033206510063));
#42205=CARTESIAN_POINT('Ctrl Pts',(4.61325284863728,-4.95077641936495,134.041416575096));
#42206=CARTESIAN_POINT('Ctrl Pts',(4.74109616562688,-4.83164893383064,134.049630569322));
#42207=CARTESIAN_POINT('Ctrl Pts',(4.86423454795761,-4.70764805725219,134.057844563547));
#42208=CARTESIAN_POINT('Ctrl Pts',(4.98229591798076,-4.57919385762082,134.066058557772));
#42209=CARTESIAN_POINT('Ctrl Pts',(5.10051824497317,-4.45056453213196,134.074283750407));
#42210=CARTESIAN_POINT('Ctrl Pts',(5.21364949452321,-4.31747002295741,134.082508943043));
#42211=CARTESIAN_POINT('Ctrl Pts',(5.32135817489546,-4.18036316298875,134.090734135678));
#42212=CARTESIAN_POINT('Ctrl Pts',(5.41822036046025,-4.05706325747888,134.098131033798));
#42213=CARTESIAN_POINT('Ctrl Pts',(5.51069757661604,-3.93051897913587,134.105527931918));
#42214=CARTESIAN_POINT('Ctrl Pts',(5.59857970815348,-3.80107803806395,134.112924830037));
#42215=CARTESIAN_POINT('Ctrl Pts',(5.70130195092437,-3.64977920699706,134.121570796528));
#42216=CARTESIAN_POINT('Ctrl Pts',(5.79797894980601,-3.49417916443688,134.130216763019));
#42217=CARTESIAN_POINT('Ctrl Pts',(5.88825544569583,-3.33477687502978,134.13886272951));
#42218=CARTESIAN_POINT('Ctrl Pts',(5.97841646567461,-3.17557848282107,134.147497636634));
#42219=CARTESIAN_POINT('Ctrl Pts',(6.06219315868862,-3.01258780613254,134.156132543759));
#42220=CARTESIAN_POINT('Ctrl Pts',(6.13927355357156,-2.84633259378043,134.164767450883));
#42221=CARTESIAN_POINT('Ctrl Pts',(6.21891295535231,-2.67455784256438,134.173689029955));
#42222=CARTESIAN_POINT('Ctrl Pts',(6.29140359053872,-2.49929831964581,134.182610609026));
#42223=CARTESIAN_POINT('Ctrl Pts',(6.35645150764813,-2.32116635140997,134.191532188098));
#42224=CARTESIAN_POINT('Ctrl Pts',(6.41923539892832,-2.14923435690143,134.200143247074));
#42225=CARTESIAN_POINT('Ctrl Pts',(6.47508577903036,-1.97462681126812,134.208754306049));
#42226=CARTESIAN_POINT('Ctrl Pts',(6.52378584774984,-1.7979174654858,134.217365365025));
#42227=CARTESIAN_POINT('Ctrl Pts',(6.57243999005592,-1.62137476477566,134.225968303375));
#42228=CARTESIAN_POINT('Ctrl Pts',(6.61395718414473,-1.44273450872252,134.234571241724));
#42229=CARTESIAN_POINT('Ctrl Pts',(6.64816983304999,-1.2625873716001,134.243174180074));
#42230=CARTESIAN_POINT('Ctrl Pts',(6.68234417170306,-1.08264195759693,134.251767485122));
#42231=CARTESIAN_POINT('Ctrl Pts',(6.70923022607123,-0.901193327721689,
134.260360790171));
#42232=CARTESIAN_POINT('Ctrl Pts',(6.72871100294165,-0.718844377380814,
134.26895409522));
#42233=CARTESIAN_POINT('Ctrl Pts',(6.7308814803534,-0.698527719559418,134.269911530061));
#42234=CARTESIAN_POINT('Ctrl Pts',(6.73296008349514,-0.67819989735964,134.270868964901));
#42235=CARTESIAN_POINT('Ctrl Pts',(6.73494668975532,-0.657861753071142,
134.271826399742));
#42236=CARTESIAN_POINT('Ctrl Pts',(6.7527822489269,-0.475267857557712,134.28042215729));
#42237=CARTESIAN_POINT('Ctrl Pts',(6.76317747172217,-0.292055383205121,
134.289017914837));
#42238=CARTESIAN_POINT('Ctrl Pts',(6.76612466864008,-0.108839186050769,
134.297613672385));
#42239=CARTESIAN_POINT('Ctrl Pts',(6.76907461539293,0.0745479580457943,
134.306217450066));
#42240=CARTESIAN_POINT('Ctrl Pts',(6.76456266037914,0.257938526612442,134.314821227748));
#42241=CARTESIAN_POINT('Ctrl Pts',(6.75263320084626,0.440719700976544,134.32342500543));
#42242=CARTESIAN_POINT('Ctrl Pts',(6.74023490312219,0.63068433532344,134.332366919098));
#42243=CARTESIAN_POINT('Ctrl Pts',(6.7198243193483,0.819990332411676,134.341308832766));
#42244=CARTESIAN_POINT('Ctrl Pts',(6.6915100729088,1.00795929687667,134.350250746434));
#42245=CARTESIAN_POINT('Ctrl Pts',(6.66419234854404,1.18931267922269,134.358877948764));
#42246=CARTESIAN_POINT('Ctrl Pts',(6.6295179237513,1.36942125684008,134.367505151095));
#42247=CARTESIAN_POINT('Ctrl Pts',(6.58763598010825,1.54768898477156,134.376132353426));
#42248=CARTESIAN_POINT('Ctrl Pts',(6.54571415032432,1.72612648542832,134.384767771846));
#42249=CARTESIAN_POINT('Ctrl Pts',(6.49657117916455,1.90271934256209,134.393403190267));
#42250=CARTESIAN_POINT('Ctrl Pts',(6.44040592710666,2.0768872126549,134.402038608687));
#42251=CARTESIAN_POINT('Ctrl Pts',(6.38415769888914,2.25131239096695,134.410686784708));
#42252=CARTESIAN_POINT('Ctrl Pts',(6.32086655941959,2.4233051354262,134.41933496073));
#42253=CARTESIAN_POINT('Ctrl Pts',(6.25077978429076,2.59230420442933,134.427983136751));
#42254=CARTESIAN_POINT('Ctrl Pts',(6.24336486923098,2.6101836651341,134.428898080982));
#42255=CARTESIAN_POINT('Ctrl Pts',(6.23587393435357,2.62802964033025,134.429813025214));
#42256=CARTESIAN_POINT('Ctrl Pts',(6.22830730251598,2.64584148153779,134.430727969446));
#42257=CARTESIAN_POINT('Ctrl Pts',(6.16026405941084,2.80601518463973,134.438955642487));
#42258=CARTESIAN_POINT('Ctrl Pts',(6.08594872974335,2.96377266448755,134.447183315528));
#42259=CARTESIAN_POINT('Ctrl Pts',(6.00555492202109,3.11858927699501,134.455410988569));
#42260=CARTESIAN_POINT('Ctrl Pts',(5.92527093089928,3.27319441259199,134.463627422746));
#42261=CARTESIAN_POINT('Ctrl Pts',(5.83892517462812,3.42486637195514,134.471843856923));
#42262=CARTESIAN_POINT('Ctrl Pts',(5.74675932745894,3.57310036694517,134.480060291099));
#42263=CARTESIAN_POINT('Ctrl Pts',(5.65466644834513,3.72121700451175,134.488270220294));
#42264=CARTESIAN_POINT('Ctrl Pts',(5.55676284076521,3.86590079466694,134.496480149488));
#42265=CARTESIAN_POINT('Ctrl Pts',(5.45333641300495,4.00667080836377,134.504690078683));
#42266=CARTESIAN_POINT('Ctrl Pts',(5.34997312202254,4.14735488884917,134.512894996117));
#42267=CARTESIAN_POINT('Ctrl Pts',(5.24109393611688,4.2841296630918,134.52109991355));
#42268=CARTESIAN_POINT('Ctrl Pts',(5.12703049513253,4.41654246011302,134.529304830984));
#42269=CARTESIAN_POINT('Ctrl Pts',(5.01301601183697,4.54889842363479,134.537506226748));
#42270=CARTESIAN_POINT('Ctrl Pts',(4.89382193916935,4.67689586840449,134.545707622512));
#42271=CARTESIAN_POINT('Ctrl Pts',(4.76982071906617,4.80011450988069,134.553909018276));
#42272=CARTESIAN_POINT('Ctrl Pts',(4.64582916844672,4.92332354289779,134.562109774504));
#42273=CARTESIAN_POINT('Ctrl Pts',(4.51703146484481,5.04175425634369,134.570310530732));
#42274=CARTESIAN_POINT('Ctrl Pts',(4.38383773760777,5.15502237534679,134.57851128696));
#42275=CARTESIAN_POINT('Ctrl Pts',(4.25065495043721,5.2682811909031,134.586711369606));
#42276=CARTESIAN_POINT('Ctrl Pts',(4.11307713424406,5.3763780274387,134.594911452253));
#42277=CARTESIAN_POINT('Ctrl Pts',(3.97154820464094,5.47896832060684,134.603111534899));
#42278=CARTESIAN_POINT('Ctrl Pts',(3.82995342251291,5.58160634839613,134.611315432993));
#42279=CARTESIAN_POINT('Ctrl Pts',(3.6844041436477,5.67873250239356,134.619519331086));
#42280=CARTESIAN_POINT('Ctrl Pts',(3.53537457188812,5.77004468236138,134.62772322918));
#42281=CARTESIAN_POINT('Ctrl Pts',(3.39300572892145,5.85727575507597,134.635560462191));
#42282=CARTESIAN_POINT('Ctrl Pts',(3.24746117470512,5.93920110032378,134.643397695202));
#42283=CARTESIAN_POINT('Ctrl Pts',(3.09917575053266,6.01559628526635,134.651234928213));
#42284=CARTESIAN_POINT('Origin',(0.,0.,-3.69717978381041));
#42285=CARTESIAN_POINT('',(3.09917575053248,6.01559628526645,137.045751582742));
#42286=CARTESIAN_POINT('',(3.0991757505325,6.01559628526643,136.651412426306));
#42287=CARTESIAN_POINT('',(3.09917575053259,6.01559628526639,-3.69717978381041));
#42288=CARTESIAN_POINT('',(-6.76699999982859,-4.81653644018645E-5,135.697182049439));
#42289=CARTESIAN_POINT('Ctrl Pts',(-6.76699999982859,-4.81653644018645E-5,
135.697182049439));
#42290=CARTESIAN_POINT('Ctrl Pts',(-6.76699867588785,-0.186055414706891,
135.705931561242));
#42291=CARTESIAN_POINT('Ctrl Pts',(-6.75932372490837,-0.372062466127105,
135.714681073045));
#42292=CARTESIAN_POINT('Ctrl Pts',(-6.74400121519305,-0.55743753863076,
135.723430584848));
#42293=CARTESIAN_POINT('Ctrl Pts',(-6.72867877019546,-0.742811828165125,
135.732180059695));
#42294=CARTESIAN_POINT('Ctrl Pts',(-6.70570885470968,-0.927553858495178,
135.740929534542));
#42295=CARTESIAN_POINT('Ctrl Pts',(-6.67516948638864,-1.11103615062068,
135.74967900939));
#42296=CARTESIAN_POINT('Ctrl Pts',(-6.64463024452037,-1.29451768301062,
135.758428448009));
#42297=CARTESIAN_POINT('Ctrl Pts',(-6.60652165959189,-1.47673920492593,
135.767177886628));
#42298=CARTESIAN_POINT('Ctrl Pts',(-6.56097316689686,-1.65708180343017,
135.775927325246));
#42299=CARTESIAN_POINT('Ctrl Pts',(-6.51542485901923,-1.83742367017695,
135.784676728364));
#42300=CARTESIAN_POINT('Ctrl Pts',(-6.46243677396501,-2.01588635090299,
135.793426131481));
#42301=CARTESIAN_POINT('Ctrl Pts',(-6.40218888358992,-2.19186370443913,
135.802175534598));
#42302=CARTESIAN_POINT('Ctrl Pts',(-6.34194123267288,-2.3678403585451,135.81092490294));
#42303=CARTESIAN_POINT('Ctrl Pts',(-6.27443392700289,-2.54133143409247,
135.819674271283));
#42304=CARTESIAN_POINT('Ctrl Pts',(-6.19989625055173,-2.71174768044421,
135.828423639625));
#42305=CARTESIAN_POINT('Ctrl Pts',(-6.12535886416388,-2.8821632636213,135.837172973919));
#42306=CARTESIAN_POINT('Ctrl Pts',(-6.04379127658468,-3.04950377898405,
135.845922308213));
#42307=CARTESIAN_POINT('Ctrl Pts',(-5.95547052442305,-3.21320087027379,
135.854671642507));
#42308=CARTESIAN_POINT('Ctrl Pts',(-5.86715010862682,-3.3768973381309,135.86342094348));
#42309=CARTESIAN_POINT('Ctrl Pts',(-5.77207671579077,-3.53695015747485,
135.872170244453));
#42310=CARTESIAN_POINT('Ctrl Pts',(-5.67057325125895,-3.69281572815468,
135.880919545426));
#42311=CARTESIAN_POINT('Ctrl Pts',(-5.56907016486904,-3.84868071817152,
135.889668813803));
#42312=CARTESIAN_POINT('Ctrl Pts',(-5.46113721110327,-4.00035825060242,
135.898418082181));
#42313=CARTESIAN_POINT('Ctrl Pts',(-5.34714096852922,-4.1473331747855,135.907167350559));
#42314=CARTESIAN_POINT('Ctrl Pts',(-5.2331451411717,-4.29430756363148,135.915916587069));
#42315=CARTESIAN_POINT('Ctrl Pts',(-5.11308624482862,-4.4365791520693,135.924665823579));
#42316=CARTESIAN_POINT('Ctrl Pts',(-4.98737203909913,-4.57366473887322,
135.933415060089));
#42317=CARTESIAN_POINT('Ctrl Pts',(-4.86165828082827,-4.71074983774398,
135.942164265458));
#42318=CARTESIAN_POINT('Ctrl Pts',(-4.7302894471308,-4.84264876072114,135.950913470826));
#42319=CARTESIAN_POINT('Ctrl Pts',(-4.59371170670946,-4.96891353875679,
135.959662676195));
#42320=CARTESIAN_POINT('Ctrl Pts',(-4.45713444107297,-5.09517787785851,
135.968411851148));
#42321=CARTESIAN_POINT('Ctrl Pts',(-4.31534851536104,-5.21580791668835,
135.977161026102));
#42322=CARTESIAN_POINT('Ctrl Pts',(-4.16883547455953,-5.33039396161804,
135.985910201056));
#42323=CARTESIAN_POINT('Ctrl Pts',(-4.02232293091532,-5.44497961772713,
135.994659346321));
#42324=CARTESIAN_POINT('Ctrl Pts',(-3.87108352999623,-5.55352114444728,
136.003408491586));
#42325=CARTESIAN_POINT('Ctrl Pts',(-3.71563091997335,-5.65564990664539,
136.012157636852));
#42326=CARTESIAN_POINT('Ctrl Pts',(-3.56017882453426,-5.75777833077388,
136.020906753155));
#42327=CARTESIAN_POINT('Ctrl Pts',(-3.40051378738538,-5.85349387552368,
136.029655869459));
#42328=CARTESIAN_POINT('Ctrl Pts',(-3.23717806875404,-5.94247146826789,
136.038404985763));
#42329=CARTESIAN_POINT('Ctrl Pts',(-3.07384287723976,-6.03144877386358,
136.047154073831));
#42330=CARTESIAN_POINT('Ctrl Pts',(-2.9068372795745,-6.11368803389362,136.0559031619));
#42331=CARTESIAN_POINT('Ctrl Pts',(-2.73672846260799,-6.18890994618207,
136.064652249968));
#42332=CARTESIAN_POINT('Ctrl Pts',(-2.56662018049375,-6.26413162195949,
136.073401310528));
#42333=CARTESIAN_POINT('Ctrl Pts',(-2.39340896066045,-6.33233587826648,
136.082150371088));
#42334=CARTESIAN_POINT('Ctrl Pts',(-2.21768306188705,-6.39329108026682,
136.090899431648));
#42335=CARTESIAN_POINT('Ctrl Pts',(-2.04195770103624,-6.4542460956744,136.099648465426));
#42336=CARTESIAN_POINT('Ctrl Pts',(-1.86371794735658,-6.50795200727928,
136.108397499203));
#42337=CARTESIAN_POINT('Ctrl Pts',(-1.68356913379756,-6.55422642054149,
136.117146532981));
#42338=CARTESIAN_POINT('Ctrl Pts',(-1.50342085674391,-6.6005006959928,136.125895540703));
#42339=CARTESIAN_POINT('Ctrl Pts',(-1.32136380870533,-6.63934344610502,
136.134644548425));
#42340=CARTESIAN_POINT('Ctrl Pts',(-1.13801628314245,-6.67062275498343,
136.143393556147));
#42341=CARTESIAN_POINT('Ctrl Pts',(-0.95466928838962,-6.701901973305,136.15214253854));
#42342=CARTESIAN_POINT('Ctrl Pts',(-0.770032106030325,-6.72561774602647,
136.160891520933));
#42343=CARTESIAN_POINT('Ctrl Pts',(-0.584731788427198,-6.7416895312379,
136.169640503325));
#42344=CARTESIAN_POINT('Ctrl Pts',(-0.391443045919639,-6.75845418223015,
136.178766660403));
#42345=CARTESIAN_POINT('Ctrl Pts',(-0.197433054891392,-6.76690112092229,
136.18789281748));
#42346=CARTESIAN_POINT('Ctrl Pts',(-0.00341866909486969,-6.76699913644901,
136.197018974557));
#42347=CARTESIAN_POINT('Ctrl Pts',(0.1845327671456,-6.76709408899052,136.205859939226));
#42348=CARTESIAN_POINT('Ctrl Pts',(0.372488010641898,-6.75935406923834,
136.214700903894));
#42349=CARTESIAN_POINT('Ctrl Pts',(0.559795261984329,-6.74380591837131,
136.223541868563));
#42350=CARTESIAN_POINT('Ctrl Pts',(0.745174855785072,-6.72841778005085,
136.232291847153));
#42351=CARTESIAN_POINT('Ctrl Pts',(0.929919443623088,-6.70538151166438,
136.241041825744));
#42352=CARTESIAN_POINT('Ctrl Pts',(1.11340146562901,-6.67477536523404,136.249791804334));
#42353=CARTESIAN_POINT('Ctrl Pts',(1.29688160934916,-6.64416953211554,136.258541693352));
#42354=CARTESIAN_POINT('Ctrl Pts',(1.47909893033434,-6.60599402319168,136.26729158237));
#42355=CARTESIAN_POINT('Ctrl Pts',(1.65943446626114,-6.56037851439874,136.276041471387));
#42356=CARTESIAN_POINT('Ctrl Pts',(1.8397682160447,-6.51476345740711,136.284791273742));
#42357=CARTESIAN_POINT('Ctrl Pts',(2.01821994016055,-6.46170861830474,136.293541076096));
#42358=CARTESIAN_POINT('Ctrl Pts',(2.19418347939502,-6.40139421210333,136.30229087845));
#42359=CARTESIAN_POINT('Ctrl Pts',(2.37014533426395,-6.34108038324599,136.311040597048));
#42360=CARTESIAN_POINT('Ctrl Pts',(2.54361878075444,-6.27350721929238,136.319790315647));
#42361=CARTESIAN_POINT('Ctrl Pts',(2.71401458097926,-6.19890424625449,136.328540034246));
#42362=CARTESIAN_POINT('Ctrl Pts',(2.88440880675507,-6.12430196254449,136.337289671998));
#42363=CARTESIAN_POINT('Ctrl Pts',(3.05172518060253,-6.04267011469176,136.34603930975));
#42364=CARTESIAN_POINT('Ctrl Pts',(3.21539538887731,-5.95428597677224,136.354788947502));
#42365=CARTESIAN_POINT('Ctrl Pts',(3.37906413922919,-5.86590262615091,136.363538507314));
#42366=CARTESIAN_POINT('Ctrl Pts',(3.53908653680616,-5.77076724201437,136.372288067127));
#42367=CARTESIAN_POINT('Ctrl Pts',(3.69491905265573,-5.66920295935167,136.38103762694));
#42368=CARTESIAN_POINT('Ctrl Pts',(3.85075023217284,-5.56763954764742,136.389787111722));
#42369=CARTESIAN_POINT('Ctrl Pts',(4.00239136175179,-5.45964750423334,136.398536596503));
#42370=CARTESIAN_POINT('Ctrl Pts',(4.14932738891612,-5.34559362649188,136.407286081285));
#42371=CARTESIAN_POINT('Ctrl Pts',(4.29626220485472,-5.2315406889214,136.416035493942));
#42372=CARTESIAN_POINT('Ctrl Pts',(4.43849176959685,-5.11142619274938,136.4247849066));
#42373=CARTESIAN_POINT('Ctrl Pts',(4.57553300521195,-4.98565810282014,136.433534319257));
#42374=CARTESIAN_POINT('Ctrl Pts',(4.71257315669189,-4.85989100784405,136.442283662698));
#42375=CARTESIAN_POINT('Ctrl Pts',(4.84442485003742,-4.72847060238681,136.451033006139));
#42376=CARTESIAN_POINT('Ctrl Pts',(4.97064026248733,-4.591843244378,136.45978234958));
#42377=CARTESIAN_POINT('Ctrl Pts',(5.0968547183719,-4.45521692184491,136.468531626711));
#42378=CARTESIAN_POINT('Ctrl Pts',(5.21743278438389,-4.31338393622911,136.477280903842));
#42379=CARTESIAN_POINT('Ctrl Pts',(5.33196493385394,-4.16682600358497,136.486030180973));
#42380=CARTESIAN_POINT('Ctrl Pts',(5.44649625334771,-4.02026913299729,136.494779394701));
#42381=CARTESIAN_POINT('Ctrl Pts',(5.55498156752181,-3.86898760969255,136.503528608429));
#42382=CARTESIAN_POINT('Ctrl Pts',(5.65705242639514,-3.71349523293311,136.512277822157));
#42383=CARTESIAN_POINT('Ctrl Pts',(5.75912257949751,-3.55800393132876,136.521026975388));
#42384=CARTESIAN_POINT('Ctrl Pts',(5.85477820880497,-3.39830207408514,136.529776128619));
#42385=CARTESIAN_POINT('Ctrl Pts',(5.94369444243805,-3.23493205105318,136.538525281851));
#42386=CARTESIAN_POINT('Ctrl Pts',(6.03261009078973,-3.07156310338652,136.547274377492));
#42387=CARTESIAN_POINT('Ctrl Pts',(6.11478629525939,-2.90452628992948,136.556023473133));
#42388=CARTESIAN_POINT('Ctrl Pts',(6.18994396733866,-2.73438890452834,136.564772568774));
#42389=CARTESIAN_POINT('Ctrl Pts',(6.26510116966157,-2.56425258253322,136.57352160973));
#42390=CARTESIAN_POINT('Ctrl Pts',(6.33323981159752,-2.39101598947377,136.582270650687));
#42391=CARTESIAN_POINT('Ctrl Pts',(6.39412848218535,-2.21526746766753,136.591019691644));
#42392=CARTESIAN_POINT('Ctrl Pts',(6.4550167924232,-2.03951998597227,136.599768680822));
#42393=CARTESIAN_POINT('Ctrl Pts',(6.5086551233768,-1.86126087601571,136.608517670001));
#42394=CARTESIAN_POINT('Ctrl Pts',(6.55486131187705,-1.68109553031869,136.617266659179));
#42395=CARTESIAN_POINT('Ctrl Pts',(6.60200641330949,-1.49726921239052,136.62619342842));
#42396=CARTESIAN_POINT('Ctrl Pts',(6.64141400419643,-1.31145865379569,136.635120197661));
#42397=CARTESIAN_POINT('Ctrl Pts',(6.67294476247483,-1.12432077138144,136.644046966902));
#42398=CARTESIAN_POINT('Ctrl Pts',(6.70385084062283,-0.94089042164866,136.652796881044));
#42399=CARTESIAN_POINT('Ctrl Pts',(6.72718922812515,-0.756185141262743,
136.661546795186));
#42400=CARTESIAN_POINT('Ctrl Pts',(6.74288064785628,-0.570832347336133,
136.670296709328));
#42401=CARTESIAN_POINT('Ctrl Pts',(6.75857175900919,-0.385483198448501,
136.679046451399));
#42402=CARTESIAN_POINT('Ctrl Pts',(6.76661617913882,-0.199486847133674,
136.68779619347));
#42403=CARTESIAN_POINT('Ctrl Pts',(6.76698658358759,-0.0134750712614812,
136.696545935542));
#42404=CARTESIAN_POINT('Ctrl Pts',(6.76735698124455,0.172533293857823,136.705295517176));
#42405=CARTESIAN_POINT('Ctrl Pts',(6.76005364423136,0.358556796342125,136.71404509881));
#42406=CARTESIAN_POINT('Ctrl Pts',(6.74510137904359,0.543963589245015,136.722794680444));
#42407=CARTESIAN_POINT('Ctrl Pts',(6.73014936815213,0.729367228895691,136.731544113272));
#42408=CARTESIAN_POINT('Ctrl Pts',(6.7075487124433,0.914153894279106,136.740293546101));
#42409=CARTESIAN_POINT('Ctrl Pts',(6.67737617463727,1.09769596081362,136.749042978929));
#42410=CARTESIAN_POINT('Ctrl Pts',(6.64720410988742,1.28123514970791,136.75779227458));
#42411=CARTESIAN_POINT('Ctrl Pts',(6.60946044708916,1.46352949601816,136.766541570231));
#42412=CARTESIAN_POINT('Ctrl Pts',(6.5642733778979,1.64395985967447,136.775290865883));
#42413=CARTESIAN_POINT('Ctrl Pts',(6.51908695712672,1.8243876342124,136.784040035985));
#42414=CARTESIAN_POINT('Ctrl Pts',(6.46645741331857,2.00295120164824,136.792789206086));
#42415=CARTESIAN_POINT('Ctrl Pts',(6.40656349104716,2.17904411042586,136.801538376188));
#42416=CARTESIAN_POINT('Ctrl Pts',(6.34667034866294,2.35513472627295,136.810287432366));
#42417=CARTESIAN_POINT('Ctrl Pts',(6.27951310937061,2.52875447656288,136.819036488543));
#42418=CARTESIAN_POINT('Ctrl Pts',(6.20531985190598,2.69931371565841,136.827785544721));
#42419=CARTESIAN_POINT('Ctrl Pts',(6.12830387608104,2.87636196348825,136.836867462972));
#42420=CARTESIAN_POINT('Ctrl Pts',(6.04370611833773,3.05011194839779,136.845949381223));
#42421=CARTESIAN_POINT('Ctrl Pts',(5.95183614183747,3.21992787818567,136.855031299473));
#42422=CARTESIAN_POINT('Ctrl Pts',(5.86332597394906,3.38353341100748,136.863781079758));
#42423=CARTESIAN_POINT('Ctrl Pts',(5.76806621040237,3.54348726717114,136.872530860043));
#42424=CARTESIAN_POINT('Ctrl Pts',(5.66638042494076,3.6992461231781,136.881280640328));
#42425=CARTESIAN_POINT('Ctrl Pts',(5.56469829503605,3.8549993797263,136.890030106062));
#42426=CARTESIAN_POINT('Ctrl Pts',(5.45659076217561,4.00655769790067,136.898779571796));
#42427=CARTESIAN_POINT('Ctrl Pts',(5.34242501440727,4.1534063087345,136.90752903753));
#42428=CARTESIAN_POINT('Ctrl Pts',(5.22826276398812,4.30025042101353,136.916278235233));
#42429=CARTESIAN_POINT('Ctrl Pts',(5.10804284592829,4.4423848884234,136.925027432937));
#42430=CARTESIAN_POINT('Ctrl Pts',(4.98217356309145,4.5793269797245,136.93377663064));
#42431=CARTESIAN_POINT('Ctrl Pts',(4.85630746721564,4.71626560370538,136.942525606817));
#42432=CARTESIAN_POINT('Ctrl Pts',(4.72479248669995,4.84801190370368,136.951274582994));
#42433=CARTESIAN_POINT('Ctrl Pts',(4.58807526322912,4.97411845244411,136.960023559171));
#42434=CARTESIAN_POINT('Ctrl Pts',(4.45134915258695,5.10023319861921,136.968773104067));
#42435=CARTESIAN_POINT('Ctrl Pts',(4.30942033290745,5.22070726557791,136.977522648963));
#42436=CARTESIAN_POINT('Ctrl Pts',(4.16277087520749,5.33513145484947,136.986272193859));
#42437=CARTESIAN_POINT('Ctrl Pts',(4.01613003785245,5.44954891804108,136.995021224439));
#42438=CARTESIAN_POINT('Ctrl Pts',(3.8647693436718,5.55791703889848,137.003770255019));
#42439=CARTESIAN_POINT('Ctrl Pts',(3.70920283931706,5.65986778085869,137.0125192856));
#42440=CARTESIAN_POINT('Ctrl Pts',(3.55363422426545,5.76181990606726,137.021268434885));
#42441=CARTESIAN_POINT('Ctrl Pts',(3.39385992450911,5.8573543210766,137.030017584171));
#42442=CARTESIAN_POINT('Ctrl Pts',(3.23042257544398,5.94614656597547,137.038766733456));
#42443=CARTESIAN_POINT('Ctrl Pts',(3.18692938489662,5.96977554704133,137.041095016552));
#42444=CARTESIAN_POINT('Ctrl Pts',(3.14317693223697,5.99292731134156,137.043423299647));
#42445=CARTESIAN_POINT('Ctrl Pts',(3.09917575053248,6.01559628526645,137.045751582743));
#42446=CARTESIAN_POINT('Ctrl Pts',(3.09917575053244,6.01559628526647,135.045784814338));
#42447=CARTESIAN_POINT('Ctrl Pts',(2.94386895177856,6.09560881299704,135.053980427697));
#42448=CARTESIAN_POINT('Ctrl Pts',(2.78543539305422,6.16961655946919,135.062176041057));
#42449=CARTESIAN_POINT('Ctrl Pts',(2.62438265169782,6.23737963390618,135.070371654417));
#42450=CARTESIAN_POINT('Ctrl Pts',(2.46332212967719,6.30514598206408,135.078567663717));
#42451=CARTESIAN_POINT('Ctrl Pts',(2.29964250359656,6.36666691759768,135.086763673017));
#42452=CARTESIAN_POINT('Ctrl Pts',(2.13387138950178,6.42175068755131,135.094959682317));
#42453=CARTESIAN_POINT('Ctrl Pts',(1.96806210663525,6.47684714053392,135.103157578748));
#42454=CARTESIAN_POINT('Ctrl Pts',(1.80016071703524,6.52550336246885,135.111355475178));
#42455=CARTESIAN_POINT('Ctrl Pts',(1.63071009932585,6.56757745077717,135.119553371608));
#42456=CARTESIAN_POINT('Ctrl Pts',(1.46118963574362,6.60966888160958,135.12775464713));
#42457=CARTESIAN_POINT('Ctrl Pts',(1.29011902001511,6.64517268827312,135.135955922652));
#42458=CARTESIAN_POINT('Ctrl Pts',(1.11805147058748,6.67399804533364,135.144157198174));
#42459=CARTESIAN_POINT('Ctrl Pts',(0.945796492507914,6.70285480109678,135.152367407129));
#42460=CARTESIAN_POINT('Ctrl Pts',(0.772542766060607,6.72501852076012,135.160577616085));
#42461=CARTESIAN_POINT('Ctrl Pts',(0.598849659984146,6.74045013962249,135.168787825041));
#42462=CARTESIAN_POINT('Ctrl Pts',(0.42504445880697,6.75589171748041,135.177003332561));
#42463=CARTESIAN_POINT('Ctrl Pts',(0.250799670077478,6.7645925172971,135.185218840082));
#42464=CARTESIAN_POINT('Ctrl Pts',(0.0766746961772759,6.76656559792086,
135.193434347602));
#42465=CARTESIAN_POINT('Ctrl Pts',(-0.0976759411793136,6.76854123562867,
135.201660502302));
#42466=CARTESIAN_POINT('Ctrl Pts',(-0.271906096475163,6.76377175418914,
135.209886657002));
#42467=CARTESIAN_POINT('Ctrl Pts',(-0.445460622895264,6.75232210676074,
135.218112811702));
#42468=CARTESIAN_POINT('Ctrl Pts',(-0.489282012439895,6.74943114522572,
135.22018986228));
#42469=CARTESIAN_POINT('Ctrl Pts',(-0.533060375600027,6.74611455845737,
135.222266912859));
#42470=CARTESIAN_POINT('Ctrl Pts',(-0.576786882283782,6.74237390630521,
135.224343963438));
#42471=CARTESIAN_POINT('Ctrl Pts',(-0.749938123180659,6.72756141358553,
135.23256881176));
#42472=CARTESIAN_POINT('Ctrl Pts',(-0.922761412954599,6.70605378641513,
135.240793660082));
#42473=CARTESIAN_POINT('Ctrl Pts',(-1.09469913561974,6.67786813305515,135.249018508404));
#42474=CARTESIAN_POINT('Ctrl Pts',(-1.26644321828709,6.64971422299018,135.257234093723));
#42475=CARTESIAN_POINT('Ctrl Pts',(-1.43730336899484,6.61489732035186,135.265449679043));
#42476=CARTESIAN_POINT('Ctrl Pts',(-1.60672494982419,6.57348643686229,135.273665264362));
#42477=CARTESIAN_POINT('Ctrl Pts',(-1.77598976455819,6.53211387093815,135.281873247785));
#42478=CARTESIAN_POINT('Ctrl Pts',(-1.94381831403307,6.4841595599196,135.290081231208));
#42479=CARTESIAN_POINT('Ctrl Pts',(-2.10966395224759,6.42974393025003,135.298289214632));
#42480=CARTESIAN_POINT('Ctrl Pts',(-2.2753894441314,6.37536772180557,135.306491251808));
#42481=CARTESIAN_POINT('Ctrl Pts',(-2.43913454650945,6.31453962953897,135.314693288985));
#42482=CARTESIAN_POINT('Ctrl Pts',(-2.60036554707839,6.24743051354457,135.322895326161));
#42483=CARTESIAN_POINT('Ctrl Pts',(-2.76151212099262,6.18035653842347,135.33109306844));
#42484=CARTESIAN_POINT('Ctrl Pts',(-2.92014688529361,6.10700822929251,135.33929081072));
#42485=CARTESIAN_POINT('Ctrl Pts',(-3.07575388260547,6.0276054162194,135.347488552999));
#42486=CARTESIAN_POINT('Ctrl Pts',(-3.23133129382267,5.94821770027678,135.355684736613));
#42487=CARTESIAN_POINT('Ctrl Pts',(-3.38388176265211,5.86277793071786,135.363880920228));
#42488=CARTESIAN_POINT('Ctrl Pts',(-3.53291154513242,5.77155308511237,135.372077103842));
#42489=CARTESIAN_POINT('Ctrl Pts',(-3.68193035694097,5.68033495492859,135.380272684103));
#42490=CARTESIAN_POINT('Ctrl Pts',(-3.82742869203973,5.58333278338579,135.388468264364));
#42491=CARTESIAN_POINT('Ctrl Pts',(-3.96893960261898,5.48085827501156,135.396663844625));
#42492=CARTESIAN_POINT('Ctrl Pts',(-4.11046584225693,5.37837266616636,135.404860312666));
#42493=CARTESIAN_POINT('Ctrl Pts',(-4.24800350613985,5.27041374997989,135.413056780706));
#42494=CARTESIAN_POINT('Ctrl Pts',(-4.38111666396505,5.157335142952,135.421253248747));
#42495=CARTESIAN_POINT('Ctrl Pts',(-4.51426845963583,5.04422371337052,135.42945209592));
#42496=CARTESIAN_POINT('Ctrl Pts',(-4.64299291773781,4.92598986516729,135.437650943094));
#42497=CARTESIAN_POINT('Ctrl Pts',(-4.76688904449317,4.80302590431189,135.445849790267));
#42498=CARTESIAN_POINT('Ctrl Pts',(-4.89091465474872,4.67993343416031,135.454057206033));
#42499=CARTESIAN_POINT('Ctrl Pts',(-5.01010159722915,4.55210122814411,135.462264621799));
#42500=CARTESIAN_POINT('Ctrl Pts',(-5.12408678035863,4.41995742822869,135.470472037565));
#42501=CARTESIAN_POINT('Ctrl Pts',(-5.2381330555376,4.28774280388379,135.478683852217));
#42502=CARTESIAN_POINT('Ctrl Pts',(-5.34697179003514,4.15121225919749,135.486895666869));
#42503=CARTESIAN_POINT('Ctrl Pts',(-5.45028181332655,4.01082499684564,135.495107481522));
#42504=CARTESIAN_POINT('Ctrl Pts',(-5.55374397633277,3.87023099290788,135.503331389319));
#42505=CARTESIAN_POINT('Ctrl Pts',(-5.65166095550955,3.72576921781061,135.511555297117));
#42506=CARTESIAN_POINT('Ctrl Pts',(-5.74375565126593,3.57792677657757,135.519779204914));
#42507=CARTESIAN_POINT('Ctrl Pts',(-5.82884944931349,3.44132309127496,135.527377943838));
#42508=CARTESIAN_POINT('Ctrl Pts',(-5.90897291807125,3.30183366422781,135.534976682761));
#42509=CARTESIAN_POINT('Ctrl Pts',(-5.98394366326475,3.15985873653771,135.542575421685));
#42510=CARTESIAN_POINT('Ctrl Pts',(-6.06893960768602,2.99889871097019,135.551190275246));
#42511=CARTESIAN_POINT('Ctrl Pts',(-6.14754099250621,2.83431097684033,135.559805128807));
#42512=CARTESIAN_POINT('Ctrl Pts',(-6.21943977118642,2.66661919527041,135.568419982368));
#42513=CARTESIAN_POINT('Ctrl Pts',(-6.29121675126856,2.49921148839938,135.57702024212));
#42514=CARTESIAN_POINT('Ctrl Pts',(-6.35631363926335,2.32871049720225,135.585620501872));
#42515=CARTESIAN_POINT('Ctrl Pts',(-6.41446782623058,2.15566498005899,135.594220761623));
#42516=CARTESIAN_POINT('Ctrl Pts',(-6.472486908962,1.98302148353667,135.602801041188));
#42517=CARTESIAN_POINT('Ctrl Pts',(-6.52359536620775,1.80784554277667,135.611381320753));
#42518=CARTESIAN_POINT('Ctrl Pts',(-6.56757851987453,1.63070579360064,135.619961600317));
#42519=CARTESIAN_POINT('Ctrl Pts',(-6.6115023361629,1.45380502247536,135.628530304284));
#42520=CARTESIAN_POINT('Ctrl Pts',(-6.6483199339772,1.27494601980787,135.637099008251));
#42521=CARTESIAN_POINT('Ctrl Pts',(-6.67786559221037,1.09471463513233,135.645667712218));
#42522=CARTESIAN_POINT('Ctrl Pts',(-6.70745774600986,0.914199622986577,
135.654249900628));
#42523=CARTESIAN_POINT('Ctrl Pts',(-6.72975492875082,0.732308194204803,
135.662832089038));
#42524=CARTESIAN_POINT('Ctrl Pts',(-6.74464084693375,0.549644290312154,
135.671414277448));
#42525=CARTESIAN_POINT('Ctrl Pts',(-6.75952676511669,0.366980386419505,
135.679996465858));
#42526=CARTESIAN_POINT('Ctrl Pts',(-6.76700133295404,0.183544311678704,
135.688578654268));
#42527=CARTESIAN_POINT('Ctrl Pts',(-6.7669999998216,-4.91374134034539E-5,
135.697160842678));
#42528=CARTESIAN_POINT('',(-6.76699727515127,-0.00607273375871645,135.302820216236));
#42529=CARTESIAN_POINT('Ctrl Pts',(3.09917575053266,6.01559628526635,134.651234928213));
#42530=CARTESIAN_POINT('Ctrl Pts',(2.94375641574756,6.09566679044796,134.659449205158));
#42531=CARTESIAN_POINT('Ctrl Pts',(2.78532630390312,6.16966174797828,134.667663482103));
#42532=CARTESIAN_POINT('Ctrl Pts',(2.62440605859029,6.23736978538507,134.675877759049));
#42533=CARTESIAN_POINT('Ctrl Pts',(2.46339164215883,6.30511744578405,134.684096843019));
#42534=CARTESIAN_POINT('Ctrl Pts',(2.29988452233624,6.36657072615371,134.692315926989));
#42535=CARTESIAN_POINT('Ctrl Pts',(2.13442169041754,6.42156780291816,134.70053501096));
#42536=CARTESIAN_POINT('Ctrl Pts',(1.96870032426658,6.47665081213555,134.708766937177));
#42537=CARTESIAN_POINT('Ctrl Pts',(1.80101748311864,6.52525735769499,134.716998863395));
#42538=CARTESIAN_POINT('Ctrl Pts',(1.631922906266,6.56727619550178,134.725230789612));
#42539=CARTESIAN_POINT('Ctrl Pts',(1.47238318581289,6.60692071729683,134.732997562692));
#42540=CARTESIAN_POINT('Ctrl Pts',(1.31158709881734,6.64070139695056,134.740764335773));
#42541=CARTESIAN_POINT('Ctrl Pts',(1.15000040363666,6.66856716781315,134.748531108853));
#42542=CARTESIAN_POINT('Ctrl Pts',(0.980327161221296,6.69782747101679,134.75668656726));
#42543=CARTESIAN_POINT('Ctrl Pts',(0.809259701637315,6.72065559255727,134.764842025667));
#42544=CARTESIAN_POINT('Ctrl Pts',(0.637331484518815,6.73692048185527,134.772997484073));
#42545=CARTESIAN_POINT('Ctrl Pts',(0.465612526639907,6.75316557464503,134.781143016215));
#42546=CARTESIAN_POINT('Ctrl Pts',(0.293035256511699,6.76286330225553,134.789288548357));
#42547=CARTESIAN_POINT('Ctrl Pts',(0.120144304616915,6.76593336843248,134.797434080499));
#42548=CARTESIAN_POINT('Ctrl Pts',(-0.0525725717618749,6.76900034350867,
134.8055714113));
#42549=CARTESIAN_POINT('Ctrl Pts',(-0.225602138431937,6.76545293561209,
134.8137087421));
#42550=CARTESIAN_POINT('Ctrl Pts',(-0.398393642743159,6.75526250455316,
134.821846072901));
#42551=CARTESIAN_POINT('Ctrl Pts',(-0.571047484336989,6.74508019219449,
134.829976920703));
#42552=CARTESIAN_POINT('Ctrl Pts',(-0.743463278046017,6.72826541608935,
134.838107768505));
#42553=CARTESIAN_POINT('Ctrl Pts',(-0.915089264245877,6.70484158190646,
134.846238616307));
#42554=CARTESIAN_POINT('Ctrl Pts',(-1.08661456930557,6.68143148887306,134.854364694301));
#42555=CARTESIAN_POINT('Ctrl Pts',(-1.25735062832298,6.65142010819043,134.862490772295));
#42556=CARTESIAN_POINT('Ctrl Pts',(-1.42674980407973,6.61488276514093,134.870616850288));
#42557=CARTESIAN_POINT('Ctrl Pts',(-1.59674963837203,6.57821586734671,134.878771741871));
#42558=CARTESIAN_POINT('Ctrl Pts',(-1.76540272049193,6.53497667053279,134.886926633453));
#42559=CARTESIAN_POINT('Ctrl Pts',(-1.93216428719813,6.48529337557494,134.895081525035));
#42560=CARTESIAN_POINT('Ctrl Pts',(-2.09827554210092,6.43580382809608,134.903204615391));
#42561=CARTESIAN_POINT('Ctrl Pts',(-2.26250965949945,6.37992047329634,134.911327705747));
#42562=CARTESIAN_POINT('Ctrl Pts',(-2.42434222066462,6.31782033593097,134.919450796104));
#42563=CARTESIAN_POINT('Ctrl Pts',(-2.5861874896611,6.2557153221794,134.927574524322));
#42564=CARTESIAN_POINT('Ctrl Pts',(-2.74563048522756,6.18739268450539,134.935698252541));
#42565=CARTESIAN_POINT('Ctrl Pts',(-2.90216584432869,6.11307798183631,134.943821980759));
#42566=CARTESIAN_POINT('Ctrl Pts',(-3.05874327596736,6.03874330535343,134.951947892419));
#42567=CARTESIAN_POINT('Ctrl Pts',(-3.2124111847011,5.95841351387982,134.96007380408));
#42568=CARTESIAN_POINT('Ctrl Pts',(-3.36268796982347,5.87236056604195,134.96819971574));
#42569=CARTESIAN_POINT('Ctrl Pts',(-3.51392579060767,5.78575730065763,134.97637759345));
#42570=CARTESIAN_POINT('Ctrl Pts',(-3.66172863811399,5.69335761111662,134.98455547116));
#42571=CARTESIAN_POINT('Ctrl Pts',(-3.80563511522079,5.59548303275048,134.99273334887));
#42572=CARTESIAN_POINT('Ctrl Pts',(-3.94885475792429,5.49807558851882,135.000872195343));
#42573=CARTESIAN_POINT('Ctrl Pts',(-4.08821488393055,5.39524566857946,135.009011041817));
#42574=CARTESIAN_POINT('Ctrl Pts',(-4.22329412815464,5.28735053756554,135.01714988829));
#42575=CARTESIAN_POINT('Ctrl Pts',(-4.35934506596433,5.17867926209414,135.025347281619));
#42576=CARTESIAN_POINT('Ctrl Pts',(-4.49105301484361,5.06486987451833,135.033544674947));
#42577=CARTESIAN_POINT('Ctrl Pts',(-4.6180256938709,4.94632466491518,135.041742068275));
#42578=CARTESIAN_POINT('Ctrl Pts',(-4.74499837289828,4.82777945531193,135.049939461604));
#42579=CARTESIAN_POINT('Ctrl Pts',(-4.8672355633818,4.70449873103403,135.058136854932));
#42580=CARTESIAN_POINT('Ctrl Pts',(-4.98438690250362,4.57691776265975,135.06633424826));
#42581=CARTESIAN_POINT('Ctrl Pts',(-5.10086689039312,4.45006791388668,135.074484665343));
#42582=CARTESIAN_POINT('Ctrl Pts',(-5.21268078880439,4.31857319100973,135.082635082425));
#42583=CARTESIAN_POINT('Ctrl Pts',(-5.3194320149186,4.18281389003373,135.090785499508));
#42584=CARTESIAN_POINT('Ctrl Pts',(-5.42605861687286,4.0472130779993,135.098926401581));
#42585=CARTESIAN_POINT('Ctrl Pts',(-5.52763408874244,3.90735788464401,135.107067303655));
#42586=CARTESIAN_POINT('Ctrl Pts',(-5.62379884921759,3.76366516889308,135.115208205728));
#42587=CARTESIAN_POINT('Ctrl Pts',(-5.71985329518928,3.62013728889394,135.123339769042));
#42588=CARTESIAN_POINT('Ctrl Pts',(-5.81050919468711,3.47278096033235,135.131471332356));
#42589=CARTESIAN_POINT('Ctrl Pts',(-5.89544760215918,3.32204554005445,135.13960289567));
#42590=CARTESIAN_POINT('Ctrl Pts',(-5.98033041312994,3.17140878376426,135.147729136463));
#42591=CARTESIAN_POINT('Ctrl Pts',(-6.05950300213959,3.01739765578338,135.155855377256));
#42592=CARTESIAN_POINT('Ctrl Pts',(-6.13268982894256,2.8604902485386,135.163981618048));
#42593=CARTESIAN_POINT('Ctrl Pts',(-6.20584271886969,2.70365559956784,135.172104090687));
#42594=CARTESIAN_POINT('Ctrl Pts',(-6.27301521813021,2.5439276762172,135.180226563326));
#42595=CARTESIAN_POINT('Ctrl Pts',(-6.33397785597443,2.38180887562909,135.188349035965));
#42596=CARTESIAN_POINT('Ctrl Pts',(-6.39492385896012,2.21973431235435,135.196469292227));
#42597=CARTESIAN_POINT('Ctrl Pts',(-6.4496632467032,2.05527051365083,135.204589548489));
#42598=CARTESIAN_POINT('Ctrl Pts',(-6.49801481700214,1.88893950088949,135.212709804751));
#42599=CARTESIAN_POINT('Ctrl Pts',(-6.54637421784645,1.72258155079119,135.22083137609));
#42600=CARTESIAN_POINT('Ctrl Pts',(-6.58834362541911,1.55435613228336,135.228952947429));
#42601=CARTESIAN_POINT('Ctrl Pts',(-6.62379172668878,1.38480040491377,135.237074518768));
#42602=CARTESIAN_POINT('Ctrl Pts',(-6.65924229645898,1.21523287018671,135.245196655669));
#42603=CARTESIAN_POINT('Ctrl Pts',(-6.68817058647215,1.04433520189303,135.25331879257));
#42604=CARTESIAN_POINT('Ctrl Pts',(-6.71049652523991,0.872654218315073,
135.261440929471));
#42605=CARTESIAN_POINT('Ctrl Pts',(-6.73283687678045,0.700862404055715,
135.269568309714));
#42606=CARTESIAN_POINT('Ctrl Pts',(-6.748566321262,0.528286628481025,135.277695689956));
#42607=CARTESIAN_POINT('Ctrl Pts',(-6.75765667739668,0.355478874809866,
135.285823070198));
#42608=CARTESIAN_POINT('Ctrl Pts',(-6.76399369727002,0.235012068773062,
135.291488785529));
#42609=CARTESIAN_POINT('Ctrl Pts',(-6.76710541717883,0.11443261880474,135.297154500859));
#42610=CARTESIAN_POINT('Ctrl Pts',(-6.76699727515214,-0.00607273278968599,
135.30282021619));
#42611=CARTESIAN_POINT('Ctrl Pts',(-6.76699727515127,-0.0060727337587121,
135.302820216236));
#42612=CARTESIAN_POINT('Ctrl Pts',(-6.76679986671651,-0.226049830262332,
135.31316272461));
#42613=CARTESIAN_POINT('Ctrl Pts',(-6.75587263188703,-0.445562092144057,
135.323505232985));
#42614=CARTESIAN_POINT('Ctrl Pts',(-6.73437268671693,-0.663711922750399,
135.333847741359));
#42615=CARTESIAN_POINT('Ctrl Pts',(-6.71248172404542,-0.88582922401878,
135.344378347971));
#42616=CARTESIAN_POINT('Ctrl Pts',(-6.67962999568742,-1.10653425722591,
135.354908954583));
#42617=CARTESIAN_POINT('Ctrl Pts',(-6.63603191500124,-1.32490355237086,
135.365439561194));
#42618=CARTESIAN_POINT('Ctrl Pts',(-6.61022810402908,-1.45414685678616,
135.371672170019));
#42619=CARTESIAN_POINT('Ctrl Pts',(-6.58066082080314,-1.5825724067862,135.377904778844));
#42620=CARTESIAN_POINT('Ctrl Pts',(-6.54738235195893,-1.70999220385846,
135.384137387669));
#42621=CARTESIAN_POINT('Ctrl Pts',(-6.5034592722332,-1.87816910922156,135.392363588688));
#42622=CARTESIAN_POINT('Ctrl Pts',(-6.45299091726314,-2.04488766880344,
135.400589789706));
#42623=CARTESIAN_POINT('Ctrl Pts',(-6.3960888113794,-2.20960107642698,135.408815990725));
#42624=CARTESIAN_POINT('Ctrl Pts',(-6.3392506230189,-2.37412946325213,135.417032951341));
#42625=CARTESIAN_POINT('Ctrl Pts',(-6.27599319063386,-2.53665684729028,
135.425249911957));
#42626=CARTESIAN_POINT('Ctrl Pts',(-6.20647868369198,-2.69664816927923,
135.433466872572));
#42627=CARTESIAN_POINT('Ctrl Pts',(-6.13702830953398,-2.85649188626708,
135.441676252374));
#42628=CARTESIAN_POINT('Ctrl Pts',(-6.06133249930582,-3.01380387398899,
135.449885632176));
#42629=CARTESIAN_POINT('Ctrl Pts',(-5.97960273516409,-3.16806567634228,
135.458095011977));
#42630=CARTESIAN_POINT('Ctrl Pts',(-5.89793197482443,-3.32221611127702,
135.466298465118));
#42631=CARTESIAN_POINT('Ctrl Pts',(-5.81023610447354,-3.47332043131457,
135.474501918258));
#42632=CARTESIAN_POINT('Ctrl Pts',(-5.71677411393429,-3.62088148525339,
135.482705371398));
#42633=CARTESIAN_POINT('Ctrl Pts',(-5.62336084889186,-3.76836560967657,
135.490904547749));
#42634=CARTESIAN_POINT('Ctrl Pts',(-5.52418764381147,-3.91230984579046,
135.499103724099));
#42635=CARTESIAN_POINT('Ctrl Pts',(-5.41955873637874,-4.05224284846564,
135.507302900449));
#42636=CARTESIAN_POINT('Ctrl Pts',(-5.31494951645399,-4.19214952063451,
135.515500534));
#42637=CARTESIAN_POINT('Ctrl Pts',(-5.20488684855691,-4.32804617214016,
135.523698167552));
#42638=CARTESIAN_POINT('Ctrl Pts',(-5.08971766663502,-4.45949134699726,
135.531895801103));
#42639=CARTESIAN_POINT('Ctrl Pts',(-4.97455677972071,-4.59092705457584,
135.540092844224));
#42640=CARTESIAN_POINT('Ctrl Pts',(-4.85429034697056,-4.71791165367092,
135.548289887344));
#42641=CARTESIAN_POINT('Ctrl Pts',(-4.72930483669364,-4.84003768183949,
135.556486930465));
#42642=CARTESIAN_POINT('Ctrl Pts',(-4.60430561253319,-4.96217711013838,
135.564684872996));
#42643=CARTESIAN_POINT('Ctrl Pts',(-4.47458653584447,-5.07945665469392,
135.572882815527));
#42644=CARTESIAN_POINT('Ctrl Pts',(-4.3405701204733,-5.19150652790252,135.581080758058));
#42645=CARTESIAN_POINT('Ctrl Pts',(-4.2065146429628,-5.30358906060097,135.589281090067));
#42646=CARTESIAN_POINT('Ctrl Pts',(-4.06815960692982,-5.41043865570606,
135.597481422075));
#42647=CARTESIAN_POINT('Ctrl Pts',(-3.92595973287986,-5.51172651496842,
135.605681754084));
#42648=CARTESIAN_POINT('Ctrl Pts',(-3.78361164812745,-5.61311994355615,
135.613890633054));
#42649=CARTESIAN_POINT('Ctrl Pts',(-3.63741101178872,-5.70893984674031,
135.622099512025));
#42650=CARTESIAN_POINT('Ctrl Pts',(-3.48784143229593,-5.79890085646926,
135.630308390996));
#42651=CARTESIAN_POINT('Ctrl Pts',(-3.3381915603836,-5.88891015935487,135.638521676683));
#42652=CARTESIAN_POINT('Ctrl Pts',(-3.18516945394858,-5.9730541260828,135.646734962371));
#42653=CARTESIAN_POINT('Ctrl Pts',(-3.02928222881453,-6.05109396540729,
135.654948248058));
#42654=CARTESIAN_POINT('Ctrl Pts',(-2.87316695988291,-6.12924796739845,
135.66317354877));
#42655=CARTESIAN_POINT('Ctrl Pts',(-2.71417852287252,-6.20127984877912,
135.671398849482));
#42656=CARTESIAN_POINT('Ctrl Pts',(-2.55284404967992,-6.26699898340616,
135.679624150194));
#42657=CARTESIAN_POINT('Ctrl Pts',(-2.40693648010347,-6.32643401312018,
135.687062942488));
#42658=CARTESIAN_POINT('Ctrl Pts',(-2.25911048961878,-6.38070641181775,
135.694501734782));
#42659=CARTESIAN_POINT('Ctrl Pts',(-2.10976495382097,-6.42971078973455,
135.701940527076));
#42660=CARTESIAN_POINT('Ctrl Pts',(-1.94608947698599,-6.48341721543843,
135.710093083289));
#42661=CARTESIAN_POINT('Ctrl Pts',(-1.78010591636705,-6.53095375125263,
135.718245639503));
#42662=CARTESIAN_POINT('Ctrl Pts',(-1.61232421108503,-6.5721153092706,135.726398195716));
#42663=CARTESIAN_POINT('Ctrl Pts',(-1.44473688495347,-6.61322918063129,
135.734541306996));
#42664=CARTESIAN_POINT('Ctrl Pts',(-1.27535591236074,-6.64798268966008,
135.742684418277));
#42665=CARTESIAN_POINT('Ctrl Pts',(-1.104709404532,-6.67621944902492,135.750827529557));
#42666=CARTESIAN_POINT('Ctrl Pts',(-0.934224718493542,-6.70442943185028,
135.758962918834));
#42667=CARTESIAN_POINT('Ctrl Pts',(-0.762477244622202,-6.72613490882853,
135.767098308112));
#42668=CARTESIAN_POINT('Ctrl Pts',(-0.590008392774742,-6.74122979110306,
135.775233697389));
#42669=CARTESIAN_POINT('Ctrl Pts',(-0.41766685095481,-6.75631353090254,
135.783363081428));
#42670=CARTESIAN_POINT('Ctrl Pts',(-0.244605354082271,-6.76479636058453,
135.791492465466));
#42671=CARTESIAN_POINT('Ctrl Pts',(-0.0713735999031859,-6.76662359003638,
135.799621849505));
#42672=CARTESIAN_POINT('Ctrl Pts',(0.101766668056435,-6.76844985450167,
135.807746940297));
#42673=CARTESIAN_POINT('Ctrl Pts',(0.27507664952675,-6.76362751499981,135.815872031089));
#42674=CARTESIAN_POINT('Ctrl Pts',(0.448003455664473,-6.75215387144818,
135.823997121881));
#42675=CARTESIAN_POINT('Ctrl Pts',(0.621590360909375,-6.7406364305118,135.832153227906));
#42676=CARTESIAN_POINT('Ctrl Pts',(0.794790788257611,-6.72241678171025,
135.840309333931));
#42677=CARTESIAN_POINT('Ctrl Pts',(0.967046932838719,-6.69754501512959,
135.848465439957));
#42678=CARTESIAN_POINT('Ctrl Pts',(1.13860977759075,-6.67277335291131,135.85658871913));
#42679=CARTESIAN_POINT('Ctrl Pts',(1.3092355651262,-6.64140309460029,135.864711998303));
#42680=CARTESIAN_POINT('Ctrl Pts',(1.47838010729718,-6.60353551200779,135.872835277477));
#42681=CARTESIAN_POINT('Ctrl Pts',(1.64754717249343,-6.56566288702664,135.880959638333));
#42682=CARTESIAN_POINT('Ctrl Pts',(1.81523224243433,-6.5212912944284,135.88908399919));
#42683=CARTESIAN_POINT('Ctrl Pts',(1.98090320622816,-6.47057273257592,135.897208360047));
#42684=CARTESIAN_POINT('Ctrl Pts',(2.14662775026381,-6.41983776765107,135.905335348432));
#42685=CARTESIAN_POINT('Ctrl Pts',(2.31033654141122,-6.36275185293676,135.913462336818));
#42686=CARTESIAN_POINT('Ctrl Pts',(2.4715145046851,-6.29951625548591,135.921589325203));
#42687=CARTESIAN_POINT('Ctrl Pts',(2.63373446514111,-6.23587184709703,135.929768853643));
#42688=CARTESIAN_POINT('Ctrl Pts',(2.79339041138535,-6.16599810356462,135.937948382083));
#42689=CARTESIAN_POINT('Ctrl Pts',(2.94998031069297,-6.09014820562881,135.946127910523));
#42690=CARTESIAN_POINT('Ctrl Pts',(3.10583277768259,-6.01465550931522,135.954268918927));
#42691=CARTESIAN_POINT('Ctrl Pts',(3.25864772138151,-5.93324305328491,135.962409927331));
#42692=CARTESIAN_POINT('Ctrl Pts',(3.40795773782195,-5.8462050132731,135.970550935734));
#42693=CARTESIAN_POINT('Ctrl Pts',(3.55832746830142,-5.75854922881836,135.978749724193));
#42694=CARTESIAN_POINT('Ctrl Pts',(3.70514201828591,-5.66518791531266,135.986948512651));
#42695=CARTESIAN_POINT('Ctrl Pts',(3.847956675002,-5.56646372729649,135.995147301109));
#42696=CARTESIAN_POINT('Ctrl Pts',(3.99077133171809,-5.46773953928033,136.003346089567));
#42697=CARTESIAN_POINT('Ctrl Pts',(4.12958583691194,-5.36365275137169,136.011544878026));
#42698=CARTESIAN_POINT('Ctrl Pts',(4.26399241036301,-5.2545844483048,136.019743666484));
#42699=CARTESIAN_POINT('Ctrl Pts',(4.39896065145484,-5.14506036294325,136.027976716616));
#42700=CARTESIAN_POINT('Ctrl Pts',(4.52990367279796,-5.03017267465564,136.036209766748));
#42701=CARTESIAN_POINT('Ctrl Pts',(4.65636808142651,-4.91024696835835,136.04444281688));
#42702=CARTESIAN_POINT('Ctrl Pts',(4.78268189038405,-4.79046407514272,136.052666062715));
#42703=CARTESIAN_POINT('Ctrl Pts',(4.90452744927105,-4.6656553544627,136.06088930855));
#42704=CARTESIAN_POINT('Ctrl Pts',(5.02148275758391,-4.53618781746165,136.069112554384));
#42705=CARTESIAN_POINT('Ctrl Pts',(5.1383221989597,-4.40684854318915,136.077327653498));
#42706=CARTESIAN_POINT('Ctrl Pts',(5.25028079967261,-4.27285990830849,136.085542752611));
#42707=CARTESIAN_POINT('Ctrl Pts',(5.35697183840158,-4.13462715641598,136.093757851725));
#42708=CARTESIAN_POINT('Ctrl Pts',(5.46357852567245,-3.9965036933102,136.101966455864));
#42709=CARTESIAN_POINT('Ctrl Pts',(5.56492572816444,-3.85414307886854,136.110175060003));
#42710=CARTESIAN_POINT('Ctrl Pts',(5.66066555732851,-3.70798522759661,136.118383664142));
#42711=CARTESIAN_POINT('Ctrl Pts',(5.75634884385217,-3.56191369516294,136.126587420391));
#42712=CARTESIAN_POINT('Ctrl Pts',(5.84643115854175,-3.41204969227551,136.13479117664));
#42713=CARTESIAN_POINT('Ctrl Pts',(5.93060663138424,-3.25886390998172,136.142994932889));
#42714=CARTESIAN_POINT('Ctrl Pts',(6.01475719882597,-3.10572345149982,136.151196261853));
#42715=CARTESIAN_POINT('Ctrl Pts',(6.09300423008896,-2.94926348302826,136.159397590817));
#42716=CARTESIAN_POINT('Ctrl Pts',(6.16508658856647,-2.78998142565105,136.167598919781));
#42717=CARTESIAN_POINT('Ctrl Pts',(6.23715900619858,-2.6307213347902,136.175799117704));
#42718=CARTESIAN_POINT('Ctrl Pts',(6.30306829588569,-2.46864025613144,136.183999315627));
#42719=CARTESIAN_POINT('Ctrl Pts',(6.36260047293043,-2.30425784621979,136.192199513549));
#42720=CARTESIAN_POINT('Ctrl Pts',(6.42213522836136,-2.13986831677454,136.200400066629));
#42721=CARTESIAN_POINT('Ctrl Pts',(6.47529219883229,-1.97317759437616,136.208600619709));
#42722=CARTESIAN_POINT('Ctrl Pts',(6.52190649157642,-1.80472289150809,136.216801172789));
#42723=CARTESIAN_POINT('Ctrl Pts',(6.56853125064582,-1.63623036544012,136.225003567142));
#42724=CARTESIAN_POINT('Ctrl Pts',(6.60861031056241,-1.46597341528508,136.233205961495));
#42725=CARTESIAN_POINT('Ctrl Pts',(6.6420293341823,-1.29450195977522,136.241408355848));
#42726=CARTESIAN_POINT('Ctrl Pts',(6.67547961046399,-1.12287014831153,136.249618420882));
#42727=CARTESIAN_POINT('Ctrl Pts',(6.70225733818844,-0.950021914430184,
136.257828485916));
#42728=CARTESIAN_POINT('Ctrl Pts',(6.72229962242656,-0.776515799146235,
136.26603855095));
#42729=CARTESIAN_POINT('Ctrl Pts',(6.74235149854637,-0.602926646913526,
136.274252545175));
#42730=CARTESIAN_POINT('Ctrl Pts',(6.75566147684693,-0.428679342564065,
136.282466539401));
#42731=CARTESIAN_POINT('Ctrl Pts',(6.76221877328653,-0.254334940995662,
136.290680533626));
#42732=CARTESIAN_POINT('Ctrl Pts',(6.76878500950514,-0.0797528499407057,
136.298905726261));
#42733=CARTESIAN_POINT('Ctrl Pts',(6.76858016566121,0.0949262445043662,
136.307130918896));
#42734=CARTESIAN_POINT('Ctrl Pts',(6.76164560026206,0.269142669334809,136.315356111531));
#42735=CARTESIAN_POINT('Ctrl Pts',(6.75540936045118,0.425815127045349,136.322753009651));
#42736=CARTESIAN_POINT('Ctrl Pts',(6.74373126377443,0.582113277860358,136.330149907771));
#42737=CARTESIAN_POINT('Ctrl Pts',(6.72667688091511,0.737636183875304,136.337546805891));
#42738=CARTESIAN_POINT('Ctrl Pts',(6.7067426300531,0.919421279757408,136.346192772382));
#42739=CARTESIAN_POINT('Ctrl Pts',(6.67941735311857,1.1005597477816,136.354838738873));
#42740=CARTESIAN_POINT('Ctrl Pts',(6.64475423594991,1.28044138632964,136.363484705364));
#42741=CARTESIAN_POINT('Ctrl Pts',(6.6101354576204,1.46009293180789,136.372119612488));
#42742=CARTESIAN_POINT('Ctrl Pts',(6.56819761291054,1.63849055556209,136.380754519613));
#42743=CARTESIAN_POINT('Ctrl Pts',(6.51904550524376,1.81503022028866,136.389389426737));
#42744=CARTESIAN_POINT('Ctrl Pts',(6.46826158727407,1.99743085939558,136.398311005809));
#42745=CARTESIAN_POINT('Ctrl Pts',(6.40977616501106,2.17784773207027,136.40723258488));
#42746=CARTESIAN_POINT('Ctrl Pts',(6.34376261036176,2.35562410910064,136.416154163952));
#42747=CARTESIAN_POINT('Ctrl Pts',(6.28004669104689,2.52721288893735,136.424765222927));
#42748=CARTESIAN_POINT('Ctrl Pts',(6.20931793043112,2.69634154520653,136.433376281903));
#42749=CARTESIAN_POINT('Ctrl Pts',(6.1317834083069,2.86243274743919,136.441987340879));
#42750=CARTESIAN_POINT('Ctrl Pts',(6.05432200481651,3.02836731800034,136.450590279228));
#42751=CARTESIAN_POINT('Ctrl Pts',(5.97006776449354,3.19126987008528,136.459193217578));
#42752=CARTESIAN_POINT('Ctrl Pts',(5.8792761950018,3.35058210209587,136.467796155927));
#42753=CARTESIAN_POINT('Ctrl Pts',(5.78858629106469,3.50971594126098,136.476389460976));
#42754=CARTESIAN_POINT('Ctrl Pts',(5.69137381241983,3.66526721640593,136.484982766025));
#42755=CARTESIAN_POINT('Ctrl Pts',(5.58794071107854,3.81670114227865,136.493576071074));
#42756=CARTESIAN_POINT('Ctrl Pts',(5.57641657056191,3.83357336034144,136.494533505914));
#42757=CARTESIAN_POINT('Ctrl Pts',(5.56481525689396,3.85039449191347,136.495490940755));
#42758=CARTESIAN_POINT('Ctrl Pts',(5.55313722300797,3.86716381634439,136.496448375595));
#42759=CARTESIAN_POINT('Ctrl Pts',(5.4482957167536,4.01771323668101,136.505043907326));
#42760=CARTESIAN_POINT('Ctrl Pts',(5.33738994259946,4.16390834428211,136.513639439056));
#42761=CARTESIAN_POINT('Ctrl Pts',(5.22081277752856,4.3052761748806,136.522234970787));
#42762=CARTESIAN_POINT('Ctrl Pts',(5.10412689175144,4.44677584613904,136.530838518772));
#42763=CARTESIAN_POINT('Ctrl Pts',(4.98175925188976,4.58343901883024,136.539442066758));
#42764=CARTESIAN_POINT('Ctrl Pts',(4.85414105635593,4.71482805677999,136.548045614743));
#42765=CARTESIAN_POINT('Ctrl Pts',(4.72629659892285,4.84645004218008,136.556664416472));
#42766=CARTESIAN_POINT('Ctrl Pts',(4.59318318588712,4.9727789761998,136.5652832182));
#42767=CARTESIAN_POINT('Ctrl Pts',(4.45526823835273,5.09341476068122,136.573902019928));
#42768=CARTESIAN_POINT('Ctrl Pts',(4.31723216976737,5.21415649113343,136.582528390947));
#42769=CARTESIAN_POINT('Ctrl Pts',(4.17438638564857,5.32919489817194,136.591154761965));
#42770=CARTESIAN_POINT('Ctrl Pts',(4.02722979680182,5.43817149083693,136.599781132984));
#42771=CARTESIAN_POINT('Ctrl Pts',(3.87980799723326,5.54734448490691,136.608423050749));
#42772=CARTESIAN_POINT('Ctrl Pts',(3.72806010805104,5.65043364266486,136.617064968514));
#42773=CARTESIAN_POINT('Ctrl Pts',(3.57251416560888,5.74712376206776,136.625706886278));
#42774=CARTESIAN_POINT('Ctrl Pts',(3.41828942990522,5.84299259590516,136.634275399621));
#42775=CARTESIAN_POINT('Ctrl Pts',(3.26033119644323,5.93257059232623,136.642843912964));
#42776=CARTESIAN_POINT('Ctrl Pts',(3.0991757505325,6.01559628526643,136.651412426306));
#42777=CARTESIAN_POINT('Origin',(0.,0.,-3.69717978381041));
#42778=CARTESIAN_POINT('',(3.09917575053254,6.01559628526642,139.045839590042));
#42779=CARTESIAN_POINT('',(3.09917575053274,6.01559628526631,138.651549674451));
#42780=CARTESIAN_POINT('',(3.09917575053259,6.01559628526639,-3.69717978381041));
#42781=CARTESIAN_POINT('',(-6.7669998232546,-0.000434751987798659,137.69717978381));
#42782=CARTESIAN_POINT('Ctrl Pts',(-6.76699776313827,-0.00550215245942883,
137.69717978381));
#42783=CARTESIAN_POINT('Ctrl Pts',(-6.76680634472756,-0.24092419258413,
137.708261686933));
#42784=CARTESIAN_POINT('Ctrl Pts',(-6.75432628838775,-0.475813744433624,
137.719343590055));
#42785=CARTESIAN_POINT('Ctrl Pts',(-6.72974340733669,-0.709114004521386,
137.730425493178));
#42786=CARTESIAN_POINT('Ctrl Pts',(-6.70434842898574,-0.950121356015059,
137.741873487793));
#42787=CARTESIAN_POINT('Ctrl Pts',(-6.66603767317495,-1.18943322621959,
137.753321482407));
#42788=CARTESIAN_POINT('Ctrl Pts',(-6.61506338143551,-1.42591215002575,
137.764769477022));
#42789=CARTESIAN_POINT('Ctrl Pts',(-6.60700973581777,-1.46327446313319,
137.766578194485));
#42790=CARTESIAN_POINT('Ctrl Pts',(-6.59864007656568,-1.50056610371897,
137.768386911949));
#42791=CARTESIAN_POINT('Ctrl Pts',(-6.58995550656827,-1.5377826314049,137.770195629413));
#42792=CARTESIAN_POINT('Ctrl Pts',(-6.55081850664034,-1.70549885014642,
137.778346611587));
#42793=CARTESIAN_POINT('Ctrl Pts',(-6.50521320785507,-1.87198348611265,
137.786497593761));
#42794=CARTESIAN_POINT('Ctrl Pts',(-6.45322902003838,-2.03669443337349,
137.794648575935));
#42795=CARTESIAN_POINT('Ctrl Pts',(-6.4013052166738,-2.20121405360344,137.802790089988));
#42796=CARTESIAN_POINT('Ctrl Pts',(-6.34301738273073,-2.36396374115074,
137.810931604041));
#42797=CARTESIAN_POINT('Ctrl Pts',(-6.2785059857144,-2.5244111367502,137.819073118094));
#42798=CARTESIAN_POINT('Ctrl Pts',(-6.21405594910061,-2.68470592184615,
137.827206888297));
#42799=CARTESIAN_POINT('Ctrl Pts',(-6.14339426990799,-2.84270243767562,
137.8353406585));
#42800=CARTESIAN_POINT('Ctrl Pts',(-6.06671130901988,-2.99788306860195,
137.843474428703));
#42801=CARTESIAN_POINT('Ctrl Pts',(-5.9900851575855,-3.15294873622001,137.851602173121));
#42802=CARTESIAN_POINT('Ctrl Pts',(-5.90744676789015,-3.30520234622276,
137.859729917539));
#42803=CARTESIAN_POINT('Ctrl Pts',(-5.81903473287829,-3.45414588249484,
137.867857661957));
#42804=CARTESIAN_POINT('Ctrl Pts',(-5.73066960866939,-3.60301039037583,
137.875981093851));
#42805=CARTESIAN_POINT('Ctrl Pts',(-5.63653712633621,-3.74856800846109,
137.884104525745));
#42806=CARTESIAN_POINT('Ctrl Pts',(-5.53692196945519,-3.89034498523774,
137.89222795764));
#42807=CARTESIAN_POINT('Ctrl Pts',(-5.43667489320057,-4.03302133938991,
137.90040292139));
#42808=CARTESIAN_POINT('Ctrl Pts',(-5.330875513871,-4.17186858700254,137.908577885141));
#42809=CARTESIAN_POINT('Ctrl Pts',(-5.21985875539365,-4.30643281309952,
137.916752848892));
#42810=CARTESIAN_POINT('Ctrl Pts',(-5.10956682858407,-4.44011846542296,
137.924874438065));
#42811=CARTESIAN_POINT('Ctrl Pts',(-4.99412570466661,-4.56957658910254,
137.932996027238));
#42812=CARTESIAN_POINT('Ctrl Pts',(-4.87390450601608,-4.69439494144199,
137.941117616411));
#42813=CARTESIAN_POINT('Ctrl Pts',(-4.75366743570169,-4.81922977236388,
137.9492402778));
#42814=CARTESIAN_POINT('Ctrl Pts',(-4.62864928759518,-4.93942334823802,
137.95736293919));
#42815=CARTESIAN_POINT('Ctrl Pts',(-4.49925625483112,-5.05460009826327,
137.965485600579));
#42816=CARTESIAN_POINT('Ctrl Pts',(-4.36982149927201,-5.16981398704192,
137.973610881121));
#42817=CARTESIAN_POINT('Ctrl Pts',(-4.23600932318569,-5.28000758547039,
137.981736161664));
#42818=CARTESIAN_POINT('Ctrl Pts',(-4.09825916716812,-5.38484547584445,
137.989861442206));
#42819=CARTESIAN_POINT('Ctrl Pts',(-3.95900825178452,-5.49082555327981,
137.998075245994));
#42820=CARTESIAN_POINT('Ctrl Pts',(-3.81573335245716,-5.59133230767598,
138.006289049781));
#42821=CARTESIAN_POINT('Ctrl Pts',(-3.66891787395882,-5.68606459989205,
138.014502853569));
#42822=CARTESIAN_POINT('Ctrl Pts',(-3.52343336359155,-5.77993808850503,
138.022642194424));
#42823=CARTESIAN_POINT('Ctrl Pts',(-3.37447255167075,-5.86814125164929,
138.03078153528));
#42824=CARTESIAN_POINT('Ctrl Pts',(-3.22252959690908,-5.95042788352611,
138.038920876135));
#42825=CARTESIAN_POINT('Ctrl Pts',(-3.06850156212743,-6.03384371690035,
138.047171911389));
#42826=CARTESIAN_POINT('Ctrl Pts',(-2.91140929657605,-6.11117928556882,
138.055422946643));
#42827=CARTESIAN_POINT('Ctrl Pts',(-2.7517870228635,-6.18222914334304,138.063673981897));
#42828=CARTESIAN_POINT('Ctrl Pts',(-2.59216474915094,-6.25327900111727,
138.071925017151));
#42829=CARTESIAN_POINT('Ctrl Pts',(-2.43001284864779,-6.31804306789245,
138.080176052405));
#42830=CARTESIAN_POINT('Ctrl Pts',(-2.26587948645026,-6.37636880621596,
138.088427087659));
#42831=CARTESIAN_POINT('Ctrl Pts',(-2.10212931708763,-6.43455837475218,
138.09665885969));
#42832=CARTESIAN_POINT('Ctrl Pts',(-1.93589578800268,-6.4865214679517,138.104890631721));
#42833=CARTESIAN_POINT('Ctrl Pts',(-1.76769268313256,-6.53204038398414,
138.113122403752));
#42834=CARTESIAN_POINT('Ctrl Pts',(-1.59969042957885,-6.57750494588195,
138.121344346224));
#42835=CARTESIAN_POINT('Ctrl Pts',(-1.42972362582028,-6.61654056044007,
138.129566288696));
#42836=CARTESIAN_POINT('Ctrl Pts',(-1.25832510178768,-6.64897788672898,
138.137788231169));
#42837=CARTESIAN_POINT('Ctrl Pts',(-1.08709690351991,-6.68138297871226,
138.146002003159));
#42838=CARTESIAN_POINT('Ctrl Pts',(-0.914440168031664,-6.70720277447715,
138.154215775149));
#42839=CARTESIAN_POINT('Ctrl Pts',(-0.740902019958573,-6.72631795240318,
138.162429547139));
#42840=CARTESIAN_POINT('Ctrl Pts',(-0.567501566619891,-6.74541796329316,
138.170636801869));
#42841=CARTESIAN_POINT('Ctrl Pts',(-0.393221448224845,-6.75782391320529,
138.178844056599));
#42842=CARTESIAN_POINT('Ctrl Pts',(-0.218618191936567,-6.76346768205145,
138.18705131133));
#42843=CARTESIAN_POINT('Ctrl Pts',(-0.0441185140205303,-6.76910810289367,
138.195253697342));
#42844=CARTESIAN_POINT('Ctrl Pts',(0.130703562748177,-6.76799432244862,
138.203456083354));
#42845=CARTESIAN_POINT('Ctrl Pts',(0.305287093792983,-6.76011011673356,
138.211658469366));
#42846=CARTESIAN_POINT('Ctrl Pts',(0.479818515888508,-6.75222826426267,
138.219858407164));
#42847=CARTESIAN_POINT('Ctrl Pts',(0.654111176415007,-6.73758002415768,
138.228058344963));
#42848=CARTESIAN_POINT('Ctrl Pts',(0.827604583781613,-6.71620128144651,
138.236258282762));
#42849=CARTESIAN_POINT('Ctrl Pts',(1.00107373229203,-6.69482552803535,138.244457073997));
#42850=CARTESIAN_POINT('Ctrl Pts',(1.17374349451156,-6.66672118934978,138.252655865233));
#42851=CARTESIAN_POINT('Ctrl Pts',(1.34505892949523,-6.63197598579678,138.260854656469));
#42852=CARTESIAN_POINT('Ctrl Pts',(1.51638148766872,-6.5972293375597,138.269053788605));
#42853=CARTESIAN_POINT('Ctrl Pts',(1.68634925510853,-6.55584134552222,138.277252920742));
#42854=CARTESIAN_POINT('Ctrl Pts',(1.85441784894717,-6.50795078665367,138.285452052878));
#42855=CARTESIAN_POINT('Ctrl Pts',(2.02252391937709,-6.46004954896132,138.293653013289));
#42856=CARTESIAN_POINT('Ctrl Pts',(2.18872962810827,-6.40564295472346,138.3018539737));
#42857=CARTESIAN_POINT('Ctrl Pts',(2.35250605513895,-6.34491956296804,138.310054934111));
#42858=CARTESIAN_POINT('Ctrl Pts',(2.51643598010764,-6.28413925877662,138.318263580796));
#42859=CARTESIAN_POINT('Ctrl Pts',(2.6779317379114,-6.21703045331984,138.326472227481));
#42860=CARTESIAN_POINT('Ctrl Pts',(2.83648381696526,-6.14383012103152,138.334680874166));
#42861=CARTESIAN_POINT('Ctrl Pts',(2.99511159323484,-6.07059484084863,138.34289343989));
#42862=CARTESIAN_POINT('Ctrl Pts',(3.15079256944966,-5.99126239789787,138.351106005613));
#42863=CARTESIAN_POINT('Ctrl Pts',(3.3030422132211,-5.90611557097213,138.359318571337));
#42864=CARTESIAN_POINT('Ctrl Pts',(3.4555007654734,-5.82085191031318,138.367542405885));
#42865=CARTESIAN_POINT('Ctrl Pts',(3.60451826961661,-5.72975810790641,138.375766240434));
#42866=CARTESIAN_POINT('Ctrl Pts',(3.74963850414986,-5.63316075469153,138.383990074983));
#42867=CARTESIAN_POINT('Ctrl Pts',(3.88297670128961,-5.54440595790133,138.391546231957));
#42868=CARTESIAN_POINT('Ctrl Pts',(4.0130249464866,-5.45100559476595,138.399102388932));
#42869=CARTESIAN_POINT('Ctrl Pts',(4.13945490553084,-5.3532422031024,138.406658545906));
#42870=CARTESIAN_POINT('Ctrl Pts',(4.28411544963616,-5.24138180594225,138.415304263959));
#42871=CARTESIAN_POINT('Ctrl Pts',(4.42436852531527,-5.12355421362863,138.423949982011));
#42872=CARTESIAN_POINT('Ctrl Pts',(4.55972131160622,-5.00012305453416,138.432595700064));
#42873=CARTESIAN_POINT('Ctrl Pts',(4.69490033250359,-4.87685035589351,138.441230318776));
#42874=CARTESIAN_POINT('Ctrl Pts',(4.82519138426705,-4.74798863987478,138.449864937488));
#42875=CARTESIAN_POINT('Ctrl Pts',(4.95013382671809,-4.61394235958592,138.458499556201));
#42876=CARTESIAN_POINT('Ctrl Pts',(5.07948875087282,-4.47516208540662,138.467439116103));
#42877=CARTESIAN_POINT('Ctrl Pts',(5.20311011490759,-4.33082453966867,138.476378676005));
#42878=CARTESIAN_POINT('Ctrl Pts',(5.32052523390524,-4.18142323083632,138.485318235908));
#42879=CARTESIAN_POINT('Ctrl Pts',(5.43362038505844,-4.03751873413159,138.493928889178));
#42880=CARTESIAN_POINT('Ctrl Pts',(5.54095757740913,-3.88891668735461,138.502539542449));
#42881=CARTESIAN_POINT('Ctrl Pts',(5.64215238935616,-3.73609494195244,138.511150195719));
#42882=CARTESIAN_POINT('Ctrl Pts',(5.74325141364355,-3.58341785255637,138.51975269843));
#42883=CARTESIAN_POINT('Ctrl Pts',(5.83821948159534,-3.42652928140618,138.528355201141));
#42884=CARTESIAN_POINT('Ctrl Pts',(5.92671367097066,-3.26593846579043,138.536957703852));
#42885=CARTESIAN_POINT('Ctrl Pts',(6.01510826191704,-3.10552839190528,138.54555052462));
#42886=CARTESIAN_POINT('Ctrl Pts',(6.09704336319448,-2.94142465275138,138.554143345387));
#42887=CARTESIAN_POINT('Ctrl Pts',(6.172220347804,-2.77416383405058,138.562736166155));
#42888=CARTESIAN_POINT('Ctrl Pts',(6.18108029691207,-2.75445138682809,138.563748869113));
#42889=CARTESIAN_POINT('Ctrl Pts',(6.18984642887871,-2.73469511937173,138.564761572071));
#42890=CARTESIAN_POINT('Ctrl Pts',(6.19851829608991,-2.71489593410845,138.565774275029));
#42891=CARTESIAN_POINT('Ctrl Pts',(6.27212026727549,-2.5468514948022,138.574369532789));
#42892=CARTESIAN_POINT('Ctrl Pts',(6.33884127528107,-2.3759112722682,138.582964790549));
#42893=CARTESIAN_POINT('Ctrl Pts',(6.39848336877615,-2.20265739040257,138.591560048309));
#42894=CARTESIAN_POINT('Ctrl Pts',(6.45818131456241,-2.02924126362413,138.600163355164));
#42895=CARTESIAN_POINT('Ctrl Pts',(6.51078701450223,-1.85350744152906,138.608766662018));
#42896=CARTESIAN_POINT('Ctrl Pts',(6.55615266914944,-1.67605226016515,138.617369968872));
#42897=CARTESIAN_POINT('Ctrl Pts',(6.6033991995701,-1.49123972544446,138.626329971812));
#42898=CARTESIAN_POINT('Ctrl Pts',(6.64279246110562,-1.30456042620896,138.635289974752));
#42899=CARTESIAN_POINT('Ctrl Pts',(6.67422477828092,-1.11669718768384,138.644249977692));
#42900=CARTESIAN_POINT('Ctrl Pts',(6.70448834779617,-0.935819266824322,
138.652876820897));
#42901=CARTESIAN_POINT('Ctrl Pts',(6.72737233016089,-0.753844163263907,
138.661503664102));
#42902=CARTESIAN_POINT('Ctrl Pts',(6.74283385906733,-0.571384764423357,
138.670130507306));
#42903=CARTESIAN_POINT('Ctrl Pts',(6.75831016528702,-0.388750980520001,
138.678765595593));
#42904=CARTESIAN_POINT('Ctrl Pts',(6.76634984139253,-0.205632281804545,
138.687400683879));
#42905=CARTESIAN_POINT('Ctrl Pts',(6.76696212040592,-0.0226420182733682,
138.696035772165));
#42906=CARTESIAN_POINT('Ctrl Pts',(6.76757530877651,0.160620022521937,138.70468368529));
#42907=CARTESIAN_POINT('Ctrl Pts',(6.76073906296994,0.343752942058419,138.713331598415));
#42908=CARTESIAN_POINT('Ctrl Pts',(6.74651456775601,0.526146545228584,138.72197951154));
#42909=CARTESIAN_POINT('Ctrl Pts',(6.74491879593467,0.546608330898569,138.722949675744));
#42910=CARTESIAN_POINT('Ctrl Pts',(6.74323009309983,0.567060820849754,138.723919839948));
#42911=CARTESIAN_POINT('Ctrl Pts',(6.74144858588057,0.587503160781988,138.724890004153));
#42912=CARTESIAN_POINT('Ctrl Pts',(6.72634565188616,0.760805467587939,138.733114683671));
#42913=CARTESIAN_POINT('Ctrl Pts',(6.70453590366463,0.933753406765605,138.74133936319));
#42914=CARTESIAN_POINT('Ctrl Pts',(6.67604077222952,1.10578868122673,138.749564042709));
#42915=CARTESIAN_POINT('Ctrl Pts',(6.64757559240127,1.27764312715159,138.757780077159));
#42916=CARTESIAN_POINT('Ctrl Pts',(6.61243908087821,1.44858646800505,138.765996111609));
#42917=CARTESIAN_POINT('Ctrl Pts',(6.57070455705608,1.61806385037256,138.774212146059));
#42918=CARTESIAN_POINT('Ctrl Pts',(6.52900554144138,1.78739703945603,138.782421190214));
#42919=CARTESIAN_POINT('Ctrl Pts',(6.48071977902235,1.95526640804378,138.790630234369));
#42920=CARTESIAN_POINT('Ctrl Pts',(6.42597194211774,2.12112555005959,138.798839278523));
#42921=CARTESIAN_POINT('Ctrl Pts',(6.37125972230467,2.28687678972565,138.807042982151));
#42922=CARTESIAN_POINT('Ctrl Pts',(6.3100939139596,2.45062006867249,138.815246685779));
#42923=CARTESIAN_POINT('Ctrl Pts',(6.24264951638908,2.61182235527747,138.823450389408));
#42924=CARTESIAN_POINT('Ctrl Pts',(6.17523549319343,2.77295204254347,138.831650398402));
#42925=CARTESIAN_POINT('Ctrl Pts',(6.10154865225163,2.93154268739914,138.839850407395));
#42926=CARTESIAN_POINT('Ctrl Pts',(6.021812813575,3.08707943504277,138.848050416389));
#42927=CARTESIAN_POINT('Ctrl Pts',(5.94208335074426,3.24260374563989,138.856249769693));
#42928=CARTESIAN_POINT('Ctrl Pts',(5.85630600922196,3.3950743227376,138.864449122997));
#42929=CARTESIAN_POINT('Ctrl Pts',(5.76475160007908,3.54399886983415,138.872648476301));
#42930=CARTESIAN_POINT('Ctrl Pts',(5.67319778784387,3.69292244598668,138.880847776148));
#42931=CARTESIAN_POINT('Ctrl Pts',(5.5758671698464,3.83829973220239,138.889047075995));
#42932=CARTESIAN_POINT('Ctrl Pts',(5.47307505995551,3.97966561259774,138.897246375841));
#42933=CARTESIAN_POINT('Ctrl Pts',(5.37026497274139,4.12105621648725,138.905447109664));
#42934=CARTESIAN_POINT('Ctrl Pts',(5.26199170148207,4.25843372685605,138.913647843487));
#42935=CARTESIAN_POINT('Ctrl Pts',(5.14861221183529,4.39136439983527,138.92184857731));
#42936=CARTESIAN_POINT('Ctrl Pts',(5.03519232486205,4.52434243626452,138.93005223307));
#42937=CARTESIAN_POINT('Ctrl Pts',(4.91666282776165,4.65287020646299,138.93825588883));
#42938=CARTESIAN_POINT('Ctrl Pts',(4.79341908311819,4.77654922445047,138.94645954459));
#42939=CARTESIAN_POINT('Ctrl Pts',(4.67003415484269,4.90036992470359,138.954672598165));
#42940=CARTESIAN_POINT('Ctrl Pts',(4.54192444304752,5.01933052138917,138.96288565174));
#42941=CARTESIAN_POINT('Ctrl Pts',(4.4095208755519,5.13307068411024,138.971098705315));
#42942=CARTESIAN_POINT('Ctrl Pts',(4.27703896189472,5.24687814943753,138.979316618739));
#42943=CARTESIAN_POINT('Ctrl Pts',(4.1402584081641,5.35545880063626,138.987534532162));
#42944=CARTESIAN_POINT('Ctrl Pts',(3.99964084713923,5.45849448968261,138.995752445585));
#42945=CARTESIAN_POINT('Ctrl Pts',(3.85880397015197,5.5616908796481,139.003983176181));
#42946=CARTESIAN_POINT('Ctrl Pts',(3.71411842340981,5.65932482410708,139.012213906777));
#42947=CARTESIAN_POINT('Ctrl Pts',(3.56607341546888,5.75112244657389,139.020444637373));
#42948=CARTESIAN_POINT('Ctrl Pts',(3.43011178152382,5.83542758402129,139.028003579048));
#42949=CARTESIAN_POINT('Ctrl Pts',(3.2913171798409,5.91481066982111,139.035562520724));
#42950=CARTESIAN_POINT('Ctrl Pts',(3.15008384884486,5.98909515246225,139.0431214624));
#42951=CARTESIAN_POINT('Ctrl Pts',(3.13315510240313,5.99799916373436,139.044027504947));
#42952=CARTESIAN_POINT('Ctrl Pts',(3.11618552915106,6.00683301543969,139.044933547494));
#42953=CARTESIAN_POINT('Ctrl Pts',(3.09917575053254,6.01559628526642,139.045839590042));
#42954=CARTESIAN_POINT('Ctrl Pts',(3.09917575053248,6.01559628526645,137.045751582743));
#42955=CARTESIAN_POINT('Ctrl Pts',(2.93382384459259,6.10078395293762,137.054501030655));
#42956=CARTESIAN_POINT('Ctrl Pts',(2.76495772122983,6.17915010267049,137.063250478567));
#42957=CARTESIAN_POINT('Ctrl Pts',(2.59315093316716,6.25042856433175,137.07199992648));
#42958=CARTESIAN_POINT('Ctrl Pts',(2.42134553245626,6.32170645041447,137.08074930374));
#42959=CARTESIAN_POINT('Ctrl Pts',(2.24659977927604,6.38589665313452,137.089498681));
#42960=CARTESIAN_POINT('Ctrl Pts',(2.06950718689937,6.44278115439069,137.09824805826));
#42961=CARTESIAN_POINT('Ctrl Pts',(1.89241596572871,6.49966521519721,137.106997367774));
#42962=CARTESIAN_POINT('Ctrl Pts',(1.712978214572,6.54924360009546,137.115746677289));
#42963=CARTESIAN_POINT('Ctrl Pts',(1.53180337335838,6.59134792173557,137.124495986804));
#42964=CARTESIAN_POINT('Ctrl Pts',(1.35062987477788,6.63345193135303,137.13324523148));
#42965=CARTESIAN_POINT('Ctrl Pts',(1.16771959102968,6.66808192368235,137.141994476156));
#42966=CARTESIAN_POINT('Ctrl Pts',(0.983693746907124,6.69512028363164,137.150743720832));
#42967=CARTESIAN_POINT('Ctrl Pts',(0.799669205420131,6.72215845218864,137.159492903576));
#42968=CARTESIAN_POINT('Ctrl Pts',(0.614529402873715,6.74160505424577,137.16824208632));
#42969=CARTESIAN_POINT('Ctrl Pts',(0.428903127363467,6.75339404354121,137.176991269065));
#42970=CARTESIAN_POINT('Ctrl Pts',(0.243278104163973,6.7651829533033,137.185740392783));
#42971=CARTESIAN_POINT('Ctrl Pts',(0.0571669005390867,6.76931433552276,
137.194489516502));
#42972=CARTESIAN_POINT('Ctrl Pts',(-0.128798404777669,6.76577415902473,
137.20323864022));
#42973=CARTESIAN_POINT('Ctrl Pts',(-0.314762517259109,6.76223400523441,
137.21198770782));
#42974=CARTESIAN_POINT('Ctrl Pts',(-0.500580446819374,6.7510223966509,137.220736775419));
#42975=CARTESIAN_POINT('Ctrl Pts',(-0.685621118842331,6.732177410125,137.229485843018));
#42976=CARTESIAN_POINT('Ctrl Pts',(-0.870660665414054,6.71333253821777,
137.238234857404));
#42977=CARTESIAN_POINT('Ctrl Pts',(-1.05492267885428,6.68685441030621,137.24698387179));
#42978=CARTESIAN_POINT('Ctrl Pts',(-1.23778137635178,6.65283295028191,137.255732886175));
#42979=CARTESIAN_POINT('Ctrl Pts',(-1.4299992297876,6.61707018861884,137.264929696543));
#42980=CARTESIAN_POINT('Ctrl Pts',(-1.62066601233596,6.57297172934437,137.27412650691));
#42981=CARTESIAN_POINT('Ctrl Pts',(-1.80906628500274,6.52070304311325,137.283323317278));
#42982=CARTESIAN_POINT('Ctrl Pts',(-1.98831342545419,6.47097374915064,137.292073315015));
#42983=CARTESIAN_POINT('Ctrl Pts',(-2.16550875896596,6.41384933989564,137.300823312753));
#42984=CARTESIAN_POINT('Ctrl Pts',(-2.34005036713908,6.34952386240514,137.309573310491));
#42985=CARTESIAN_POINT('Ctrl Pts',(-2.51458843546987,6.28519968948637,137.318323130772));
#42986=CARTESIAN_POINT('Ctrl Pts',(-2.68647261717955,6.21367483971142,137.327072951053));
#42987=CARTESIAN_POINT('Ctrl Pts',(-2.85511905908633,6.1351922674389,137.335822771333));
#42988=CARTESIAN_POINT('Ctrl Pts',(-3.02376230488794,6.05671118252982,137.344572425792));
#42989=CARTESIAN_POINT('Ctrl Pts',(-3.18916767379822,5.97127275992677,137.35332208025));
#42990=CARTESIAN_POINT('Ctrl Pts',(-3.35077334102712,5.87916720438039,137.362071734709));
#42991=CARTESIAN_POINT('Ctrl Pts',(-3.51237616037281,5.78706327195695,137.370821234977));
#42992=CARTESIAN_POINT('Ctrl Pts',(-3.67017916302202,5.68829258362361,137.379570735246));
#42993=CARTESIAN_POINT('Ctrl Pts',(-3.82364636566355,5.58319061741116,137.388320235514));
#42994=CARTESIAN_POINT('Ctrl Pts',(-3.97711106778689,5.47809036367781,137.397069593223));
#42995=CARTESIAN_POINT('Ctrl Pts',(-4.12623987481817,5.3666592004331,137.405818950931));
#42996=CARTESIAN_POINT('Ctrl Pts',(-4.27052628213818,5.24927559512425,137.41456830864));
#42997=CARTESIAN_POINT('Ctrl Pts',(-4.41481053024877,5.13189374643124,137.423317535416));
#42998=CARTESIAN_POINT('Ctrl Pts',(-4.55425230136438,5.00855981477437,137.432066762193));
#42999=CARTESIAN_POINT('Ctrl Pts',(-4.68837800630465,4.87969268192156,137.440815988969));
#43000=CARTESIAN_POINT('Ctrl Pts',(-4.8225018822883,4.75082730631876,137.44956509644));
#43001=CARTESIAN_POINT('Ctrl Pts',(-4.95130963052918,4.61642907903578,137.458314203911));
#43002=CARTESIAN_POINT('Ctrl Pts',(-5.07436379033335,4.47695444731725,137.467063311382));
#43003=CARTESIAN_POINT('Ctrl Pts',(-5.19741643562774,4.33748153220623,137.475812311171));
#43004=CARTESIAN_POINT('Ctrl Pts',(-5.31471544462743,4.19293255254628,137.484561310961));
#43005=CARTESIAN_POINT('Ctrl Pts',(-5.42586245275597,4.04379841779643,137.493310310751));
#43006=CARTESIAN_POINT('Ctrl Pts',(-5.53702160019118,3.89464799484392,137.502060266093));
#43007=CARTESIAN_POINT('Ctrl Pts',(-5.64202723081213,3.74091164443907,137.510810221435));
#43008=CARTESIAN_POINT('Ctrl Pts',(-5.74052265232925,3.58311159163299,137.519560176777));
#43009=CARTESIAN_POINT('Ctrl Pts',(-5.83901427066878,3.42531763191851,137.52830979426));
#43010=CARTESIAN_POINT('Ctrl Pts',(-5.93099603115702,3.26346052695681,137.537059411742));
#43011=CARTESIAN_POINT('Ctrl Pts',(-6.01615550622718,3.09809004467146,137.545809029225));
#43012=CARTESIAN_POINT('Ctrl Pts',(-6.10131214578762,2.93272506863905,137.554558355376));
#43013=CARTESIAN_POINT('Ctrl Pts',(-6.17964682328709,2.7638472041698,137.563307681527));
#43014=CARTESIAN_POINT('Ctrl Pts',(-6.25089348288525,2.59203002791687,137.572057007678));
#43015=CARTESIAN_POINT('Ctrl Pts',(-6.32213814889304,2.42021765937099,137.58080608901));
#43016=CARTESIAN_POINT('Ctrl Pts',(-6.3862950841257,2.24546640831963,137.589555170341));
#43017=CARTESIAN_POINT('Ctrl Pts',(-6.44314639819805,2.06836976660061,137.598304251673));
#43018=CARTESIAN_POINT('Ctrl Pts',(-6.50000285283698,1.89125711158286,137.607054124107));
#43019=CARTESIAN_POINT('Ctrl Pts',(-6.5495522767325,1.71179891440255,137.615803996542));
#43020=CARTESIAN_POINT('Ctrl Pts',(-6.59162635926387,1.53060476278421,137.624553868976));
#43021=CARTESIAN_POINT('Ctrl Pts',(-6.63369752055196,1.34942319164695,137.633303133899));
#43022=CARTESIAN_POINT('Ctrl Pts',(-6.66829431424252,1.16650618642713,137.642052398821));
#43023=CARTESIAN_POINT('Ctrl Pts',(-6.69529923745415,0.982474997618747,
137.650801663743));
#43024=CARTESIAN_POINT('Ctrl Pts',(-6.72230554731441,0.798434359177943,
137.659551377923));
#43025=CARTESIAN_POINT('Ctrl Pts',(-6.74171916496701,0.613279706240553,
137.668301092103));
#43026=CARTESIAN_POINT('Ctrl Pts',(-6.75347414817274,0.427639953655605,
137.677050806283));
#43027=CARTESIAN_POINT('Ctrl Pts',(-6.7624883775873,0.285283364200971,137.683760465458));
#43028=CARTESIAN_POINT('Ctrl Pts',(-6.76699999999983,0.142641701109694,
137.690470124634));
#43029=CARTESIAN_POINT('Ctrl Pts',(-6.767,8.32090660346834E-12,137.69717978381));
#43030=CARTESIAN_POINT('',(-6.76699997222249,0.000613140130776506,137.302820216215));
#43031=CARTESIAN_POINT('Ctrl Pts',(3.0991757505325,6.01559628526643,136.651412426306));
#43032=CARTESIAN_POINT('Ctrl Pts',(3.07449030807931,6.02831398123773,136.652724932637));
#43033=CARTESIAN_POINT('Ctrl Pts',(3.04972988437511,6.04087802633221,136.654037438968));
#43034=CARTESIAN_POINT('Ctrl Pts',(3.02489644499519,6.05328757759413,136.655349945299));
#43035=CARTESIAN_POINT('Ctrl Pts',(2.86925552937279,6.1310631080521,136.663575937841));
#43036=CARTESIAN_POINT('Ctrl Pts',(2.71040878682656,6.2029341524034,136.671801930382));
#43037=CARTESIAN_POINT('Ctrl Pts',(2.54884354114607,6.26862709073988,136.680027922924));
#43038=CARTESIAN_POINT('Ctrl Pts',(2.38744767574249,6.33425115852169,136.688245291575));
#43039=CARTESIAN_POINT('Ctrl Pts',(2.22333931178423,6.39370988444081,136.696462660226));
#43040=CARTESIAN_POINT('Ctrl Pts',(2.05702995467596,6.44677568754845,136.704680028878));
#43041=CARTESIAN_POINT('Ctrl Pts',(1.89086167365069,6.49979647625779,136.71289042694));
#43042=CARTESIAN_POINT('Ctrl Pts',(1.72249645736861,6.54643503440276,136.721100825003));
#43043=CARTESIAN_POINT('Ctrl Pts',(1.55246544864081,6.58651197757785,136.729311223065));
#43044=CARTESIAN_POINT('Ctrl Pts',(1.38254466009271,6.62656294144534,136.737516298854));
#43045=CARTESIAN_POINT('Ctrl Pts',(1.21096057751938,6.66006068105089,136.745721374643));
#43046=CARTESIAN_POINT('Ctrl Pts',(1.03825924602322,6.68687570828465,136.753926450431));
#43047=CARTESIAN_POINT('Ctrl Pts',(0.865635325669229,6.71367871602865,136.762127848401));
#43048=CARTESIAN_POINT('Ctrl Pts',(0.691895507423722,6.73380492433716,136.77032924637));
#43049=CARTESIAN_POINT('Ctrl Pts',(0.517595858989442,6.7471759667847,136.77853064434));
#43050=CARTESIAN_POINT('Ctrl Pts',(0.343309863154941,6.76054596190086,136.786731399908));
#43051=CARTESIAN_POINT('Ctrl Pts',(0.168464480763489,6.76716180902418,136.794932155475));
#43052=CARTESIAN_POINT('Ctrl Pts',(-0.00637888808444536,6.76699699348144,
136.803132911043));
#43053=CARTESIAN_POINT('Ctrl Pts',(-0.181221368811281,6.76683217877588,
136.811333624955));
#43054=CARTESIAN_POINT('Ctrl Pts',(-0.356061477640533,6.75988676928104,
136.819534338867));
#43055=CARTESIAN_POINT('Ctrl Pts',(-0.530337721449143,6.74618639686217,
136.827735052778));
#43056=CARTESIAN_POINT('Ctrl Pts',(-0.704644663212336,6.73248361118603,
136.835937211208));
#43057=CARTESIAN_POINT('Ctrl Pts',(-0.878387184796682,6.71202352008909,
136.844139369638));
#43058=CARTESIAN_POINT('Ctrl Pts',(-1.05100876161048,6.68488366263902,136.852341528067));
#43059=CARTESIAN_POINT('Ctrl Pts',(-1.2236920285752,6.65773410615866,136.86054661772));
#43060=CARTESIAN_POINT('Ctrl Pts',(-1.3952531989625,6.62390008358326,136.868751707373));
#43061=CARTESIAN_POINT('Ctrl Pts',(-1.56514572896263,6.58351029824592,136.876956797026));
#43062=CARTESIAN_POINT('Ctrl Pts',(-1.73523234109187,6.54307437235411,136.885171260024));
#43063=CARTESIAN_POINT('Ctrl Pts',(-1.90364615552444,6.49606780460035,136.893385723022));
#43064=CARTESIAN_POINT('Ctrl Pts',(-2.06985456410139,6.44266956187175,136.901600186019));
#43065=CARTESIAN_POINT('Ctrl Pts',(-2.23616144590738,6.38923968237198,136.909819515827));
#43066=CARTESIAN_POINT('Ctrl Pts',(-2.40025998110839,6.32941070176852,136.918038845634));
#43067=CARTESIAN_POINT('Ctrl Pts',(-2.56163746254934,6.26340981498606,136.926258175442));
#43068=CARTESIAN_POINT('Ctrl Pts',(-2.72326498861374,6.19730666383107,136.934490240602));
#43069=CARTESIAN_POINT('Ctrl Pts',(-2.88216270952051,6.12501264421115,136.942722305763));
#43070=CARTESIAN_POINT('Ctrl Pts',(-3.03784124961139,6.04680159606378,136.950954370924));
#43071=CARTESIAN_POINT('Ctrl Pts',(-3.17777629977712,5.97649989012777,136.958353942185));
#43072=CARTESIAN_POINT('Ctrl Pts',(-3.31511053933854,5.90141810395166,136.965753513446));
#43073=CARTESIAN_POINT('Ctrl Pts',(-3.44950926018174,5.82178450854379,136.973153084707));
#43074=CARTESIAN_POINT('Ctrl Pts',(-3.59763719071756,5.73401611599594,136.981308543114));
#43075=CARTESIAN_POINT('Ctrl Pts',(-3.74265481063443,5.64044748463279,136.989464001521));
#43076=CARTESIAN_POINT('Ctrl Pts',(-3.88407107074503,5.54132483413503,136.997619459927));
#43077=CARTESIAN_POINT('Ctrl Pts',(-4.0253152086782,5.44232282893239,137.005764992069));
#43078=CARTESIAN_POINT('Ctrl Pts',(-4.16296641600805,5.33778046811054,137.013910524211));
#43079=CARTESIAN_POINT('Ctrl Pts',(-4.29655805699752,5.22798984915328,137.022056056353));
#43080=CARTESIAN_POINT('Ctrl Pts',(-4.43001519104161,5.11830977304643,137.030193387154));
#43081=CARTESIAN_POINT('Ctrl Pts',(-4.55942061573056,5.00339218907516,137.038330717954));
#43082=CARTESIAN_POINT('Ctrl Pts',(-4.68433653653444,4.88357248461498,137.046468048755));
#43083=CARTESIAN_POINT('Ctrl Pts',(-4.80915293702246,4.76384824032318,137.054598896557));
#43084=CARTESIAN_POINT('Ctrl Pts',(-4.92948669289416,4.63922990373686,137.062729744359));
#43085=CARTESIAN_POINT('Ctrl Pts',(-5.04493299719119,4.51009313139446,137.070860592161));
#43086=CARTESIAN_POINT('Ctrl Pts',(-5.16031157709498,4.38103211469973,137.078986670155));
#43087=CARTESIAN_POINT('Ctrl Pts',(-5.27080817226869,4.24745821278198,137.087112748148));
#43088=CARTESIAN_POINT('Ctrl Pts',(-5.37605478581504,4.10978392861659,137.095238826142));
#43089=CARTESIAN_POINT('Ctrl Pts',(-5.48167458463072,3.97162147658447,137.103393717724));
#43090=CARTESIAN_POINT('Ctrl Pts',(-5.58200683845017,3.82932977235232,137.111548609306));
#43091=CARTESIAN_POINT('Ctrl Pts',(-5.67672003015765,3.68335970266372,137.119703500889));
#43092=CARTESIAN_POINT('Ctrl Pts',(-5.7710638735329,3.53795886521006,137.127826591245));
#43093=CARTESIAN_POINT('Ctrl Pts',(-5.85983221476445,3.38890861778875,137.135949681601));
#43094=CARTESIAN_POINT('Ctrl Pts',(-5.94274068696559,3.23668381642133,137.144072771957));
#43095=CARTESIAN_POINT('Ctrl Pts',(-6.02565566951855,3.08444706166741,137.152196500176));
#43096=CARTESIAN_POINT('Ctrl Pts',(-6.10270969147033,2.92903557768013,137.160320228394));
#43097=CARTESIAN_POINT('Ctrl Pts',(-6.17366436725664,2.77094880509649,137.168443956613));
#43098=CARTESIAN_POINT('Ctrl Pts',(-6.24463811377077,2.61281954299714,137.176569868273));
#43099=CARTESIAN_POINT('Ctrl Pts',(-6.30950910014755,2.45201389415588,137.184695779933));
#43100=CARTESIAN_POINT('Ctrl Pts',(-6.3680871204253,2.28905120665165,137.192821691594));
#43101=CARTESIAN_POINT('Ctrl Pts',(-6.42703975323206,2.12504635582046,137.200999569304));
#43102=CARTESIAN_POINT('Ctrl Pts',(-6.47961852516843,1.95885713505044,137.209177447014));
#43103=CARTESIAN_POINT('Ctrl Pts',(-6.52568076147207,1.79102752612945,137.217355324724));
#43104=CARTESIAN_POINT('Ctrl Pts',(-6.57152315271205,1.62399893153206,137.225494171198));
#43105=CARTESIAN_POINT('Ctrl Pts',(-6.61091105274013,1.45534594316093,137.233633017671));
#43106=CARTESIAN_POINT('Ctrl Pts',(-6.64375543029131,1.28561377655762,137.241771864144));
#43107=CARTESIAN_POINT('Ctrl Pts',(-6.67683607412608,1.11466064030292,137.249969257473));
#43108=CARTESIAN_POINT('Ctrl Pts',(-6.7032786414045,0.942613114501291,137.258166650801));
#43109=CARTESIAN_POINT('Ctrl Pts',(-6.72304544005497,0.770031824638522,
137.26636404413));
#43110=CARTESIAN_POINT('Ctrl Pts',(-6.74281223870545,0.597450534775627,
137.274561437458));
#43111=CARTESIAN_POINT('Ctrl Pts',(-6.75590330159673,0.424335856632697,
137.282758830787));
#43112=CARTESIAN_POINT('Ctrl Pts',(-6.76233423306537,0.251246333927945,
137.290956224115));
#43113=CARTESIAN_POINT('Ctrl Pts',(-6.7654367038518,0.167742849207789,137.29491088814));
#43114=CARTESIAN_POINT('Ctrl Pts',(-6.76699239991745,0.0841857874934056,
137.298865552165));
#43115=CARTESIAN_POINT('Ctrl Pts',(-6.76699997222244,0.000613140658257255,
137.30282021619));
#43116=CARTESIAN_POINT('Ctrl Pts',(-6.76699997222249,0.000613140130961323,
137.302820216215));
#43117=CARTESIAN_POINT('Ctrl Pts',(-6.76701562449587,-0.172135189647376,
137.310994680361));
#43118=CARTESIAN_POINT('Ctrl Pts',(-6.7604121071467,-0.345139132386608,
137.319169144507));
#43119=CARTESIAN_POINT('Ctrl Pts',(-6.74715665970798,-0.517847476925649,
137.327343608653));
#43120=CARTESIAN_POINT('Ctrl Pts',(-6.73391603079622,-0.69036274738927,
137.335508934404));
#43121=CARTESIAN_POINT('Ctrl Pts',(-6.71403830402876,-0.862582718275997,
137.343674260155));
#43122=CARTESIAN_POINT('Ctrl Pts',(-6.68754268485469,-1.03395446623465,
137.351839585906));
#43123=CARTESIAN_POINT('Ctrl Pts',(-6.66107118090542,-1.20517023866385,
137.359997479913));
#43124=CARTESIAN_POINT('Ctrl Pts',(-6.62799383308207,-1.37553896817054,
137.368155373919));
#43125=CARTESIAN_POINT('Ctrl Pts',(-6.58838177335109,-1.54451112283959,
137.376313267926));
#43126=CARTESIAN_POINT('Ctrl Pts',(-6.54879754047434,-1.71336457720498,
137.384465431139));
#43127=CARTESIAN_POINT('Ctrl Pts',(-6.50268782024288,-1.88082305774971,
137.392617594353));
#43128=CARTESIAN_POINT('Ctrl Pts',(-6.45017512153973,-2.04634549904702,
137.400769757566));
#43129=CARTESIAN_POINT('Ctrl Pts',(-6.39768840969953,-2.21178602855718,
137.408917886533));
#43130=CARTESIAN_POINT('Ctrl Pts',(-6.33880514060618,-2.37529208122676,
137.4170660155));
#43131=CARTESIAN_POINT('Ctrl Pts',(-6.27369814580787,-2.53633605330344,
137.425214144468));
#43132=CARTESIAN_POINT('Ctrl Pts',(-6.20860080580003,-2.69735614398595,
137.43336106514));
#43133=CARTESIAN_POINT('Ctrl Pts',(-6.13728170805753,-2.85591454168801,
137.441507985812));
#43134=CARTESIAN_POINT('Ctrl Pts',(-6.05996255435189,-3.01150175823508,
137.449654906484));
#43135=CARTESIAN_POINT('Ctrl Pts',(-5.98264609294616,-3.16708355714072,
137.457801543475));
#43136=CARTESIAN_POINT('Ctrl Pts',(-5.89933015289816,-3.31969405475827,
137.465948180466));
#43137=CARTESIAN_POINT('Ctrl Pts',(-5.81028324683367,-3.4688467235616,137.474094817457));
#43138=CARTESIAN_POINT('Ctrl Pts',(-5.72122269490448,-3.61802224905055,
137.482242702868));
#43139=CARTESIAN_POINT('Ctrl Pts',(-5.62642961453309,-3.76373857806599,
137.490390588279));
#43140=CARTESIAN_POINT('Ctrl Pts',(-5.52621683817355,-3.90553664142166,
137.49853847369));
#43141=CARTESIAN_POINT('Ctrl Pts',(-5.42596985777076,-4.0473831024694,137.50668914009));
#43142=CARTESIAN_POINT('Ctrl Pts',(-5.32029970766465,-4.18530833783343,
137.514839806489));
#43143=CARTESIAN_POINT('Ctrl Pts',(-5.20956060664076,-4.31888495861337,
137.522990472889));
#43144=CARTESIAN_POINT('Ctrl Pts',(-5.09870503425828,-4.45260207042451,
137.531149711864));
#43145=CARTESIAN_POINT('Ctrl Pts',(-4.98277009609973,-4.58196115331192,
137.539308950838));
#43146=CARTESIAN_POINT('Ctrl Pts',(-4.86214867596418,-4.70656979687115,
137.547468189812));
#43147=CARTESIAN_POINT('Ctrl Pts',(-4.74145571725088,-4.83125234376469,
137.555632267897));
#43148=CARTESIAN_POINT('Ctrl Pts',(-4.61607100008085,-4.95117858619476,
137.563796345981));
#43149=CARTESIAN_POINT('Ctrl Pts',(-4.48642163544698,-5.06599545094479,
137.571960424066));
#43150=CARTESIAN_POINT('Ctrl Pts',(-4.35659652926539,-5.18096795157912,
137.580135568674));
#43151=CARTESIAN_POINT('Ctrl Pts',(-4.22249551110337,-5.29081701279263,
137.588310713281));
#43152=CARTESIAN_POINT('Ctrl Pts',(-4.08457661889368,-5.39523149126959,
137.596485857889));
#43153=CARTESIAN_POINT('Ctrl Pts',(-4.01555650236539,-5.44748466236354,
137.600577026434));
#43154=CARTESIAN_POINT('Ctrl Pts',(-3.94558066492359,-5.49837749322565,
137.604668194978));
#43155=CARTESIAN_POINT('Ctrl Pts',(-3.87470887583674,-5.54787528045756,
137.608759363522));
#43156=CARTESIAN_POINT('Ctrl Pts',(-3.73220543769111,-5.64740155109401,
137.616985564541));
#43157=CARTESIAN_POINT('Ctrl Pts',(-3.58566569063898,-5.74157286039979,
137.62521176556));
#43158=CARTESIAN_POINT('Ctrl Pts',(-3.43552915256106,-5.83004532074178,
137.633437966579));
#43159=CARTESIAN_POINT('Ctrl Pts',(-3.28556126124083,-5.91841840092106,
137.641654927195));
#43160=CARTESIAN_POINT('Ctrl Pts',(-3.13200493027858,-6.0011051987528,137.64987188781));
#43161=CARTESIAN_POINT('Ctrl Pts',(-2.97533060905648,-6.07780361370879,
137.658088848426));
#43162=CARTESIAN_POINT('Ctrl Pts',(-2.81880083263286,-6.15443126814163,
137.666298228228));
#43163=CARTESIAN_POINT('Ctrl Pts',(-2.6591591148915,-6.22508138578937,137.674507608029));
#43164=CARTESIAN_POINT('Ctrl Pts',(-2.49690267299663,-6.289496485537,137.682716987831));
#43165=CARTESIAN_POINT('Ctrl Pts',(-2.33476337015323,-6.3538650815921,137.690920440971));
#43166=CARTESIAN_POINT('Ctrl Pts',(-2.17001343504685,-6.41200749375973,
137.699123894112));
#43167=CARTESIAN_POINT('Ctrl Pts',(-2.00317242939371,-6.46371326855678,
137.707327347252));
#43168=CARTESIAN_POINT('Ctrl Pts',(-1.83641840466981,-6.51539208705299,
137.715526523602));
#43169=CARTESIAN_POINT('Ctrl Pts',(-1.66757582293883,-6.56064084737598,
137.723725699952));
#43170=CARTESIAN_POINT('Ctrl Pts',(-1.49718195114939,-6.59929808427779,
137.731924876302));
#43171=CARTESIAN_POINT('Ctrl Pts',(-1.32682014153861,-6.63794804723704,
137.740122509854));
#43172=CARTESIAN_POINT('Ctrl Pts',(-1.15490797131203,-6.67000887197743,
137.748320143405));
#43173=CARTESIAN_POINT('Ctrl Pts',(-0.981995822377504,-6.69536953459875,
137.756517776957));
#43174=CARTESIAN_POINT('Ctrl Pts',(-0.809096127361443,-6.72072837062995,
137.764714820077));
#43175=CARTESIAN_POINT('Ctrl Pts',(-0.635196951828904,-6.73938795269441,
137.772911863198));
#43176=CARTESIAN_POINT('Ctrl Pts',(-0.460856723997039,-6.75128877177882,
137.781108906318));
#43177=CARTESIAN_POINT('Ctrl Pts',(-0.286497366894744,-6.76319089666618,
137.789306848849));
#43178=CARTESIAN_POINT('Ctrl Pts',(-0.111697219000216,-6.76833275666487,
137.797504791381));
#43179=CARTESIAN_POINT('Ctrl Pts',(0.0629822882574094,-6.76670689710777,
137.805702733912));
#43180=CARTESIAN_POINT('Ctrl Pts',(0.237712709839843,-6.76508056365683,
137.81390306592));
#43181=CARTESIAN_POINT('Ctrl Pts',(0.412322062169648,-6.75668258479427,
137.822103397929));
#43182=CARTESIAN_POINT('Ctrl Pts',(0.586250982279984,-6.74155759344795,
137.830303729937));
#43183=CARTESIAN_POINT('Ctrl Pts',(0.760361183333839,-6.72641683777274,
137.838512608908));
#43184=CARTESIAN_POINT('Ctrl Pts',(0.933789177502336,-6.70453509308144,
137.846721487879));
#43185=CARTESIAN_POINT('Ctrl Pts',(1.10598177941889,-6.67600878546407,137.85493036685));
#43186=CARTESIAN_POINT('Ctrl Pts',(1.27826681831792,-6.64746716426314,137.863143652537));
#43187=CARTESIAN_POINT('Ctrl Pts',(1.44931479189869,-6.61227394150192,137.871356938224));
#43188=CARTESIAN_POINT('Ctrl Pts',(1.61858482864857,-6.57057624204062,137.879570223912));
#43189=CARTESIAN_POINT('Ctrl Pts',(1.78810248660039,-6.52881754398408,137.887795524624));
#43190=CARTESIAN_POINT('Ctrl Pts',(1.95583666532564,-6.48053545283601,137.896020825336));
#43191=CARTESIAN_POINT('Ctrl Pts',(2.12126249475715,-6.42592673692571,137.904246126048));
#43192=CARTESIAN_POINT('Ctrl Pts',(2.27087020251983,-6.37653974071551,137.911684918342));
#43193=CARTESIAN_POINT('Ctrl Pts',(2.41858997147528,-6.32197888860733,137.919123710636));
#43194=CARTESIAN_POINT('Ctrl Pts',(2.56404983685379,-6.26242264895384,137.92656250293));
#43195=CARTESIAN_POINT('Ctrl Pts',(2.72346680703007,-6.19715189364311,137.934715059143));
#43196=CARTESIAN_POINT('Ctrl Pts',(2.88063918846917,-6.12568786670864,137.942867615356));
#43197=CARTESIAN_POINT('Ctrl Pts',(3.03504581874679,-6.04820517824153,137.95102017157));
#43198=CARTESIAN_POINT('Ctrl Pts',(3.18927356522068,-5.97081225533702,137.95916328285));
#43199=CARTESIAN_POINT('Ctrl Pts',(3.34074161538607,-5.88741471313523,137.96730639413));
#43200=CARTESIAN_POINT('Ctrl Pts',(3.48894655912745,-5.79823601688934,137.975449505411));
#43201=CARTESIAN_POINT('Ctrl Pts',(3.63701096211187,-5.70914188760294,137.983584894688));
#43202=CARTESIAN_POINT('Ctrl Pts',(3.78181810807352,-5.614277705794,137.991720283965));
#43203=CARTESIAN_POINT('Ctrl Pts',(3.92288708508951,-5.5139138474987,137.999855673243));
#43204=CARTESIAN_POINT('Ctrl Pts',(4.06385193028665,-5.41362407403292,138.007985057281));
#43205=CARTESIAN_POINT('Ctrl Pts',(4.20108380432733,-5.30784291859152,138.01611444132));
#43206=CARTESIAN_POINT('Ctrl Pts',(4.33412882111483,-5.19688525580292,138.024243825359));
#43207=CARTESIAN_POINT('Ctrl Pts',(4.46710357488483,-5.08598619137742,138.032368916151));
#43208=CARTESIAN_POINT('Ctrl Pts',(4.59589559486509,-4.96991629767309,138.040494006943));
#43209=CARTESIAN_POINT('Ctrl Pts',(4.72008228381978,-4.84903209248718,138.048619097735));
#43210=CARTESIAN_POINT('Ctrl Pts',(4.8447430202892,-4.72768644608306,138.05677520376));
#43211=CARTESIAN_POINT('Ctrl Pts',(4.96476289850688,-4.6014898832583,138.064931309785));
#43212=CARTESIAN_POINT('Ctrl Pts',(5.07974981604692,-4.47084229271972,138.07308741581));
#43213=CARTESIAN_POINT('Ctrl Pts',(5.19427393203929,-4.34072053510538,138.081210694984));
#43214=CARTESIAN_POINT('Ctrl Pts',(5.30380529847201,-4.20618380314721,138.089333974157));
#43215=CARTESIAN_POINT('Ctrl Pts',(5.40799537127942,-4.06766211283832,138.09745725333));
#43216=CARTESIAN_POINT('Ctrl Pts',(5.51219931787526,-3.92912197719611,138.105581614187));
#43217=CARTESIAN_POINT('Ctrl Pts',(5.61106033427002,-3.78659611867205,138.113705975044));
#43218=CARTESIAN_POINT('Ctrl Pts',(5.70427196775197,-3.64054533249059,138.1218303359));
#43219=CARTESIAN_POINT('Ctrl Pts',(5.79751374714345,-3.49444731149926,138.129957324286));
#43220=CARTESIAN_POINT('Ctrl Pts',(5.88510230860671,-3.34482240094478,138.138084312671));
#43221=CARTESIAN_POINT('Ctrl Pts',(5.96677611970491,-3.19215784968713,138.146211301057));
#43222=CARTESIAN_POINT('Ctrl Pts',(6.04897794269357,-3.03850633948597,138.154390829497));
#43223=CARTESIAN_POINT('Ctrl Pts',(6.12518809651608,-2.88177608184259,138.162570357937));
#43224=CARTESIAN_POINT('Ctrl Pts',(6.19518864453863,-2.72248538262001,138.170749886377));
#43225=CARTESIAN_POINT('Ctrl Pts',(6.26485953741319,-2.56394483465351,138.178890894781));
#43226=CARTESIAN_POINT('Ctrl Pts',(6.32837911048866,-2.40286827257537,138.187031903184));
#43227=CARTESIAN_POINT('Ctrl Pts',(6.38558237281462,-2.23978274839307,138.195172911588));
#43228=CARTESIAN_POINT('Ctrl Pts',(6.4431916300072,-2.07553973977815,138.203371700046));
#43229=CARTESIAN_POINT('Ctrl Pts',(6.49439447691907,-1.90925950819574,138.211570488505));
#43230=CARTESIAN_POINT('Ctrl Pts',(6.5390746352727,-1.74149129034089,138.219769276963));
#43231=CARTESIAN_POINT('Ctrl Pts',(6.58375479362637,-1.57372307248591,138.227968065421));
#43232=CARTESIAN_POINT('Ctrl Pts',(6.621912244947,-1.40446724488043,138.23616685388));
#43233=CARTESIAN_POINT('Ctrl Pts',(6.65348374684837,-1.23427834398266,138.244365642338));
#43234=CARTESIAN_POINT('Ctrl Pts',(6.68518718196193,-1.06337824573845,138.25259869247));
#43235=CARTESIAN_POINT('Ctrl Pts',(6.71034817818033,-0.891006032119165,
138.260831742602));
#43236=CARTESIAN_POINT('Ctrl Pts',(6.72883277965433,-0.717703576310849,
138.269064792734));
#43237=CARTESIAN_POINT('Ctrl Pts',(6.74729536880935,-0.544607497088091,
138.277288038569));
#43238=CARTESIAN_POINT('Ctrl Pts',(6.7590973571348,-0.370583734199326,138.285511284404));
#43239=CARTESIAN_POINT('Ctrl Pts',(6.76415555074572,-0.196185334100025,
138.293734530239));
#43240=CARTESIAN_POINT('Ctrl Pts',(6.76920873323391,-0.021959709471846,
138.301949629352));
#43241=CARTESIAN_POINT('Ctrl Pts',(6.76753141606382,0.152639457644934,138.310164728466));
#43242=CARTESIAN_POINT('Ctrl Pts',(6.75909205449102,0.327052899263056,138.318379827579));
#43243=CARTESIAN_POINT('Ctrl Pts',(6.75065936519795,0.501328447124589,138.326588431718));
#43244=CARTESIAN_POINT('Ctrl Pts',(6.73547529723366,0.675418205804321,138.334797035857));
#43245=CARTESIAN_POINT('Ctrl Pts',(6.7135603500842,0.848761701408204,138.343005639996));
#43246=CARTESIAN_POINT('Ctrl Pts',(6.69165834560424,1.02200282270295,138.351209396245));
#43247=CARTESIAN_POINT('Ctrl Pts',(6.66303342581454,1.1944982045209,138.359413152494));
#43248=CARTESIAN_POINT('Ctrl Pts',(6.62775803369018,1.36569119747302,138.367616908743));
#43249=CARTESIAN_POINT('Ctrl Pts',(6.59249307866533,1.53683353873298,138.375818237707));
#43250=CARTESIAN_POINT('Ctrl Pts',(6.55058163932144,1.70667390757311,138.384019566671));
#43251=CARTESIAN_POINT('Ctrl Pts',(6.50214754427987,1.8746643199291,138.392220895635));
#43252=CARTESIAN_POINT('Ctrl Pts',(6.45372012876234,2.04263156480367,138.400421093558));
#43253=CARTESIAN_POINT('Ctrl Pts',(6.39877194756112,2.2087490169544,138.408621291481));
#43254=CARTESIAN_POINT('Ctrl Pts',(6.33747714091964,2.37248234731494,138.416821489404));
#43255=CARTESIAN_POINT('Ctrl Pts',(6.27617967955108,2.53622276909692,138.425022042484));
#43256=CARTESIAN_POINT('Ctrl Pts',(6.2085351706833,2.69757852779026,138.433222595563));
#43257=CARTESIAN_POINT('Ctrl Pts',(6.13476650800192,2.85603376946035,138.441423148643));
#43258=CARTESIAN_POINT('Ctrl Pts',(6.06098128201432,3.01452458914686,138.449625542996));
#43259=CARTESIAN_POINT('Ctrl Pts',(5.98106931466843,3.17011326995205,138.45782793735));
#43260=CARTESIAN_POINT('Ctrl Pts',(5.89530022198093,3.32230707381356,138.466030331703));
#43261=CARTESIAN_POINT('Ctrl Pts',(5.80945092011412,3.47464320563636,138.474240396737));
#43262=CARTESIAN_POINT('Ctrl Pts',(5.7177337255637,3.62357780498087,138.48245046177));
#43263=CARTESIAN_POINT('Ctrl Pts',(5.62046300289667,3.76864493327107,138.490660526804));
#43264=CARTESIAN_POINT('Ctrl Pts',(5.5231457281873,3.91378148811548,138.49887452103));
#43265=CARTESIAN_POINT('Ctrl Pts',(5.42026983690323,4.05504659204454,138.507088515255));
#43266=CARTESIAN_POINT('Ctrl Pts',(5.3121909895703,4.19200618920441,138.51530250948));
#43267=CARTESIAN_POINT('Ctrl Pts',(5.20396479477191,4.32915250791073,138.523527702115));
#43268=CARTESIAN_POINT('Ctrl Pts',(5.09052170049427,4.46198131637448,138.531752894751));
#43269=CARTESIAN_POINT('Ctrl Pts',(4.9722561607381,4.59009342737182,138.539978087386));
#43270=CARTESIAN_POINT('Ctrl Pts',(4.86590021414053,4.70530437439686,138.547374985506));
#43271=CARTESIAN_POINT('Ctrl Pts',(4.75564480751625,4.81670112120452,138.554771883625));
#43272=CARTESIAN_POINT('Ctrl Pts',(4.64179987782883,4.92402100870704,138.562168781745));
#43273=CARTESIAN_POINT('Ctrl Pts',(4.50874499689211,5.04944982572152,138.570813816718));
#43274=CARTESIAN_POINT('Ctrl Pts',(4.37048472851995,5.16959417462541,138.579458851691));
#43275=CARTESIAN_POINT('Ctrl Pts',(4.22745515641186,5.28402421460451,138.588103886664));
#43276=CARTESIAN_POINT('Ctrl Pts',(4.0845883862147,5.39832400579028,138.596739081516));
#43277=CARTESIAN_POINT('Ctrl Pts',(3.93696337097964,5.50692226462593,138.605374276369));
#43278=CARTESIAN_POINT('Ctrl Pts',(3.78505167362472,5.60942713902148,138.614009471221));
#43279=CARTESIAN_POINT('Ctrl Pts',(3.63336168653824,5.71178241082807,138.622632063283));
#43280=CARTESIAN_POINT('Ctrl Pts',(3.47739774985327,5.80806186913041,138.631254655344));
#43281=CARTESIAN_POINT('Ctrl Pts',(3.31766296943204,5.89791500627632,138.639877247406));
#43282=CARTESIAN_POINT('Ctrl Pts',(3.24558516275021,5.93845982082378,138.643768056421));
#43283=CARTESIAN_POINT('Ctrl Pts',(3.1727399991916,5.97769671143552,138.647658865436));
#43284=CARTESIAN_POINT('Ctrl Pts',(3.09917575053274,6.01559628526631,138.651549674452));
#43285=CARTESIAN_POINT('Origin',(0.,0.,-3.69717978381041));
#43286=CARTESIAN_POINT('',(3.09917575053271,6.01559628526633,141.045900408649));
#43287=CARTESIAN_POINT('',(3.09917575053259,6.01559628526639,140.651392015123));
#43288=CARTESIAN_POINT('',(3.09917575053259,6.01559628526639,-3.69717978381041));
#43289=CARTESIAN_POINT('',(-6.76699963384649,0.00222610005286933,139.69717978384));
#43290=CARTESIAN_POINT('Ctrl Pts',(-6.76699963384649,0.00222610005305866,
139.69717978384));
#43291=CARTESIAN_POINT('Ctrl Pts',(-6.76705636330936,-0.170222687206146,
139.705337466641));
#43292=CARTESIAN_POINT('Ctrl Pts',(-6.76051690289134,-0.34292831167991,
139.713495149441));
#43293=CARTESIAN_POINT('Ctrl Pts',(-6.74734854687333,-0.515341233559222,
139.721652832242));
#43294=CARTESIAN_POINT('Ctrl Pts',(-6.73419462435496,-0.687565178026157,
139.729801573614));
#43295=CARTESIAN_POINT('Ctrl Pts',(-6.71442629813685,-0.859496697719035,
139.737950314987));
#43296=CARTESIAN_POINT('Ctrl Pts',(-6.68806283453828,-1.03058455318709,
139.746099056359));
#43297=CARTESIAN_POINT('Ctrl Pts',(-6.66172273840259,-1.20152076359161,
139.75424057503));
#43298=CARTESIAN_POINT('Ctrl Pts',(-6.62879919912588,-1.37161443985086,
139.762382093702));
#43299=CARTESIAN_POINT('Ctrl Pts',(-6.58936341206318,-1.5403177671387,139.770523612373));
#43300=CARTESIAN_POINT('Ctrl Pts',(-6.54995431271802,-1.70890692638066,
139.778659621365));
#43301=CARTESIAN_POINT('Ctrl Pts',(-6.50404182458938,-1.87610725598205,
139.786795630357));
#43302=CARTESIAN_POINT('Ctrl Pts',(-6.45174851469608,-2.04137946083451,
139.794931639349));
#43303=CARTESIAN_POINT('Ctrl Pts',(-6.39741451302602,-2.21310124078667,
139.80338514759));
#43304=CARTESIAN_POINT('Ctrl Pts',(-6.33619169653277,-2.38274097428837,
139.811838655831));
#43305=CARTESIAN_POINT('Ctrl Pts',(-6.26827534944102,-2.54970844285972,
139.820292164073));
#43306=CARTESIAN_POINT('Ctrl Pts',(-6.20294787868022,-2.71031134463774,
139.828423436382));
#43307=CARTESIAN_POINT('Ctrl Pts',(-6.13142790803199,-2.8684415826166,139.836554708691));
#43308=CARTESIAN_POINT('Ctrl Pts',(-6.05393904204425,-3.02359241221636,
139.844685981001));
#43309=CARTESIAN_POINT('Ctrl Pts',(-5.97645006524831,-3.17874346368005,
139.852817264938));
#43310=CARTESIAN_POINT('Ctrl Pts',(-5.89299233890733,-3.33091477113788,
139.860948548875));
#43311=CARTESIAN_POINT('Ctrl Pts',(-5.80383613475882,-3.47962284175567,
139.869079832812));
#43312=CARTESIAN_POINT('Ctrl Pts',(-5.71466288010896,-3.62835935175335,
139.8772126718));
#43313=CARTESIAN_POINT('Ctrl Pts',(-5.61978916554424,-3.77363099275641,
139.885345510788));
#43314=CARTESIAN_POINT('Ctrl Pts',(-5.51952939717935,-3.91498202213918,
139.893478349776));
#43315=CARTESIAN_POINT('Ctrl Pts',(-5.41923142313166,-4.0563869157257,139.901614287921));
#43316=CARTESIAN_POINT('Ctrl Pts',(-5.31354351973422,-4.19386792515054,
139.909750226065));
#43317=CARTESIAN_POINT('Ctrl Pts',(-5.20282125064118,-4.32700127500288,
139.917886164209));
#43318=CARTESIAN_POINT('Ctrl Pts',(-5.09198084434003,-4.46027667398758,
139.926030783146));
#43319=CARTESIAN_POINT('Ctrl Pts',(-4.97609558074881,-4.58919487029723,
139.934175402082));
#43320=CARTESIAN_POINT('Ctrl Pts',(-4.85555938568095,-4.71336737928688,
139.942320021019));
#43321=CARTESIAN_POINT('Ctrl Pts',(-4.73494703799582,-4.83761833825205,
139.95046978558));
#43322=CARTESIAN_POINT('Ctrl Pts',(-4.6096781678019,-4.95711738489197,139.958619550142));
#43323=CARTESIAN_POINT('Ctrl Pts',(-4.48018060082227,-5.07151562987001,
139.966769314703));
#43324=CARTESIAN_POINT('Ctrl Pts',(-4.3505146868854,-5.18606259267268,139.974929673966));
#43325=CARTESIAN_POINT('Ctrl Pts',(-4.21660938297347,-5.29549528569637,
139.983090033229));
#43326=CARTESIAN_POINT('Ctrl Pts',(-4.07892293864588,-5.39950707570501,
139.991250392492));
#43327=CARTESIAN_POINT('Ctrl Pts',(-4.04199757380827,-5.42740142152997,
139.993438874041));
#43328=CARTESIAN_POINT('Ctrl Pts',(-4.0048004035001,-5.45490613153912,139.995627355591));
#43329=CARTESIAN_POINT('Ctrl Pts',(-3.96734057255745,-5.48201585015399,
139.99781583714));
#43330=CARTESIAN_POINT('Ctrl Pts',(-3.82782172928879,-5.58298578213995,
140.005966819314));
#43331=CARTESIAN_POINT('Ctrl Pts',(-3.68422662962426,-5.67878465813751,
140.014117801488));
#43332=CARTESIAN_POINT('Ctrl Pts',(-3.53697823196215,-5.76906179431508,
140.022268783663));
#43333=CARTESIAN_POINT('Ctrl Pts',(-3.38990087696121,-5.8592340652319,140.030410297716));
#43334=CARTESIAN_POINT('Ctrl Pts',(-3.23917897983449,-5.94389717472451,
140.038551811769));
#43335=CARTESIAN_POINT('Ctrl Pts',(-3.08526765853149,-6.02274127579955,
140.046693325822));
#43336=CARTESIAN_POINT('Ctrl Pts',(-2.93150273090615,-6.10151038383432,
140.054827096025));
#43337=CARTESIAN_POINT('Ctrl Pts',(-2.7745547418729,-6.17447133680736,140.062960866228));
#43338=CARTESIAN_POINT('Ctrl Pts',(-2.61490681340937,-6.24135813402702,
140.071094636431));
#43339=CARTESIAN_POINT('Ctrl Pts',(-2.45537715778601,-6.30819537913816,
140.079222380849));
#43340=CARTESIAN_POINT('Ctrl Pts',(-2.29315188133859,-6.36896728787685,
140.087350125267));
#43341=CARTESIAN_POINT('Ctrl Pts',(-2.12873767178384,-6.42345428291728,
140.095477869685));
#43342=CARTESIAN_POINT('Ctrl Pts',(-1.9644106992507,-6.4779123675419,140.103601301579));
#43343=CARTESIAN_POINT('Ctrl Pts',(-1.7978974529962,-6.52609206486806,140.111724733473));
#43344=CARTESIAN_POINT('Ctrl Pts',(-1.62972351079848,-6.56782233912814,
140.119848165367));
#43345=CARTESIAN_POINT('Ctrl Pts',(-1.46048273925821,-6.60981733383464,
140.128023129118));
#43346=CARTESIAN_POINT('Ctrl Pts',(-1.28956047779386,-6.64528065816036,
140.136198092869));
#43347=CARTESIAN_POINT('Ctrl Pts',(-1.11750723084254,-6.6740891954644,140.144373056619));
#43348=CARTESIAN_POINT('Ctrl Pts',(-0.946577324580619,-6.70270964098448,
140.152494645792));
#43349=CARTESIAN_POINT('Ctrl Pts',(-0.774531526743982,-6.72476190446661,
140.160616234965));
#43350=CARTESIAN_POINT('Ctrl Pts',(-0.601918838865556,-6.7401767566896,
140.168737824139));
#43351=CARTESIAN_POINT('Ctrl Pts',(-0.42928336257217,-6.75559364398924,
140.176860485528));
#43352=CARTESIAN_POINT('Ctrl Pts',(-0.256081211738418,-6.76437134208855,
140.184983146917));
#43353=CARTESIAN_POINT('Ctrl Pts',(-0.0828653323660814,-6.76649261705737,
140.193105808307));
#43354=CARTESIAN_POINT('Ctrl Pts',(0.0904064004816274,-6.76861457603149,
140.201231088849));
#43355=CARTESIAN_POINT('Ctrl Pts',(0.263691504913624,-6.76407583332543,
140.209356369391));
#43356=CARTESIAN_POINT('Ctrl Pts',(0.436438259753492,-6.7529112718459,140.217481649933));
#43357=CARTESIAN_POINT('Ctrl Pts',(0.611067054643416,-6.74162507478562,
140.225695453721));
#43358=CARTESIAN_POINT('Ctrl Pts',(0.785145317493713,-6.72356786403866,
140.233909257509));
#43359=CARTESIAN_POINT('Ctrl Pts',(0.95811060862046,-6.69882923066777,140.242123061297));
#43360=CARTESIAN_POINT('Ctrl Pts',(1.12950786827785,-6.67431486746914,140.250262402152));
#43361=CARTESIAN_POINT('Ctrl Pts',(1.29981190532521,-6.64323985432275,140.258401743007));
#43362=CARTESIAN_POINT('Ctrl Pts',(1.46848817947352,-6.60574231004711,140.266541083862));
#43363=CARTESIAN_POINT('Ctrl Pts',(1.6394791613353,-6.56773019515146,140.274792119116));
#43364=CARTESIAN_POINT('Ctrl Pts',(1.80879700187877,-6.52311810091999,140.283043154371));
#43365=CARTESIAN_POINT('Ctrl Pts',(1.97590363668063,-6.47210119038263,140.291294189625));
#43366=CARTESIAN_POINT('Ctrl Pts',(2.14301027148261,-6.42108427984524,140.299545224879));
#43367=CARTESIAN_POINT('Ctrl Pts',(2.30790536007158,-6.36366274257922,140.307796260133));
#43368=CARTESIAN_POINT('Ctrl Pts',(2.4700750024516,-6.30008083140714,140.316047295387));
#43369=CARTESIAN_POINT('Ctrl Pts',(2.63186603658003,-6.23664736131115,140.324279067418));
#43370=CARTESIAN_POINT('Ctrl Pts',(2.79144948368518,-6.16688438648224,140.332510839449));
#43371=CARTESIAN_POINT('Ctrl Pts',(2.94829467539587,-6.09096441518356,140.340742611479));
#43372=CARTESIAN_POINT('Ctrl Pts',(3.10495257827362,-6.01513509991752,140.348964553952));
#43373=CARTESIAN_POINT('Ctrl Pts',(3.25887841724637,-5.93316358242239,140.357186496424));
#43374=CARTESIAN_POINT('Ctrl Pts',(3.40955885309962,-5.84527137327687,140.365408438897));
#43375=CARTESIAN_POINT('Ctrl Pts',(3.56008955160476,-5.75746650623547,140.373622210887));
#43376=CARTESIAN_POINT('Ctrl Pts',(3.70738096237336,-5.66375284406863,140.381835982876));
#43377=CARTESIAN_POINT('Ctrl Pts',(3.85094175012746,-5.56439903647512,140.390049754866));
#43378=CARTESIAN_POINT('Ctrl Pts',(3.99438862883727,-5.46512406167048,140.398257009597));
#43379=CARTESIAN_POINT('Ctrl Pts',(4.13411048706786,-5.36021805805965,140.406464264327));
#43380=CARTESIAN_POINT('Ctrl Pts',(4.26964246240572,-5.2499944993516,140.414671519057));
#43381=CARTESIAN_POINT('Ctrl Pts',(4.40509403728806,-5.13983632760708,140.422873905069));
#43382=CARTESIAN_POINT('Ctrl Pts',(4.5363604035007,-5.02436711034961,140.431076291081));
#43383=CARTESIAN_POINT('Ctrl Pts',(4.66300739084778,-4.90394240105846,140.439278677093));
#43384=CARTESIAN_POINT('Ctrl Pts',(4.78961657714103,-4.78355363562206,140.447478614892));
#43385=CARTESIAN_POINT('Ctrl Pts',(4.91160886901698,-4.65821256823187,140.455678552691));
#43386=CARTESIAN_POINT('Ctrl Pts',(5.02858460541446,-4.5283137994389,140.463878490489));
#43387=CARTESIAN_POINT('Ctrl Pts',(5.14554398558485,-4.39843319384647,140.472077281725));
#43388=CARTESIAN_POINT('Ctrl Pts',(5.25748796692467,-4.26399642179446,140.480276072961));
#43389=CARTESIAN_POINT('Ctrl Pts',(5.36405506699925,-4.12543358184321,140.488474864197));
#43390=CARTESIAN_POINT('Ctrl Pts',(5.470626598068,-3.98686498053469,140.496673996333));
#43391=CARTESIAN_POINT('Ctrl Pts',(5.57182058388545,-3.84417025362486,140.50487312847));
#43392=CARTESIAN_POINT('Ctrl Pts',(5.66731699076707,-3.69781112635068,140.513072260606));
#43393=CARTESIAN_POINT('Ctrl Pts',(5.76283469181036,-3.55141936334685,140.521273221017));
#43394=CARTESIAN_POINT('Ctrl Pts',(5.85265208768857,-3.40136187266688,140.529474181428));
#43395=CARTESIAN_POINT('Ctrl Pts',(5.93649346107707,-3.24812782793246,140.537675141839));
#43396=CARTESIAN_POINT('Ctrl Pts',(6.02041341401542,-3.09475016601034,140.545883788524));
#43397=CARTESIAN_POINT('Ctrl Pts',(6.0983459817951,-2.93819031663081,140.554092435209));
#43398=CARTESIAN_POINT('Ctrl Pts',(6.17006184638328,-2.77896128289066,140.562301081894));
#43399=CARTESIAN_POINT('Ctrl Pts',(6.24181195013942,-2.61965622873774,140.570513647617));
#43400=CARTESIAN_POINT('Ctrl Pts',(6.3073392986111,-2.45767978149311,140.578726213341));
#43401=CARTESIAN_POINT('Ctrl Pts',(6.36646346716161,-2.29356314962039,140.586938779064));
#43402=CARTESIAN_POINT('Ctrl Pts',(6.42566876260306,-2.12922132604648,140.595162613613));
#43403=CARTESIAN_POINT('Ctrl Pts',(6.47845321032211,-1.96273379060594,140.603386448162));
#43404=CARTESIAN_POINT('Ctrl Pts',(6.52468648835483,-1.79464626839941,140.611610282711));
#43405=CARTESIAN_POINT('Ctrl Pts',(6.56716617397803,-1.6402054542425,140.619166439685));
#43406=CARTESIAN_POINT('Ctrl Pts',(6.60411580339929,-1.4844142516776,140.626722596659));
#43407=CARTESIAN_POINT('Ctrl Pts',(6.63547272895231,-1.32770127036553,140.634278753633));
#43408=CARTESIAN_POINT('Ctrl Pts',(6.67135117063168,-1.14839103949166,140.642924471686));
#43409=CARTESIAN_POINT('Ctrl Pts',(6.69998922023828,-0.967465284381121,
140.651570189738));
#43410=CARTESIAN_POINT('Ctrl Pts',(6.72125320686374,-0.785521692395489,
140.660215907791));
#43411=CARTESIAN_POINT('Ctrl Pts',(6.74248989486381,-0.603811678903314,
140.668850526503));
#43412=CARTESIAN_POINT('Ctrl Pts',(6.75637136192696,-0.421086735623222,
140.677485145215));
#43413=CARTESIAN_POINT('Ctrl Pts',(6.76281500291947,-0.237954273521913,
140.686119763928));
#43414=CARTESIAN_POINT('Ctrl Pts',(6.76948620828031,-0.0483542842714589,
140.69505932383));
#43415=CARTESIAN_POINT('Ctrl Pts',(6.76818455781633,0.141682223962945,140.703998883732));
#43416=CARTESIAN_POINT('Ctrl Pts',(6.75887674449614,0.331472702811677,140.712938443635));
#43417=CARTESIAN_POINT('Ctrl Pts',(6.74991138668418,0.514280360598753,140.721549096905));
#43418=CARTESIAN_POINT('Ctrl Pts',(6.73351845799152,0.696859420342741,140.730159750176));
#43419=CARTESIAN_POINT('Ctrl Pts',(6.70972102713668,0.878597028221676,140.738770403447));
#43420=CARTESIAN_POINT('Ctrl Pts',(6.68594612214232,1.0601626092955,140.747372906158));
#43421=CARTESIAN_POINT('Ctrl Pts',(6.6547807282305,1.24088802507926,140.755975408869));
#43422=CARTESIAN_POINT('Ctrl Pts',(6.61629982679463,1.4201639348883,140.76457791158));
#43423=CARTESIAN_POINT('Ctrl Pts',(6.57786223483875,1.59923807326943,140.773170732347));
#43424=CARTESIAN_POINT('Ctrl Pts',(6.5321256247305,1.77686566268429,140.781763553115));
#43425=CARTESIAN_POINT('Ctrl Pts',(6.47921635425518,1.95244575718563,140.790356373882));
#43426=CARTESIAN_POINT('Ctrl Pts',(6.47298075640211,1.97313866885272,140.791369076841));
#43427=CARTESIAN_POINT('Ctrl Pts',(6.46664559110848,1.99380315177187,140.792381779799));
#43428=CARTESIAN_POINT('Ctrl Pts',(6.46021111211851,2.0144382310859,140.793394482757));
#43429=CARTESIAN_POINT('Ctrl Pts',(6.40559884401013,2.1895772727539,140.801989740517));
#43430=CARTESIAN_POINT('Ctrl Pts',(6.34389249037932,2.36239098317935,140.810584998277));
#43431=CARTESIAN_POINT('Ctrl Pts',(6.27532428130308,2.53231004509481,140.819180256037));
#43432=CARTESIAN_POINT('Ctrl Pts',(6.20669186100719,2.70238822900503,140.827783562892));
#43433=CARTESIAN_POINT('Ctrl Pts',(6.13118487331445,2.86956607055048,140.836386869746));
#43434=CARTESIAN_POINT('Ctrl Pts',(6.04908273339191,3.03329640565835,140.8449901766));
#43435=CARTESIAN_POINT('Ctrl Pts',(5.96357661027702,3.20381505723776,140.85395017954));
#43436=CARTESIAN_POINT('Ctrl Pts',(5.87091699002684,3.37059390659366,140.86291018248));
#43437=CARTESIAN_POINT('Ctrl Pts',(5.77147029246756,3.53304679606206,140.87187018542));
#43438=CARTESIAN_POINT('Ctrl Pts',(5.67572132086355,3.68945920072163,140.880497028625));
#43439=CARTESIAN_POINT('Ctrl Pts',(5.57368110157995,3.84186132870413,140.88912387183));
#43440=CARTESIAN_POINT('Ctrl Pts',(5.46571913039019,3.98976232220502,140.897750715035));
#43441=CARTESIAN_POINT('Ctrl Pts',(5.35765397484706,4.13780467166864,140.906385803321));
#43442=CARTESIAN_POINT('Ctrl Pts',(5.24365595731899,4.28133705899291,140.915020891607));
#43443=CARTESIAN_POINT('Ctrl Pts',(5.12413421366191,4.41990243788021,140.923655979893));
#43444=CARTESIAN_POINT('Ctrl Pts',(5.0044349562296,4.55867361416278,140.932303893018));
#43445=CARTESIAN_POINT('Ctrl Pts',(4.87919578376329,4.69246281460474,140.940951806143));
#43446=CARTESIAN_POINT('Ctrl Pts',(4.74886298885342,4.82084943895763,140.949599719269));
#43447=CARTESIAN_POINT('Ctrl Pts',(4.73424163334257,4.83525246375888,140.950569883473));
#43448=CARTESIAN_POINT('Ctrl Pts',(4.71955620680024,4.84958753646979,140.951540047677));
#43449=CARTESIAN_POINT('Ctrl Pts',(4.70480736498783,4.86385409509335,140.952510211881));
#43450=CARTESIAN_POINT('Ctrl Pts',(4.57978419058098,4.98478904508226,140.960734112443));
#43451=CARTESIAN_POINT('Ctrl Pts',(4.44993041114769,5.10105975968477,140.968958013006));
#43452=CARTESIAN_POINT('Ctrl Pts',(4.31562816458559,5.21225887164439,140.977181913569));
#43453=CARTESIAN_POINT('Ctrl Pts',(4.18145070678321,5.32335466143615,140.985398172783));
#43454=CARTESIAN_POINT('Ctrl Pts',(4.04283328221031,5.42938800100551,140.993614431996));
#43455=CARTESIAN_POINT('Ctrl Pts',(3.90019509022749,5.52998799801278,141.00183069121));
#43456=CARTESIAN_POINT('Ctrl Pts',(3.75769109599703,5.63049334790417,141.010039220351));
#43457=CARTESIAN_POINT('Ctrl Pts',(3.61117416244117,5.72557533448906,141.018247749493));
#43458=CARTESIAN_POINT('Ctrl Pts',(3.46109660356837,5.81490320648311,141.026456278634));
#43459=CARTESIAN_POINT('Ctrl Pts',(3.34259678803946,5.88543564605894,141.032937655306));
#43460=CARTESIAN_POINT('Ctrl Pts',(3.22187781245033,5.95238139570221,141.039419031978));
#43461=CARTESIAN_POINT('Ctrl Pts',(3.09917575053271,6.01559628526633,141.045900408649));
#43462=CARTESIAN_POINT('Ctrl Pts',(3.09917575053254,6.01559628526642,139.045839590042));
#43463=CARTESIAN_POINT('Ctrl Pts',(2.94611930473484,6.09444945339552,139.0539922918));
#43464=CARTESIAN_POINT('Ctrl Pts',(2.78980507744459,6.16758436117791,139.062144993558));
#43465=CARTESIAN_POINT('Ctrl Pts',(2.63070295282366,6.2347165913139,139.070297695316));
#43466=CARTESIAN_POINT('Ctrl Pts',(2.4717912571062,6.30176847106487,139.078440639127));
#43467=CARTESIAN_POINT('Ctrl Pts',(2.31009863951035,6.36283183385974,139.086583582939));
#43468=CARTESIAN_POINT('Ctrl Pts',(2.14612079442815,6.41766737496757,139.09472652675));
#43469=CARTESIAN_POINT('Ctrl Pts',(1.98230470270438,6.47244882442094,139.102861438083));
#43470=CARTESIAN_POINT('Ctrl Pts',(1.81620821557681,6.52101456742517,139.110996349416));
#43471=CARTESIAN_POINT('Ctrl Pts',(1.6483482856285,6.5631727791721,139.119131260749));
#43472=CARTESIAN_POINT('Ctrl Pts',(1.4806186310235,6.60529827211883,139.127259858613));
#43473=CARTESIAN_POINT('Ctrl Pts',(1.31112861174914,6.64102604678876,139.135388456478));
#43474=CARTESIAN_POINT('Ctrl Pts',(1.14041167024186,6.67021365642632,139.143517054342));
#43475=CARTESIAN_POINT('Ctrl Pts',(0.969791327360429,6.69938475052091,139.151641052714));
#43476=CARTESIAN_POINT('Ctrl Pts',(0.797945804421077,6.72202298805287,139.159765051085));
#43477=CARTESIAN_POINT('Ctrl Pts',(0.62542009786228,6.73803670969445,139.167889049456));
#43478=CARTESIAN_POINT('Ctrl Pts',(0.452933585170598,6.75404679338727,139.176011202242));
#43479=CARTESIAN_POINT('Ctrl Pts',(0.279767559797171,6.76343531791645,139.184133355029));
#43480=CARTESIAN_POINT('Ctrl Pts',(0.106473732171504,6.76616230549914,139.192255507815));
#43481=CARTESIAN_POINT('Ctrl Pts',(-0.0668039513705443,6.76888903903519,
139.20037690394));
#43482=CARTESIAN_POINT('Ctrl Pts',(-0.24020904763952,6.7649554643749,139.208498300064));
#43483=CARTESIAN_POINT('Ctrl Pts',(-0.413188376620589,6.75437372118435,
139.216619696189));
#43484=CARTESIAN_POINT('Ctrl Pts',(-0.586184528439248,6.74379094888269,
139.224741882148));
#43485=CARTESIAN_POINT('Ctrl Pts',(-0.758754465192137,6.72655874263071,
139.232864068107));
#43486=CARTESIAN_POINT('Ctrl Pts',(-0.930348706431284,6.70274125149119,
139.240986254066));
#43487=CARTESIAN_POINT('Ctrl Pts',(-1.10199231154012,6.67891690858601,139.249110776598));
#43488=CARTESIAN_POINT('Ctrl Pts',(-1.27265929991497,6.64850355893192,139.25723529913));
#43489=CARTESIAN_POINT('Ctrl Pts',(-1.44180902181761,6.61161672698935,139.265359821662));
#43490=CARTESIAN_POINT('Ctrl Pts',(-1.61113948018845,6.57469048146895,139.273493025246));
#43491=CARTESIAN_POINT('Ctrl Pts',(-1.77894907559217,6.53127701429676,139.28162622883));
#43492=CARTESIAN_POINT('Ctrl Pts',(-1.94471009998545,6.48154238025291,139.289759432414));
#43493=CARTESIAN_POINT('Ctrl Pts',(-2.1105619282766,6.43178050157393,139.297897091367));
#43494=CARTESIAN_POINT('Ctrl Pts',(-2.27436260371014,6.37569067426807,139.30603475032));
#43495=CARTESIAN_POINT('Ctrl Pts',(-2.4356034118258,6.31348754812287,139.314172409274));
#43496=CARTESIAN_POINT('Ctrl Pts',(-2.59708947912999,6.25118980642457,139.322322446208));
#43497=CARTESIAN_POINT('Ctrl Pts',(-2.75600756303741,6.18276033018469,139.330472483142));
#43498=CARTESIAN_POINT('Ctrl Pts',(-2.91187150330822,6.10846080025251,139.338622520076));
#43499=CARTESIAN_POINT('Ctrl Pts',(-3.0567726788274,6.03938716327792,139.346199320266));
#43500=CARTESIAN_POINT('Ctrl Pts',(-3.19903429087571,5.96524077185426,139.353776120456));
#43501=CARTESIAN_POINT('Ctrl Pts',(-3.33828849068273,5.88626528054719,139.361352920646));
#43502=CARTESIAN_POINT('Ctrl Pts',(-3.48945353901703,5.80053476773534,139.369577788324));
#43503=CARTESIAN_POINT('Ctrl Pts',(-3.63752622077289,5.70885705583353,139.377802656001));
#43504=CARTESIAN_POINT('Ctrl Pts',(-3.78200694796311,5.61148041478884,139.386027523679));
#43505=CARTESIAN_POINT('Ctrl Pts',(-3.92632490144238,5.51421347942969,139.394243125123));
#43506=CARTESIAN_POINT('Ctrl Pts',(-4.06705866364899,5.41126059842744,139.402458726566));
#43507=CARTESIAN_POINT('Ctrl Pts',(-4.20373301473877,5.30291596584326,139.41067432801));
#43508=CARTESIAN_POINT('Ctrl Pts',(-4.34028084749351,5.19467162700414,139.418882324338));
#43509=CARTESIAN_POINT('Ctrl Pts',(-4.47277647341769,5.08104569792874,139.427090320666));
#43510=CARTESIAN_POINT('Ctrl Pts',(-4.60077339315962,4.96237576013692,139.435298316994));
#43511=CARTESIAN_POINT('Ctrl Pts',(-4.72867753604107,4.84379183866709,139.443500363865));
#43512=CARTESIAN_POINT('Ctrl Pts',(-4.85208920566462,4.72017143363979,139.451702410737));
#43513=CARTESIAN_POINT('Ctrl Pts',(-4.97059470455424,4.59189256005162,139.459904457608));
#43514=CARTESIAN_POINT('Ctrl Pts',(-5.08903810327832,4.46368090814818,139.46810220638));
#43515=CARTESIAN_POINT('Ctrl Pts',(-5.20258021017523,4.33081591378342,139.476299955151));
#43516=CARTESIAN_POINT('Ctrl Pts',(-5.31084390006278,4.19371268319206,139.484497703923));
#43517=CARTESIAN_POINT('Ctrl Pts',(-5.41908694082581,4.05663560228841,139.492693889139));
#43518=CARTESIAN_POINT('Ctrl Pts',(-5.52205334290557,3.91532217273589,139.500890074354));
#43519=CARTESIAN_POINT('Ctrl Pts',(-5.61940584465528,3.77022107482494,139.50908625957));
#43520=CARTESIAN_POINT('Ctrl Pts',(-5.71675114448669,3.62513071116562,139.51728183845));
#43521=CARTESIAN_POINT('Ctrl Pts',(-5.80848317041546,3.47625353465381,139.525477417331));
#43522=CARTESIAN_POINT('Ctrl Pts',(-5.89430767840892,3.32406768767569,139.533672996211));
#43523=CARTESIAN_POINT('Ctrl Pts',(-5.98014145205202,3.17186541065013,139.541869459889));
#43524=CARTESIAN_POINT('Ctrl Pts',(-6.06006626081168,3.01635406411403,139.550065923568));
#43525=CARTESIAN_POINT('Ctrl Pts',(-6.13383353959432,2.85803693267737,139.558262387246));
#43526=CARTESIAN_POINT('Ctrl Pts',(-6.20762220346182,2.69967390521001,139.566461227074));
#43527=CARTESIAN_POINT('Ctrl Pts',(-6.27524963022061,2.53850379783761,139.574660066902));
#43528=CARTESIAN_POINT('Ctrl Pts',(-6.33651515021793,2.37505047337076,139.58285890673));
#43529=CARTESIAN_POINT('Ctrl Pts',(-6.39784466379375,2.21142641725664,139.591066310479));
#43530=CARTESIAN_POINT('Ctrl Pts',(-6.45279886827092,2.04551471581172,139.599273714228));
#43531=CARTESIAN_POINT('Ctrl Pts',(-6.50122649370331,1.87785597892124,139.607481117978));
#43532=CARTESIAN_POINT('Ctrl Pts',(-6.54968005953462,1.71010743513894,139.615692918047));
#43533=CARTESIAN_POINT('Ctrl Pts',(-6.59159999092413,1.54061033836585,139.623904718116));
#43534=CARTESIAN_POINT('Ctrl Pts',(-6.62688607665502,1.36991602919153,139.632116518185));
#43535=CARTESIAN_POINT('Ctrl Pts',(-6.66222410843459,1.19897043414319,139.640340407171));
#43536=CARTESIAN_POINT('Ctrl Pts',(-6.69090871860183,1.0268244584136,139.648564296157));
#43537=CARTESIAN_POINT('Ctrl Pts',(-6.71289139029902,0.854036405576067,
139.656788185144));
#43538=CARTESIAN_POINT('Ctrl Pts',(-6.73320299891431,0.694383231886422,
139.664386916394));
#43539=CARTESIAN_POINT('Ctrl Pts',(-6.74779342697931,0.534182153838582,
139.671985647644));
#43540=CARTESIAN_POINT('Ctrl Pts',(-6.756663967453,0.373873014434406,139.679584378894));
#43541=CARTESIAN_POINT('Ctrl Pts',(-6.76351075745563,0.250137260535642,
139.685449513866));
#43542=CARTESIAN_POINT('Ctrl Pts',(-6.76695884701256,0.126211727219041,
139.691314648838));
#43543=CARTESIAN_POINT('Ctrl Pts',(-6.76699963384628,0.00222610069067668,
139.69717978381));
#43544=CARTESIAN_POINT('',(-6.76699900574552,0.00191530820773601,139.30282021619));
#43545=CARTESIAN_POINT('Ctrl Pts',(3.09917575053274,6.01559628526631,138.651549674452));
#43546=CARTESIAN_POINT('Ctrl Pts',(2.93643032011442,6.0994411225101,138.660157271204));
#43547=CARTESIAN_POINT('Ctrl Pts',(2.77016378607077,6.17673784217197,138.668764867957));
#43548=CARTESIAN_POINT('Ctrl Pts',(2.60091889377964,6.24720016551256,138.677372464709));
#43549=CARTESIAN_POINT('Ctrl Pts',(2.43188856515335,6.31757315880528,138.685969149005));
#43550=CARTESIAN_POINT('Ctrl Pts',(2.25988769262987,6.38112892639731,138.694565833301));
#43551=CARTESIAN_POINT('Ctrl Pts',(2.08548129553116,6.43762819414027,138.703162517597));
#43552=CARTESIAN_POINT('Ctrl Pts',(1.96437876055543,6.47685957935186,138.709131795548));
#43553=CARTESIAN_POINT('Ctrl Pts',(1.84211691387169,6.51268963392374,138.715101073499));
#43554=CARTESIAN_POINT('Ctrl Pts',(1.71889077907999,6.54505183246044,138.721070351449));
#43555=CARTESIAN_POINT('Ctrl Pts',(1.54144520074409,6.59165338370827,138.729666108997));
#43556=CARTESIAN_POINT('Ctrl Pts',(1.36220751444305,6.63100720467594,138.738261866544));
#43557=CARTESIAN_POINT('Ctrl Pts',(1.18178355520717,6.66300807658537,138.746857624092));
#43558=CARTESIAN_POINT('Ctrl Pts',(1.00119125428201,6.69503880639649,138.755461401773));
#43559=CARTESIAN_POINT('Ctrl Pts',(0.819410771755674,6.71970283992063,138.764065179455));
#43560=CARTESIAN_POINT('Ctrl Pts',(0.637054201472317,6.73694670784818,138.772668957137));
#43561=CARTESIAN_POINT('Ctrl Pts',(0.447530858517566,6.75486827486396,138.781610870805));
#43562=CARTESIAN_POINT('Ctrl Pts',(0.257385606767702,6.76477462134419,138.790552784473));
#43563=CARTESIAN_POINT('Ctrl Pts',(0.0673054826767739,6.76666527707716,
138.799494698141));
#43564=CARTESIAN_POINT('Ctrl Pts',(-0.116084756870127,6.76848939103662,
138.808121900471));
#43565=CARTESIAN_POINT('Ctrl Pts',(-0.299414079998668,6.76285248166214,
138.816749102802));
#43566=CARTESIAN_POINT('Ctrl Pts',(-0.482070316135283,6.74980719800953,
138.825376305133));
#43567=CARTESIAN_POINT('Ctrl Pts',(-0.664900504379287,6.73674949072096,
138.834011723553));
#43568=CARTESIAN_POINT('Ctrl Pts',(-0.847056022907174,6.71626935705887,
138.842647141974));
#43569=CARTESIAN_POINT('Ctrl Pts',(-1.02793231538164,6.6884709878263,138.851282560394));
#43570=CARTESIAN_POINT('Ctrl Pts',(-1.20907582681324,6.66063155046294,138.859930736415));
#43571=CARTESIAN_POINT('Ctrl Pts',(-1.38893603553696,6.62545232648749,138.868578912437));
#43572=CARTESIAN_POINT('Ctrl Pts',(-1.56691955745236,6.58308834062504,138.877227088458));
#43573=CARTESIAN_POINT('Ctrl Pts',(-1.58574953921025,6.57860639155247,138.878142032689));
#43574=CARTESIAN_POINT('Ctrl Pts',(-1.60455853068165,6.57404407022203,138.879056976921));
#43575=CARTESIAN_POINT('Ctrl Pts',(-1.62334584034992,6.56940159242976,138.879971921153));
#43576=CARTESIAN_POINT('Ctrl Pts',(-1.79225697596518,6.5276624499018,138.888197913694));
#43577=CARTESIAN_POINT('Ctrl Pts',(-1.95977899018776,6.47934982852275,138.896423906235));
#43578=CARTESIAN_POINT('Ctrl Pts',(-2.12536348880185,6.42457150637053,138.904649898777));
#43579=CARTESIAN_POINT('Ctrl Pts',(-2.29077439347098,6.36985061220897,138.912867267428));
#43580=CARTESIAN_POINT('Ctrl Pts',(-2.4542514901066,6.30867762728692,138.92108463608));
#43581=CARTESIAN_POINT('Ctrl Pts',(-2.61525783632606,6.24121105632033,138.929302004731));
#43582=CARTESIAN_POINT('Ctrl Pts',(-2.7761276048758,6.173801715564,138.937512402793));
#43583=CARTESIAN_POINT('Ctrl Pts',(-2.93453046863394,6.10010955917699,138.945722800856));
#43584=CARTESIAN_POINT('Ctrl Pts',(-3.0899457952861,6.0203425136942,138.953933198918));
#43585=CARTESIAN_POINT('Ctrl Pts',(-3.24526037616607,5.94062717606265,138.962138274707));
#43586=CARTESIAN_POINT('Ctrl Pts',(-3.39759095994833,5.85484495648378,138.970343350496));
#43587=CARTESIAN_POINT('Ctrl Pts',(-3.54643793101119,5.76325142619035,138.978548426285));
#43588=CARTESIAN_POINT('Ctrl Pts',(-3.69521818334,5.67169895151494,138.986749824254));
#43589=CARTESIAN_POINT('Ctrl Pts',(-3.84051762937841,5.57434054311842,138.994951222223));
#43590=CARTESIAN_POINT('Ctrl Pts',(-3.98186217922372,5.47147718497187,139.003152620193));
#43591=CARTESIAN_POINT('Ctrl Pts',(-4.12319565778759,5.36862188393958,139.011353375761));
#43592=CARTESIAN_POINT('Ctrl Pts',(-4.26057456260895,5.2602626956497,139.019554131328));
#43593=CARTESIAN_POINT('Ctrl Pts',(-4.39355437305861,5.14674353071703,139.027754886896));
#43594=CARTESIAN_POINT('Ctrl Pts',(-4.52653350803412,5.03322494240769,139.035955600808));
#43595=CARTESIAN_POINT('Ctrl Pts',(-4.65511331988828,4.91454666153035,139.044156314719));
#43596=CARTESIAN_POINT('Ctrl Pts',(-4.77888303653782,4.79109235175978,139.052357028631));
#43597=CARTESIAN_POINT('Ctrl Pts',(-4.9026745546507,4.66761629608333,139.060559187061));
#43598=CARTESIAN_POINT('Ctrl Pts',(-5.02165403577198,4.53936278850447,139.068761345491));
#43599=CARTESIAN_POINT('Ctrl Pts',(-5.13544815388113,4.40675178093785,139.07696350392));
#43600=CARTESIAN_POINT('Ctrl Pts',(-5.24928293884472,4.27409338188359,139.085168593573));
#43601=CARTESIAN_POINT('Ctrl Pts',(-5.35792843607556,4.13707465250544,139.093373683226));
#43602=CARTESIAN_POINT('Ctrl Pts',(-5.46105209899662,3.99614801678374,139.101578772879));
#43603=CARTESIAN_POINT('Ctrl Pts',(-5.56429356850904,3.85506038904415,139.109793235877));
#43604=CARTESIAN_POINT('Ctrl Pts',(-5.66200038950564,3.71005622553704,139.118007698875));
#43605=CARTESIAN_POINT('Ctrl Pts',(-5.75388322105544,3.56161717179945,139.126222161872));
#43606=CARTESIAN_POINT('Ctrl Pts',(-5.8458204902793,3.41309017261341,139.13444149168));
#43607=CARTESIAN_POINT('Ctrl Pts',(-5.93192671545112,3.26112453780743,139.142660821487));
#43608=CARTESIAN_POINT('Ctrl Pts',(-6.01195898185081,3.10622571629034,139.150880151295));
#43609=CARTESIAN_POINT('Ctrl Pts',(-6.09211525339475,2.95108688844114,139.159112216456));
#43610=CARTESIAN_POINT('Ctrl Pts',(-6.16617860691969,2.79300611590146,139.167344281616));
#43611=CARTESIAN_POINT('Ctrl Pts',(-6.23395413846561,2.63250922116285,139.175576346777));
#43612=CARTESIAN_POINT('Ctrl Pts',(-6.29487565276906,2.48824308786293,139.182975918038));
#43613=CARTESIAN_POINT('Ctrl Pts',(-6.35071739569539,2.34202521030278,139.190375489299));
#43614=CARTESIAN_POINT('Ctrl Pts',(-6.40137263913761,2.19424641617581,139.19777506056));
#43615=CARTESIAN_POINT('Ctrl Pts',(-6.46711100489098,2.00246495864534,139.207377930647));
#43616=CARTESIAN_POINT('Ctrl Pts',(-6.52428232460604,1.80756608683193,139.216980800734));
#43617=CARTESIAN_POINT('Ctrl Pts',(-6.57262117171399,1.61026082767266,139.22658367082));
#43618=CARTESIAN_POINT('Ctrl Pts',(-6.62073468961635,1.41387529746773,139.236141777591));
#43619=CARTESIAN_POINT('Ctrl Pts',(-6.66009780047818,1.21510584577315,139.245699884361));
#43620=CARTESIAN_POINT('Ctrl Pts',(-6.69049480540422,1.0146764306217,139.255257991132));
#43621=CARTESIAN_POINT('Ctrl Pts',(-6.72062522273823,0.816004820072558,
139.264732271464));
#43622=CARTESIAN_POINT('Ctrl Pts',(-6.74194604189968,0.615702336556618,
139.274206551796));
#43623=CARTESIAN_POINT('Ctrl Pts',(-6.75429365501373,0.414495140914014,
139.283680832128));
#43624=CARTESIAN_POINT('Ctrl Pts',(-6.76260829568126,0.279006158870459,
139.290060626816));
#43625=CARTESIAN_POINT('Ctrl Pts',(-6.76685507026145,0.143107377020171,
139.296440421503));
#43626=CARTESIAN_POINT('Ctrl Pts',(-6.76699635293221,0.00702562468027349,
139.30282021619));
#43627=CARTESIAN_POINT('Ctrl Pts',(-6.767,8.29220280134288E-12,139.30282021619));
#43628=CARTESIAN_POINT('Ctrl Pts',(-6.76700000000023,-0.186007249407506,
139.311569727996));
#43629=CARTESIAN_POINT('Ctrl Pts',(-6.75932637295483,-0.37201435551949,
139.320319239802));
#43630=CARTESIAN_POINT('Ctrl Pts',(-6.74400518266993,-0.557389537147142,
139.329068751608));
#43631=CARTESIAN_POINT('Ctrl Pts',(-6.7286840570973,-0.742763935803766,
139.337818226458));
#43632=CARTESIAN_POINT('Ctrl Pts',(-6.70571545653094,-0.927506129687686,
139.346567701309));
#43633=CARTESIAN_POINT('Ctrl Pts',(-6.67517739415768,-1.1109886392427,139.35531717616));
#43634=CARTESIAN_POINT('Ctrl Pts',(-6.64463945823201,-1.29447038905986,
139.364066614782));
#43635=CARTESIAN_POINT('Ctrl Pts',(-6.60653217027268,-1.47669218227726,
139.372816053404));
#43636=CARTESIAN_POINT('Ctrl Pts',(-6.56098496116829,-1.65703510503657,
139.381565492026));
#43637=CARTESIAN_POINT('Ctrl Pts',(-6.5154379368764,-1.83737729603586,139.390314895146));
#43638=CARTESIAN_POINT('Ctrl Pts',(-6.46245112202766,-2.01584035396648,
139.399064298266));
#43639=CARTESIAN_POINT('Ctrl Pts',(-6.40220448416371,-2.19181813637767,
139.407813701386));
#43640=CARTESIAN_POINT('Ctrl Pts',(-6.34195808575328,-2.36779521935566,
139.416563069732));
#43641=CARTESIAN_POINT('Ctrl Pts',(-6.27445201489388,-2.54128677544449,
139.425312438077));
#43642=CARTESIAN_POINT('Ctrl Pts',(-6.19991555136349,-2.71170355237462,
139.434061806422));
#43643=CARTESIAN_POINT('Ctrl Pts',(-6.12537937789215,-2.88211966612697,
139.442811140719));
#43644=CARTESIAN_POINT('Ctrl Pts',(-6.04381298133804,-3.04946076210075,
139.451560475016));
#43645=CARTESIAN_POINT('Ctrl Pts',(-5.95549339426503,-3.21315848206489,
139.460309809313));
#43646=CARTESIAN_POINT('Ctrl Pts',(-5.86717414355367,-3.37685557859277,
139.469059110289));
#43647=CARTESIAN_POINT('Ctrl Pts',(-5.77210188986454,-3.53690907466958,
139.477808411264));
#43648=CARTESIAN_POINT('Ctrl Pts',(-5.67059953467293,-3.69277536784559,
139.48655771224));
#43649=CARTESIAN_POINT('Ctrl Pts',(-5.56909755762015,-3.84864108035431,
139.495306980621));
#43650=CARTESIAN_POINT('Ctrl Pts',(-5.46116568338345,-4.00031938103902,
139.504056249001));
#43651=CARTESIAN_POINT('Ctrl Pts',(-5.34717048686417,-4.14729511662828,
139.512805517382));
#43652=CARTESIAN_POINT('Ctrl Pts',(-5.23317570555825,-4.29427031687666,
139.521554753895));
#43653=CARTESIAN_POINT('Ctrl Pts',(-5.11311782179116,-4.43654275986771,
139.530303990407));
#43654=CARTESIAN_POINT('Ctrl Pts',(-4.98740459172328,-4.57362924147307,
139.53905322692));
#43655=CARTESIAN_POINT('Ctrl Pts',(-4.8616918091116,-4.71071523514095,139.547802432291));
#43656=CARTESIAN_POINT('Ctrl Pts',(-4.73032391415777,-4.84261509316186,
139.556551637662));
#43657=CARTESIAN_POINT('Ctrl Pts',(-4.59374707237655,-4.96888084331189,
139.565300843033));
#43658=CARTESIAN_POINT('Ctrl Pts',(-4.45717070537763,-5.09514615452409,
139.57405001799));
#43659=CARTESIAN_POINT('Ctrl Pts',(-4.31538563819868,-5.21577720253336,
139.582799192946));
#43660=CARTESIAN_POINT('Ctrl Pts',(-4.16887341291004,-5.33036429028372,
139.591548367902));
#43661=CARTESIAN_POINT('Ctrl Pts',(-4.02236168477714,-5.44495098920899,
139.60029751317));
#43662=CARTESIAN_POINT('Ctrl Pts',(-3.87112305634835,-5.55349359238483,
139.609046658438));
#43663=CARTESIAN_POINT('Ctrl Pts',(-3.71567117317149,-5.655623461022,139.617795803706));
#43664=CARTESIAN_POINT('Ctrl Pts',(-3.56021980457719,-5.75775299158511,
139.626544920012));
#43665=CARTESIAN_POINT('Ctrl Pts',(-3.40055544862808,-5.85346967275109,
139.635294036318));
#43666=CARTESIAN_POINT('Ctrl Pts',(-3.23722036323824,-5.94244842803332,
139.644043152624));
#43667=CARTESIAN_POINT('Ctrl Pts',(-3.07388580496478,-6.03142689616255,
139.652792240695));
#43668=CARTESIAN_POINT('Ctrl Pts',(-2.90688079258149,-6.11366734484612,
139.661541328766));
#43669=CARTESIAN_POINT('Ctrl Pts',(-2.73677251095066,-6.18889046787102,
139.670290416837));
#43670=CARTESIAN_POINT('Ctrl Pts',(-2.56666476417112,-6.26411335438079,
139.679039477399));
#43671=CARTESIAN_POINT('Ctrl Pts',(-2.39345402972576,-6.33231884350108,
139.687788537962));
#43672=CARTESIAN_POINT('Ctrl Pts',(-2.21772856474536,-6.3932752962087,139.696537598524));
#43673=CARTESIAN_POINT('Ctrl Pts',(-2.04200363768781,-6.45423156231919,
139.705286632304));
#43674=CARTESIAN_POINT('Ctrl Pts',(-1.86376426620618,-6.50793874251905,
139.714035666084));
#43675=CARTESIAN_POINT('Ctrl Pts',(-1.68361578195226,-6.55421443795985,
139.722784699864));
#43676=CARTESIAN_POINT('Ctrl Pts',(-1.50346783420434,-6.6004899955855,139.731533707588));
#43677=CARTESIAN_POINT('Ctrl Pts',(-1.32141106257841,-6.63933404145376,
139.740282715312));
#43678=CARTESIAN_POINT('Ctrl Pts',(-1.13806375959667,-6.67061465526924,
139.749031723036));
#43679=CARTESIAN_POINT('Ctrl Pts',(-0.954716987425224,-6.70189517852395,
139.757780705431));
#43680=CARTESIAN_POINT('Ctrl Pts',(-0.770079973815777,-6.72561226535761,
139.766529687826));
#43681=CARTESIAN_POINT('Ctrl Pts',(-0.584779770558182,-6.74168536939732,
139.775278670221));
#43682=CARTESIAN_POINT('Ctrl Pts',(-0.39149064755964,-6.75845143942361,
139.784404850897));
#43683=CARTESIAN_POINT('Ctrl Pts',(-0.19748021311006,-6.7668997592401,139.793531031573));
#43684=CARTESIAN_POINT('Ctrl Pts',(-0.00346532630350954,-6.76699911271707,
139.802657212249));
#43685=CARTESIAN_POINT('Ctrl Pts',(0.184486595290432,-6.76709536139789,
139.811498199779));
#43686=CARTESIAN_POINT('Ctrl Pts',(0.372442378179701,-6.75935659726801,
139.820339187309));
#43687=CARTESIAN_POINT('Ctrl Pts',(0.55975021771666,-6.74380965729062,139.829180174839));
#43688=CARTESIAN_POINT('Ctrl Pts',(0.74512991445234,-6.72842275717313,139.837930153437));
#43689=CARTESIAN_POINT('Ctrl Pts',(0.929874656308788,-6.70538772273548,
139.846680132035));
#43690=CARTESIAN_POINT('Ctrl Pts',(1.1133568828924,-6.67478280180832,139.855430110632));
#43691=CARTESIAN_POINT('Ctrl Pts',(1.29683723118321,-6.64417819418128,139.864179999657));
#43692=CARTESIAN_POINT('Ctrl Pts',(1.47905480729703,-6.60600390230194,139.872929888682));
#43693=CARTESIAN_POINT('Ctrl Pts',(1.65939064804279,-6.56038959797268,139.881679777707));
#43694=CARTESIAN_POINT('Ctrl Pts',(1.83972470263745,-6.51477574543403,139.890429580068));
#43695=CARTESIAN_POINT('Ctrl Pts',(2.01817678125337,-6.4617220982026,139.899179382429));
#43696=CARTESIAN_POINT('Ctrl Pts',(2.19414072347178,-6.40140886724186,139.90792918479));
#43697=CARTESIAN_POINT('Ctrl Pts',(2.37010298131595,-6.34109621361562,139.916678903396));
#43698=CARTESIAN_POINT('Ctrl Pts',(2.54357687926412,-6.27352420826174,139.925428622001));
#43699=CARTESIAN_POINT('Ctrl Pts',(2.71397317789471,-6.19892237325715,139.934178340607));
#43700=CARTESIAN_POINT('Ctrl Pts',(2.884367902067,-6.12432122757199,139.942927978365));
#43701=CARTESIAN_POINT('Ctrl Pts',(3.05168482125755,-6.0426904971767,139.951677616123));
#43702=CARTESIAN_POINT('Ctrl Pts',(3.21535561996888,-5.954307452352,139.960427253881));
#43703=CARTESIAN_POINT('Ctrl Pts',(3.37902496074775,-5.86592519481807,139.9691768137));
#43704=CARTESIAN_POINT('Ctrl Pts',(3.53904799384366,-5.77079087940544,139.977926373519));
#43705=CARTESIAN_POINT('Ctrl Pts',(3.69488118814473,-5.66922763747358,139.986675933338));
#43706=CARTESIAN_POINT('Ctrl Pts',(3.85071304610322,-5.56766526649405,139.995425418126));
#43707=CARTESIAN_POINT('Ctrl Pts',(4.00235489705458,-5.45967423581087,140.004174902913));
#43708=CARTESIAN_POINT('Ctrl Pts',(4.14929168607147,-5.34562133936722,140.012924387701));
#43709=CARTESIAN_POINT('Ctrl Pts',(4.29622726385251,-5.23156938308946,140.021673800364));
#43710=CARTESIAN_POINT('Ctrl Pts',(4.43845763091563,-5.11145583677639,140.030423213027));
#43711=CARTESIAN_POINT('Ctrl Pts',(4.57549970660462,-4.98568866204671,140.03917262569));
#43712=CARTESIAN_POINT('Ctrl Pts',(4.7125406981481,-4.85992248226632,140.047921969137));
#43713=CARTESIAN_POINT('Ctrl Pts',(4.84439326930845,-4.72850295734483,140.056671312583));
#43714=CARTESIAN_POINT('Ctrl Pts',(4.97060959434245,-4.59187644222172,140.06542065603));
#43715=CARTESIAN_POINT('Ctrl Pts',(5.0968249628008,-4.45525096257162,140.074169933166));
#43716=CARTESIAN_POINT('Ctrl Pts',(5.21740397615422,-4.3134187821883,140.082919210302));
#43717=CARTESIAN_POINT('Ctrl Pts',(5.33193710451536,-4.16686161439187,140.091668487438));
#43718=CARTESIAN_POINT('Ctrl Pts',(5.44646940289003,-4.02030550865029,140.100417701171));
#43719=CARTESIAN_POINT('Ctrl Pts',(5.55495572749303,-3.86902470980653,140.109166914904));
#43720=CARTESIAN_POINT('Ctrl Pts',(5.65702762491113,-3.71353301466304,140.117916128637));
#43721=CARTESIAN_POINT('Ctrl Pts',(5.75909881654827,-3.55804239467423,140.126665281873));
#43722=CARTESIAN_POINT('Ctrl Pts',(5.85475551250471,-3.39834117620089,140.13541443511));
#43723=CARTESIAN_POINT('Ctrl Pts',(5.943672837278,-3.23497174692511,140.144163588346));
#43724=CARTESIAN_POINT('Ctrl Pts',(6.0325895767604,-3.071603393015,140.152912683991));
#43725=CARTESIAN_POINT('Ctrl Pts',(6.11476689685035,-2.90456712830031,140.161661779637));
#43726=CARTESIAN_POINT('Ctrl Pts',(6.18992570525032,-2.73443024476422,140.170410875282));
#43727=CARTESIAN_POINT('Ctrl Pts',(6.26508404388486,-2.56429442463547,140.179159916243));
#43728=CARTESIAN_POINT('Ctrl Pts',(6.3332238428312,-2.39105828656509,140.187908957204));
#43729=CARTESIAN_POINT('Ctrl Pts',(6.39411368719854,-2.21531017132597,140.196657998165));
#43730=CARTESIAN_POINT('Ctrl Pts',(6.45500317120724,-2.03956309620039,140.205406987348));
#43731=CARTESIAN_POINT('Ctrl Pts',(6.50864269269921,-1.86130434439165,140.21415597653));
#43732=CARTESIAN_POINT('Ctrl Pts',(6.55485008446195,-1.68113930720483,140.222904965713));
#43733=CARTESIAN_POINT('Ctrl Pts',(6.60199664749285,-1.49731239212364,140.231831779242));
#43734=CARTESIAN_POINT('Ctrl Pts',(6.64140563640806,-1.31150116500181,140.240758592771));
#43735=CARTESIAN_POINT('Ctrl Pts',(6.67293772282089,-1.12436255156154,140.249685406301));
#43736=CARTESIAN_POINT('Ctrl Pts',(6.70384494949803,-0.940932395056238,
140.258435320456));
#43737=CARTESIAN_POINT('Ctrl Pts',(6.72718449348876,-0.756227260511558,
140.267185234612));
#43738=CARTESIAN_POINT('Ctrl Pts',(6.74287707373892,-0.570874564546478,
140.275935148767));
#43739=CARTESIAN_POINT('Ctrl Pts',(6.75856934538643,-0.385525513637225,
140.284684890851));
#43740=CARTESIAN_POINT('Ctrl Pts',(6.76661493004089,-0.199529212422936,
140.293434632935));
#43741=CARTESIAN_POINT('Ctrl Pts',(6.76698649908906,-0.0135174386050861,
140.302184375019));
#43742=CARTESIAN_POINT('Ctrl Pts',(6.76735806132401,0.172490924441198,140.310933956665));
#43743=CARTESIAN_POINT('Ctrl Pts',(6.76005588896313,0.35851447289691,140.319683538311));
#43744=CARTESIAN_POINT('Ctrl Pts',(6.7451047845462,0.543921359657803,140.328433119957));
#43745=CARTESIAN_POINT('Ctrl Pts',(6.73015393440735,0.729325093146103,140.337182552796));
#43746=CARTESIAN_POINT('Ctrl Pts',(6.70755443556955,0.914111900252082,140.345931985635));
#43747=CARTESIAN_POINT('Ctrl Pts',(6.67738304682388,1.09765415591119,140.354681418474));
#43748=CARTESIAN_POINT('Ctrl Pts',(6.6472121311194,1.28119353390863,140.363430714135));
#43749=CARTESIAN_POINT('Ctrl Pts',(6.60946960955583,1.46348811672254,140.372180009797));
#43750=CARTESIAN_POINT('Ctrl Pts',(6.5642836699128,1.64391876347833,140.380929305458));
#43751=CARTESIAN_POINT('Ctrl Pts',(6.51909837867823,1.8243468210934,140.389678475569));
#43752=CARTESIAN_POINT('Ctrl Pts',(6.46646995272034,2.00291071820082,140.39842764568));
#43753=CARTESIAN_POINT('Ctrl Pts',(6.40657713281668,2.17900400212353,140.407176815791));
#43754=CARTESIAN_POINT('Ctrl Pts',(6.34668509279189,2.3550949930931,140.415925871976));
#43755=CARTESIAN_POINT('Ctrl Pts',(6.27952894037665,2.52871516397778,140.424674928162));
#43756=CARTESIAN_POINT('Ctrl Pts',(6.20533675061595,2.69927486771078,140.433423984348));
#43757=CARTESIAN_POINT('Ctrl Pts',(6.12832117908069,2.87632521635599,140.44250598563));
#43758=CARTESIAN_POINT('Ctrl Pts',(6.04372366626235,3.0500772891969,140.451587986912));
#43759=CARTESIAN_POINT('Ctrl Pts',(5.95185378008025,3.21989527477906,140.460669988195));
#43760=CARTESIAN_POINT('Ctrl Pts',(5.86334450817532,3.38350129286473,140.469419768502));
#43761=CARTESIAN_POINT('Ctrl Pts',(5.7680856205742,3.54345567124695,140.478169548809));
#43762=CARTESIAN_POINT('Ctrl Pts',(5.66640068804651,3.69921508465054,140.486919329116));
#43763=CARTESIAN_POINT('Ctrl Pts',(5.56471941108094,3.85496889852037,140.49566879487));
#43764=CARTESIAN_POINT('Ctrl Pts',(5.45661270815287,4.00652780919401,140.504418260623));
#43765=CARTESIAN_POINT('Ctrl Pts',(5.3424477644929,4.15337704569003,140.513167726377));
#43766=CARTESIAN_POINT('Ctrl Pts',(5.22828631819778,4.30022178356027,140.521916924096));
#43767=CARTESIAN_POINT('Ctrl Pts',(5.10806717844259,4.44235690972461,140.530666121816));
#43768=CARTESIAN_POINT('Ctrl Pts',(4.98219864544916,4.57929969070431,140.539415319535));
#43769=CARTESIAN_POINT('Ctrl Pts',(4.85633329944237,4.71623900429782,140.548164295726));
#43770=CARTESIAN_POINT('Ctrl Pts',(4.72481904033877,4.84798602483394,140.556913271916));
#43771=CARTESIAN_POINT('Ctrl Pts',(4.58810250737444,4.97409332258899,140.565662248106));
#43772=CARTESIAN_POINT('Ctrl Pts',(4.45137708685898,5.10020881821912,140.574411793042));
#43773=CARTESIAN_POINT('Ctrl Pts',(4.30944892636317,5.22068366307714,140.583161337978));
#43774=CARTESIAN_POINT('Ctrl Pts',(4.16280009466937,5.33510865604635,140.591910882915));
#43775=CARTESIAN_POINT('Ctrl Pts',(4.01615988349057,5.44952692272694,140.600659913523));
#43776=CARTESIAN_POINT('Ctrl Pts',(3.8647997823249,5.55789587288446,140.609408944131));
#43777=CARTESIAN_POINT('Ctrl Pts',(3.70923383581317,5.65984746713714,140.618157974739));
#43778=CARTESIAN_POINT('Ctrl Pts',(3.55366577799787,5.76180044505231,140.626907124087));
#43779=CARTESIAN_POINT('Ctrl Pts',(3.39389200027082,5.85733573570919,140.635656273435));
#43780=CARTESIAN_POINT('Ctrl Pts',(3.23045513626279,5.94612887621799,140.644405422784));
#43781=CARTESIAN_POINT('Ctrl Pts',(3.18695122151738,5.96976399206604,140.646734286897));
#43782=CARTESIAN_POINT('Ctrl Pts',(3.14318791262744,5.99292165435291,140.64906315101));
#43783=CARTESIAN_POINT('Ctrl Pts',(3.09917575053259,6.01559628526639,140.651392015123));
#43784=CARTESIAN_POINT('Origin',(0.,0.,-3.69717978381041));
#43785=CARTESIAN_POINT('',(3.09917575053276,6.0155962852663,143.045751582742));
#43786=CARTESIAN_POINT('',(3.09917575053256,6.0155962852664,142.651137628792));
#43787=CARTESIAN_POINT('',(3.09917575053259,6.01559628526639,-3.69717978381041));
#43788=CARTESIAN_POINT('',(-6.767,8.61074883271029E-12,141.69717978381));
#43789=CARTESIAN_POINT('Ctrl Pts',(-6.767,8.61074887974675E-12,141.69717978381));
#43790=CARTESIAN_POINT('Ctrl Pts',(-6.76700000000024,-0.186007249407185,
141.705929295616));
#43791=CARTESIAN_POINT('Ctrl Pts',(-6.75932637295485,-0.372014355519164,
141.714678807422));
#43792=CARTESIAN_POINT('Ctrl Pts',(-6.74400518266996,-0.557389537146815,
141.723428319228));
#43793=CARTESIAN_POINT('Ctrl Pts',(-6.72868405709736,-0.742763935803183,
141.732177794078));
#43794=CARTESIAN_POINT('Ctrl Pts',(-6.70571545653104,-0.927506129686851,
141.740927268929));
#43795=CARTESIAN_POINT('Ctrl Pts',(-6.67517739415786,-1.11098863924161,
141.74967674378));
#43796=CARTESIAN_POINT('Ctrl Pts',(-6.64463945823222,-1.29447038905877,
141.758426182402));
#43797=CARTESIAN_POINT('Ctrl Pts',(-6.60653217027292,-1.47669218227619,
141.767175621023));
#43798=CARTESIAN_POINT('Ctrl Pts',(-6.56098496116856,-1.6570351050355,141.775925059645));
#43799=CARTESIAN_POINT('Ctrl Pts',(-6.5154379368767,-1.8373772960348,141.784674462766));
#43800=CARTESIAN_POINT('Ctrl Pts',(-6.46245112202799,-2.01584035396542,
141.793423865886));
#43801=CARTESIAN_POINT('Ctrl Pts',(-6.40220448416407,-2.19181813637662,
141.802173269006));
#43802=CARTESIAN_POINT('Ctrl Pts',(-6.34195808575363,-2.36779521935474,
141.810922637351));
#43803=CARTESIAN_POINT('Ctrl Pts',(-6.2744520148942,-2.54128677544369,141.819672005697));
#43804=CARTESIAN_POINT('Ctrl Pts',(-6.19991555136379,-2.71170355237395,
141.828421374042));
#43805=CARTESIAN_POINT('Ctrl Pts',(-6.12537937789256,-2.88211966612607,
141.837170708339));
#43806=CARTESIAN_POINT('Ctrl Pts',(-6.04381298133859,-3.04946076209963,
141.845920042636));
#43807=CARTESIAN_POINT('Ctrl Pts',(-5.95549339426575,-3.21315848206357,
141.854669376933));
#43808=CARTESIAN_POINT('Ctrl Pts',(-5.86717414355442,-3.37685557859146,
141.863418677909));
#43809=CARTESIAN_POINT('Ctrl Pts',(-5.77210188986533,-3.5369090746683,141.872167978884));
#43810=CARTESIAN_POINT('Ctrl Pts',(-5.67059953467376,-3.69277536784433,
141.88091727986));
#43811=CARTESIAN_POINT('Ctrl Pts',(-5.5690975576208,-3.84864108035339,141.889666548241));
#43812=CARTESIAN_POINT('Ctrl Pts',(-5.4611656833839,-4.00031938103843,141.898415816621));
#43813=CARTESIAN_POINT('Ctrl Pts',(-5.34717048686439,-4.147295116628,141.907165085002));
#43814=CARTESIAN_POINT('Ctrl Pts',(-5.23317570555848,-4.29427031687638,
141.915914321515));
#43815=CARTESIAN_POINT('Ctrl Pts',(-5.1131178217914,-4.43654275986744,141.924663558027));
#43816=CARTESIAN_POINT('Ctrl Pts',(-4.98740459172353,-4.57362924147281,
141.93341279454));
#43817=CARTESIAN_POINT('Ctrl Pts',(-4.86169180911176,-4.71071523514079,
141.942161999911));
#43818=CARTESIAN_POINT('Ctrl Pts',(-4.73032391415785,-4.84261509316178,
141.950911205282));
#43819=CARTESIAN_POINT('Ctrl Pts',(-4.59374707237654,-4.9688808433119,141.959660410653));
#43820=CARTESIAN_POINT('Ctrl Pts',(-4.45717070537781,-5.09514615452392,
141.96840958561));
#43821=CARTESIAN_POINT('Ctrl Pts',(-4.31538563819906,-5.21577720253303,
141.977158760566));
#43822=CARTESIAN_POINT('Ctrl Pts',(-4.16887341291064,-5.33036429028325,
141.985907935522));
#43823=CARTESIAN_POINT('Ctrl Pts',(-4.02236168477765,-5.44495098920861,
141.99465708079));
#43824=CARTESIAN_POINT('Ctrl Pts',(-3.87112305634876,-5.55349359238454,
142.003406226058));
#43825=CARTESIAN_POINT('Ctrl Pts',(-3.7156711731718,-5.65562346102179,142.012155371326));
#43826=CARTESIAN_POINT('Ctrl Pts',(-3.56021980457752,-5.7577529915849,142.020904487632));
#43827=CARTESIAN_POINT('Ctrl Pts',(-3.40055544862841,-5.8534696727509,142.029653603938));
#43828=CARTESIAN_POINT('Ctrl Pts',(-3.23722036323858,-5.94244842803314,
142.038402720244));
#43829=CARTESIAN_POINT('Ctrl Pts',(-3.07388580496535,-6.03142689616225,
142.047151808315));
#43830=CARTESIAN_POINT('Ctrl Pts',(-2.9068807925823,-6.11366734484573,142.055900896386));
#43831=CARTESIAN_POINT('Ctrl Pts',(-2.73677251095172,-6.18889046787056,
142.064649984457));
#43832=CARTESIAN_POINT('Ctrl Pts',(-2.56666476417208,-6.2641133543804,142.073399045019));
#43833=CARTESIAN_POINT('Ctrl Pts',(-2.39345402972661,-6.33231884350076,
142.082148105582));
#43834=CARTESIAN_POINT('Ctrl Pts',(-2.2177285647461,-6.39327529620845,142.090897166144));
#43835=CARTESIAN_POINT('Ctrl Pts',(-2.04200363768844,-6.454231562319,142.099646199924));
#43836=CARTESIAN_POINT('Ctrl Pts',(-1.86376426620669,-6.50793874251891,
142.108395233704));
#43837=CARTESIAN_POINT('Ctrl Pts',(-1.68361578195264,-6.55421443795975,
142.117144267484));
#43838=CARTESIAN_POINT('Ctrl Pts',(-1.50346783420461,-6.60048999558544,
142.125893275208));
#43839=CARTESIAN_POINT('Ctrl Pts',(-1.32141106257856,-6.63933404145374,
142.134642282932));
#43840=CARTESIAN_POINT('Ctrl Pts',(-1.13806375959669,-6.67061465526923,
142.143391290656));
#43841=CARTESIAN_POINT('Ctrl Pts',(-0.954716987425243,-6.70189517852394,
142.152140273051));
#43842=CARTESIAN_POINT('Ctrl Pts',(-0.770079973815802,-6.7256122653576,
142.160889255446));
#43843=CARTESIAN_POINT('Ctrl Pts',(-0.584779770558209,-6.74168536939732,
142.169638237841));
#43844=CARTESIAN_POINT('Ctrl Pts',(-0.391490647559668,-6.75845143942361,
142.178764418517));
#43845=CARTESIAN_POINT('Ctrl Pts',(-0.197480213110089,-6.7668997592401,
142.187890599193));
#43846=CARTESIAN_POINT('Ctrl Pts',(-0.0034653263035411,-6.76699911271707,
142.197016779869));
#43847=CARTESIAN_POINT('Ctrl Pts',(0.184486595290399,-6.76709536139789,
142.205857767399));
#43848=CARTESIAN_POINT('Ctrl Pts',(0.372442378179669,-6.75935659726801,
142.214698754929));
#43849=CARTESIAN_POINT('Ctrl Pts',(0.559750217716626,-6.74380965729062,
142.223539742459));
#43850=CARTESIAN_POINT('Ctrl Pts',(0.745129914452304,-6.72842275717314,
142.232289721057));
#43851=CARTESIAN_POINT('Ctrl Pts',(0.929874656308751,-6.70538772273548,
142.241039699655));
#43852=CARTESIAN_POINT('Ctrl Pts',(1.11335688289236,-6.67478280180833,142.249789678252));
#43853=CARTESIAN_POINT('Ctrl Pts',(1.29683723118317,-6.64417819418129,142.258539567277));
#43854=CARTESIAN_POINT('Ctrl Pts',(1.47905480729698,-6.60600390230195,142.267289456302));
#43855=CARTESIAN_POINT('Ctrl Pts',(1.65939064804274,-6.56038959797269,142.276039345327));
#43856=CARTESIAN_POINT('Ctrl Pts',(1.83972470263728,-6.51477574543408,142.284789147688));
#43857=CARTESIAN_POINT('Ctrl Pts',(2.01817678125308,-6.46172209820268,142.293538950049));
#43858=CARTESIAN_POINT('Ctrl Pts',(2.19414072347137,-6.401408867242,142.30228875241));
#43859=CARTESIAN_POINT('Ctrl Pts',(2.37010298131555,-6.34109621361577,142.311038471016));
#43860=CARTESIAN_POINT('Ctrl Pts',(2.54357687926371,-6.2735242082619,142.319788189621));
#43861=CARTESIAN_POINT('Ctrl Pts',(2.71397317789431,-6.19892237325733,142.328537908227));
#43862=CARTESIAN_POINT('Ctrl Pts',(2.8843679020666,-6.12432122757218,142.337287545985));
#43863=CARTESIAN_POINT('Ctrl Pts',(3.05168482125716,-6.0426904971769,142.346037183743));
#43864=CARTESIAN_POINT('Ctrl Pts',(3.21535561996849,-5.95430745235221,142.354786821501));
#43865=CARTESIAN_POINT('Ctrl Pts',(3.37902496074748,-5.86592519481823,142.36353638132));
#43866=CARTESIAN_POINT('Ctrl Pts',(3.5390479938435,-5.77079087940554,142.372285941139));
#43867=CARTESIAN_POINT('Ctrl Pts',(3.69488118814467,-5.66922763747361,142.381035500958));
#43868=CARTESIAN_POINT('Ctrl Pts',(3.85071304610327,-5.56766526649402,142.389784985746));
#43869=CARTESIAN_POINT('Ctrl Pts',(4.00235489705474,-5.45967423581076,142.398534470533));
#43870=CARTESIAN_POINT('Ctrl Pts',(4.14929168607172,-5.34562133936703,142.407283955321));
#43871=CARTESIAN_POINT('Ctrl Pts',(4.29622726385275,-5.23156938308926,142.416033367984));
#43872=CARTESIAN_POINT('Ctrl Pts',(4.43845763091587,-5.11145583677619,142.424782780647));
#43873=CARTESIAN_POINT('Ctrl Pts',(4.57549970660485,-4.9856886620465,142.433532193311));
#43874=CARTESIAN_POINT('Ctrl Pts',(4.71254069814832,-4.8599224822661,142.442281536757));
#43875=CARTESIAN_POINT('Ctrl Pts',(4.84439326930866,-4.72850295734461,142.451030880203));
#43876=CARTESIAN_POINT('Ctrl Pts',(4.97060959434265,-4.5918764422215,142.45978022365));
#43877=CARTESIAN_POINT('Ctrl Pts',(5.096824962801,-4.45525096257139,142.468529500786));
#43878=CARTESIAN_POINT('Ctrl Pts',(5.21740397615442,-4.31341878218807,142.477278777922));
#43879=CARTESIAN_POINT('Ctrl Pts',(5.33193710451554,-4.16686161439163,142.486028055058));
#43880=CARTESIAN_POINT('Ctrl Pts',(5.44646940289021,-4.02030550865005,142.494777268791));
#43881=CARTESIAN_POINT('Ctrl Pts',(5.5549557274932,-3.86902470980628,142.503526482524));
#43882=CARTESIAN_POINT('Ctrl Pts',(5.65702762491129,-3.7135330146628,142.512275696257));
#43883=CARTESIAN_POINT('Ctrl Pts',(5.75909881654849,-3.55804239467387,142.521024849493));
#43884=CARTESIAN_POINT('Ctrl Pts',(5.85475551250499,-3.39834117620041,142.52977400273));
#43885=CARTESIAN_POINT('Ctrl Pts',(5.94367283727832,-3.23497174692451,142.538523155966));
#43886=CARTESIAN_POINT('Ctrl Pts',(6.0325895767607,-3.07160339301441,142.547272251611));
#43887=CARTESIAN_POINT('Ctrl Pts',(6.11476689685063,-2.9045671282997,142.556021347257));
#43888=CARTESIAN_POINT('Ctrl Pts',(6.18992570525059,-2.73443024476361,142.564770442902));
#43889=CARTESIAN_POINT('Ctrl Pts',(6.26508404388511,-2.56429442463485,142.573519483863));
#43890=CARTESIAN_POINT('Ctrl Pts',(6.33322384283144,-2.39105828656447,142.582268524824));
#43891=CARTESIAN_POINT('Ctrl Pts',(6.39411368719876,-2.21531017132534,142.591017565785));
#43892=CARTESIAN_POINT('Ctrl Pts',(6.45500317120744,-2.03956309619975,142.599766554968));
#43893=CARTESIAN_POINT('Ctrl Pts',(6.50864269269939,-1.86130434439101,142.60851554415));
#43894=CARTESIAN_POINT('Ctrl Pts',(6.55485008446212,-1.68113930720419,142.617264533333));
#43895=CARTESIAN_POINT('Ctrl Pts',(6.60199664749297,-1.49731239212313,142.626191346862));
#43896=CARTESIAN_POINT('Ctrl Pts',(6.64140563640814,-1.31150116500142,142.635118160391));
#43897=CARTESIAN_POINT('Ctrl Pts',(6.67293772282093,-1.12436255156127,142.644044973921));
#43898=CARTESIAN_POINT('Ctrl Pts',(6.70384494949804,-0.9409323950561,142.652794888076));
#43899=CARTESIAN_POINT('Ctrl Pts',(6.72718449348876,-0.75622726051155,142.661544802232));
#43900=CARTESIAN_POINT('Ctrl Pts',(6.74287707373891,-0.5708745645466,142.670294716387));
#43901=CARTESIAN_POINT('Ctrl Pts',(6.75856934538643,-0.385525513637349,
142.679044458471));
#43902=CARTESIAN_POINT('Ctrl Pts',(6.76661493004089,-0.199529212423061,
142.687794200555));
#43903=CARTESIAN_POINT('Ctrl Pts',(6.76698649908906,-0.0135174386052131,
142.696543942639));
#43904=CARTESIAN_POINT('Ctrl Pts',(6.76735806132401,0.172490924441069,142.705293524285));
#43905=CARTESIAN_POINT('Ctrl Pts',(6.76005588896314,0.358514472896781,142.714043105931));
#43906=CARTESIAN_POINT('Ctrl Pts',(6.74510478454621,0.543921359657673,142.722792687577));
#43907=CARTESIAN_POINT('Ctrl Pts',(6.73015393440736,0.729325093145971,142.731542120416));
#43908=CARTESIAN_POINT('Ctrl Pts',(6.70755443556957,0.914111900251948,142.740291553255));
#43909=CARTESIAN_POINT('Ctrl Pts',(6.6773830468239,1.09765415591105,142.749040986094));
#43910=CARTESIAN_POINT('Ctrl Pts',(6.64721213111942,1.2811935339085,142.757790281755));
#43911=CARTESIAN_POINT('Ctrl Pts',(6.60946960955586,1.4634881167224,142.766539577417));
#43912=CARTESIAN_POINT('Ctrl Pts',(6.56428366991284,1.64391876347819,142.775288873078));
#43913=CARTESIAN_POINT('Ctrl Pts',(6.5190983786783,1.82434682109313,142.784038043189));
#43914=CARTESIAN_POINT('Ctrl Pts',(6.46646995272046,2.00291071820043,142.7927872133));
#43915=CARTESIAN_POINT('Ctrl Pts',(6.40657713281685,2.17900400212303,142.801536383411));
#43916=CARTESIAN_POINT('Ctrl Pts',(6.34668509279207,2.3550949930926,142.810285439596));
#43917=CARTESIAN_POINT('Ctrl Pts',(6.27952894037685,2.52871516397728,142.819034495782));
#43918=CARTESIAN_POINT('Ctrl Pts',(6.20533675061617,2.69927486771029,142.827783551968));
#43919=CARTESIAN_POINT('Ctrl Pts',(6.12832117908092,2.8763252163555,142.83686555325));
#43920=CARTESIAN_POINT('Ctrl Pts',(6.04372366626259,3.05007728919642,142.845947554532));
#43921=CARTESIAN_POINT('Ctrl Pts',(5.9518537800805,3.21989527477858,142.855029555815));
#43922=CARTESIAN_POINT('Ctrl Pts',(5.86334450817565,3.38350129286415,142.863779336122));
#43923=CARTESIAN_POINT('Ctrl Pts',(5.76808562057461,3.54345567124627,142.872529116429));
#43924=CARTESIAN_POINT('Ctrl Pts',(5.66640068804702,3.69921508464976,142.881278896736));
#43925=CARTESIAN_POINT('Ctrl Pts',(5.56471941108154,3.8549688985195,142.89002836249));
#43926=CARTESIAN_POINT('Ctrl Pts',(5.45661270815357,4.00652780919305,142.898777828243));
#43927=CARTESIAN_POINT('Ctrl Pts',(5.34244776449371,4.15337704568899,142.907527293997));
#43928=CARTESIAN_POINT('Ctrl Pts',(5.22828631819854,4.30022178355935,142.916276491716));
#43929=CARTESIAN_POINT('Ctrl Pts',(5.10806717844329,4.4423569097238,142.925025689436));
#43930=CARTESIAN_POINT('Ctrl Pts',(4.98219864544979,4.57929969070362,142.933774887155));
#43931=CARTESIAN_POINT('Ctrl Pts',(4.85633329944285,4.71623900429733,142.942523863346));
#43932=CARTESIAN_POINT('Ctrl Pts',(4.72481904033908,4.84798602483364,142.951272839536));
#43933=CARTESIAN_POINT('Ctrl Pts',(4.58810250737457,4.97409332258887,142.960021815726));
#43934=CARTESIAN_POINT('Ctrl Pts',(4.45137708685902,5.10020881821909,142.968771360662));
#43935=CARTESIAN_POINT('Ctrl Pts',(4.30944892636311,5.22068366307719,142.977520905598));
#43936=CARTESIAN_POINT('Ctrl Pts',(4.16280009466921,5.33510865604648,142.986270450535));
#43937=CARTESIAN_POINT('Ctrl Pts',(4.01615988349061,5.4495269227269,142.995019481143));
#43938=CARTESIAN_POINT('Ctrl Pts',(3.86479978232516,5.55789587288428,143.003768511751));
#43939=CARTESIAN_POINT('Ctrl Pts',(3.70923383581365,5.65984746713683,143.012517542359));
#43940=CARTESIAN_POINT('Ctrl Pts',(3.55366577799846,5.76180044505194,143.021266691707));
#43941=CARTESIAN_POINT('Ctrl Pts',(3.39389200027154,5.85733573570877,143.030015841055));
#43942=CARTESIAN_POINT('Ctrl Pts',(3.23045513626363,5.94612887621753,143.038764990403));
#43943=CARTESIAN_POINT('Ctrl Pts',(3.186951221518,5.96976399206571,143.041093854516));
#43944=CARTESIAN_POINT('Ctrl Pts',(3.14318791262784,5.99292165435271,143.04342271863));
#43945=CARTESIAN_POINT('Ctrl Pts',(3.09917575053276,6.0155962852663,143.045751582743));
#43946=CARTESIAN_POINT('Ctrl Pts',(3.09917575053271,6.01559628526633,141.045900408649));
#43947=CARTESIAN_POINT('Ctrl Pts',(2.94392531879992,6.09557977326476,141.054101057528));
#43948=CARTESIAN_POINT('Ctrl Pts',(2.78549957819497,6.16958901908825,141.062301706407));
#43949=CARTESIAN_POINT('Ctrl Pts',(2.62440023039033,6.23737223762757,141.070502355286));
#43950=CARTESIAN_POINT('Ctrl Pts',(2.46049844904947,6.30633459169672,141.078845660071));
#43951=CARTESIAN_POINT('Ctrl Pts',(2.29382951096609,6.36885211567673,141.087188964856));
#43952=CARTESIAN_POINT('Ctrl Pts',(2.12494493933669,6.42470995491527,141.095532269641));
#43953=CARTESIAN_POINT('Ctrl Pts',(1.958977437471,6.47960298598729,141.103731464151));
#43954=CARTESIAN_POINT('Ctrl Pts',(1.79087057807845,6.5280644314441,141.111930658661));
#43955=CARTESIAN_POINT('Ctrl Pts',(1.62116474209249,6.5699401731672,141.120129853171));
#43956=CARTESIAN_POINT('Ctrl Pts',(1.45143515441507,6.61182177573587,141.128330195223));
#43957=CARTESIAN_POINT('Ctrl Pts',(1.28010649233721,6.6471157521242,141.136530537276));
#43958=CARTESIAN_POINT('Ctrl Pts',(1.10773096853083,6.67571877039153,141.144730879329));
#43959=CARTESIAN_POINT('Ctrl Pts',(0.935300048529582,6.70433098078973,141.152933856719));
#43960=CARTESIAN_POINT('Ctrl Pts',(0.761821950131028,6.72624789093049,141.16113683411));
#43961=CARTESIAN_POINT('Ctrl Pts',(0.587855728529647,6.74141785104846,141.1693398115));
#43962=CARTESIAN_POINT('Ctrl Pts',(0.408647442634721,6.75704492235468,141.177789966386));
#43963=CARTESIAN_POINT('Ctrl Pts',(0.228921566005123,6.765512031444,141.186240121272));
#43964=CARTESIAN_POINT('Ctrl Pts',(0.0492902242368824,6.76682048482112,
141.194690276157));
#43965=CARTESIAN_POINT('Ctrl Pts',(-0.125385348580903,6.76809283986175,
141.202907303489));
#43966=CARTESIAN_POINT('Ctrl Pts',(-0.299971179635794,6.76259637893075,
141.211124330822));
#43967=CARTESIAN_POINT('Ctrl Pts',(-0.473909036402681,6.75038511680748,
141.219341358154));
#43968=CARTESIAN_POINT('Ctrl Pts',(-0.655249151676379,6.73765418104553,
141.227908076816));
#43969=CARTESIAN_POINT('Ctrl Pts',(-0.835884485223362,6.71762445440569,
141.236474795479));
#43970=CARTESIAN_POINT('Ctrl Pts',(-1.01519399128521,6.69041629198501,141.245041514141));
#43971=CARTESIAN_POINT('Ctrl Pts',(-1.19450349734705,6.66320812956433,141.253608232803));
#43972=CARTESIAN_POINT('Ctrl Pts',(-1.37248676300084,6.62882168162202,141.262174951465));
#43973=CARTESIAN_POINT('Ctrl Pts',(-1.54854076241575,6.58743580668054,141.270741670128));
#43974=CARTESIAN_POINT('Ctrl Pts',(-1.71611079516019,6.54804429928992,141.278895562294));
#43975=CARTESIAN_POINT('Ctrl Pts',(-1.8824512869401,6.50219016550125,141.287049454461));
#43976=CARTESIAN_POINT('Ctrl Pts',(-2.04702016246669,6.44996104286335,141.295203346628));
#43977=CARTESIAN_POINT('Ctrl Pts',(-2.21138821798702,6.39779565434711,141.303347288768));
#43978=CARTESIAN_POINT('Ctrl Pts',(-2.37398861583787,6.339270871206,141.311491230908));
#43979=CARTESIAN_POINT('Ctrl Pts',(-2.53428881202539,6.2745254176904,141.319635173048));
#43980=CARTESIAN_POINT('Ctrl Pts',(-2.69442713718199,6.20984534409047,141.327770891441));
#43981=CARTESIAN_POINT('Ctrl Pts',(-2.85226954830692,6.13895724151273,141.335906609834));
#43982=CARTESIAN_POINT('Ctrl Pts',(-3.0072980347807,6.06204977957161,141.344042328227));
#43983=CARTESIAN_POINT('Ctrl Pts',(-3.16220258387119,5.98520380123137,141.352171542527));
#43984=CARTESIAN_POINT('Ctrl Pts',(-3.31429736145067,5.90234820680222,141.360300756827));
#43985=CARTESIAN_POINT('Ctrl Pts',(-3.46308375362178,5.81371997222096,141.368429971127));
#43986=CARTESIAN_POINT('Ctrl Pts',(-3.61178248283268,5.72514395621485,141.376554395803));
#43987=CARTESIAN_POINT('Ctrl Pts',(-3.75717639514937,5.63080225999025,141.384678820478));
#43988=CARTESIAN_POINT('Ctrl Pts',(-3.89879094817286,5.53097804573887,141.392803245154));
#43989=CARTESIAN_POINT('Ctrl Pts',(-4.04126519219066,5.43054783460247,141.400976990288));
#43990=CARTESIAN_POINT('Ctrl Pts',(-4.17991370426195,5.32456848964003,141.409150735422));
#43991=CARTESIAN_POINT('Ctrl Pts',(-4.3142818636197,5.21337328427978,141.417324480556));
#43992=CARTESIAN_POINT('Ctrl Pts',(-4.44778956860342,5.10289014047698,141.425445883418));
#43993=CARTESIAN_POINT('Ctrl Pts',(-4.57707131033809,4.98725799648973,141.43356728628));
#43994=CARTESIAN_POINT('Ctrl Pts',(-4.70171373100924,4.86684466483565,141.441688689142));
#43995=CARTESIAN_POINT('Ctrl Pts',(-4.82636578837591,4.74642202345693,141.449810719909));
#43996=CARTESIAN_POINT('Ctrl Pts',(-4.94637754695109,4.62121771234742,141.457932750675));
#43997=CARTESIAN_POINT('Ctrl Pts',(-5.06137215960588,4.4916367687032,141.466054781441));
#43998=CARTESIAN_POINT('Ctrl Pts',(-5.17639756066847,4.36202113133861,141.474178986782));
#43999=CARTESIAN_POINT('Ctrl Pts',(-5.28640289827642,4.22802680182094,141.482303192123));
#44000=CARTESIAN_POINT('Ctrl Pts',(-5.39105133537233,4.09009223604801,141.490427397464));
#44001=CARTESIAN_POINT('Ctrl Pts',(-5.49683251938946,3.9506646240429,141.498639541707));
#44002=CARTESIAN_POINT('Ctrl Pts',(-5.59713992333364,3.80721128192054,141.506851685949));
#44003=CARTESIAN_POINT('Ctrl Pts',(-5.69167082960152,3.66021477067442,141.515063830192));
#44004=CARTESIAN_POINT('Ctrl Pts',(-5.78533877288137,3.51456017556538,141.523201006608));
#44005=CARTESIAN_POINT('Ctrl Pts',(-5.87333511422548,3.36542717952042,141.531338183025));
#44006=CARTESIAN_POINT('Ctrl Pts',(-5.9554120167134,3.21330930835885,141.539475359441));
#44007=CARTESIAN_POINT('Ctrl Pts',(-6.03862318125308,3.05908924372479,141.547724987596));
#44008=CARTESIAN_POINT('Ctrl Pts',(-6.11574992864197,2.90180155320928,141.555974615752));
#44009=CARTESIAN_POINT('Ctrl Pts',(-6.18658494147511,2.74198026285994,141.564224243907));
#44010=CARTESIAN_POINT('Ctrl Pts',(-6.2574199543082,2.58215897251071,141.572473872063));
#44011=CARTESIAN_POINT('Ctrl Pts',(-6.32196314922586,2.41980446325587,141.580723500218));
#44012=CARTESIAN_POINT('Ctrl Pts',(-6.38006006919299,2.25546503264607,141.588973128374));
#44013=CARTESIAN_POINT('Ctrl Pts',(-6.44833391140206,2.06233802418279,141.59866785593));
#44014=CARTESIAN_POINT('Ctrl Pts',(-6.50787396952278,1.86599841217219,141.608362583487));
#44015=CARTESIAN_POINT('Ctrl Pts',(-6.55841537856759,1.66717627207447,141.618057311044));
#44016=CARTESIAN_POINT('Ctrl Pts',(-6.60874513278828,1.46918674954501,141.627711439498));
#44017=CARTESIAN_POINT('Ctrl Pts',(-6.65015138029429,1.26873551353126,141.637365567952));
#44018=CARTESIAN_POINT('Ctrl Pts',(-6.68241934800761,1.06656488662131,141.647019696406));
#44019=CARTESIAN_POINT('Ctrl Pts',(-6.71440970154839,0.866133614101466,
141.65659076655));
#44020=CARTESIAN_POINT('Ctrl Pts',(-6.73741828367758,0.664012490796059,
141.666161836694));
#44021=CARTESIAN_POINT('Ctrl Pts',(-6.7512827600329,0.46094478420152,141.675732906837));
#44022=CARTESIAN_POINT('Ctrl Pts',(-6.76163861067503,0.309266582599061,
141.682881865828));
#44023=CARTESIAN_POINT('Ctrl Pts',(-6.76689381230157,0.15706068684614,141.690030824819));
#44024=CARTESIAN_POINT('Ctrl Pts',(-6.76699840663235,0.00464377381538438,
141.69717978381));
#44025=CARTESIAN_POINT('',(-6.76796187734296,-0.00130286369752294,141.304484749508));
#44026=CARTESIAN_POINT('Ctrl Pts',(3.09917575053259,6.01559628526639,140.651392015123));
#44027=CARTESIAN_POINT('Ctrl Pts',(2.9338238445927,6.10078395293757,140.660141463035));
#44028=CARTESIAN_POINT('Ctrl Pts',(2.76495772122994,6.17915010267044,140.668890910947));
#44029=CARTESIAN_POINT('Ctrl Pts',(2.59315093316727,6.25042856433171,140.67764035886));
#44030=CARTESIAN_POINT('Ctrl Pts',(2.42134553245637,6.32170645041443,140.68638973612));
#44031=CARTESIAN_POINT('Ctrl Pts',(2.24659977927615,6.38589665313448,140.69513911338));
#44032=CARTESIAN_POINT('Ctrl Pts',(2.06950718689948,6.44278115439066,140.70388849064));
#44033=CARTESIAN_POINT('Ctrl Pts',(1.89241596572883,6.49966521519718,140.712637800154));
#44034=CARTESIAN_POINT('Ctrl Pts',(1.71297821457211,6.54924360009543,140.721387109669));
#44035=CARTESIAN_POINT('Ctrl Pts',(1.5318033733585,6.59134792173555,140.730136419184));
#44036=CARTESIAN_POINT('Ctrl Pts',(1.35062987477787,6.63345193135304,140.73888566386));
#44037=CARTESIAN_POINT('Ctrl Pts',(1.16771959102955,6.66808192368237,140.747634908536));
#44038=CARTESIAN_POINT('Ctrl Pts',(0.983693746906859,6.69512028363168,140.756384153212));
#44039=CARTESIAN_POINT('Ctrl Pts',(0.799669205419866,6.72215845218867,140.765133335956));
#44040=CARTESIAN_POINT('Ctrl Pts',(0.614529402873451,6.74160505424579,140.7738825187));
#44041=CARTESIAN_POINT('Ctrl Pts',(0.428903127363203,6.75339404354122,140.782631701445));
#44042=CARTESIAN_POINT('Ctrl Pts',(0.243278104163965,6.7651829533033,140.791380825163));
#44043=CARTESIAN_POINT('Ctrl Pts',(0.0571669005393323,6.76931433552275,
140.800129948882));
#44044=CARTESIAN_POINT('Ctrl Pts',(-0.128798404777167,6.76577415902474,
140.8088790726));
#44045=CARTESIAN_POINT('Ctrl Pts',(-0.314762517258735,6.76223400523443,
140.8176281402));
#44046=CARTESIAN_POINT('Ctrl Pts',(-0.500580446819129,6.75102239665092,
140.826377207799));
#44047=CARTESIAN_POINT('Ctrl Pts',(-0.685621118842215,6.73217741012502,
140.835126275398));
#44048=CARTESIAN_POINT('Ctrl Pts',(-0.870660665414065,6.71333253821777,
140.843875289784));
#44049=CARTESIAN_POINT('Ctrl Pts',(-1.05492267885442,6.68685441030619,140.85262430417));
#44050=CARTESIAN_POINT('Ctrl Pts',(-1.23778137635204,6.65283295028186,140.861373318555));
#44051=CARTESIAN_POINT('Ctrl Pts',(-1.42999922978786,6.61707018861878,140.870570128923));
#44052=CARTESIAN_POINT('Ctrl Pts',(-1.62066601233622,6.57297172934431,140.87976693929));
#44053=CARTESIAN_POINT('Ctrl Pts',(-1.809066285003,6.52070304311318,140.888963749658));
#44054=CARTESIAN_POINT('Ctrl Pts',(-1.98831342545444,6.47097374915056,140.897713747395));
#44055=CARTESIAN_POINT('Ctrl Pts',(-2.16550875896621,6.41384933989556,140.906463745133));
#44056=CARTESIAN_POINT('Ctrl Pts',(-2.34005036713933,6.34952386240505,140.915213742871));
#44057=CARTESIAN_POINT('Ctrl Pts',(-2.51458843547,6.28519968948631,140.923963563152));
#44058=CARTESIAN_POINT('Ctrl Pts',(-2.68647261717956,6.21367483971142,140.932713383433));
#44059=CARTESIAN_POINT('Ctrl Pts',(-2.85511905908622,6.13519226743895,140.941463203713));
#44060=CARTESIAN_POINT('Ctrl Pts',(-3.02376230488772,6.05671118252993,140.950212858172));
#44061=CARTESIAN_POINT('Ctrl Pts',(-3.18916767379789,5.97127275992695,140.958962512631));
#44062=CARTESIAN_POINT('Ctrl Pts',(-3.35077334102669,5.87916720438064,140.967712167089));
#44063=CARTESIAN_POINT('Ctrl Pts',(-3.5123761603725,5.78706327195715,140.976461667357));
#44064=CARTESIAN_POINT('Ctrl Pts',(-3.67017916302182,5.68829258362374,140.985211167626));
#44065=CARTESIAN_POINT('Ctrl Pts',(-3.82364636566345,5.58319061741122,140.993960667894));
#44066=CARTESIAN_POINT('Ctrl Pts',(-3.9771110677869,5.47809036367781,141.002710025603));
#44067=CARTESIAN_POINT('Ctrl Pts',(-4.12623987481828,5.36665920043301,141.011459383311));
#44068=CARTESIAN_POINT('Ctrl Pts',(-4.27052628213839,5.24927559512408,141.02020874102));
#44069=CARTESIAN_POINT('Ctrl Pts',(-4.41481053024887,5.13189374643114,141.028957967796));
#44070=CARTESIAN_POINT('Ctrl Pts',(-4.55425230136439,5.00855981477436,141.037707194573));
#44071=CARTESIAN_POINT('Ctrl Pts',(-4.68837800630456,4.87969268192165,141.046456421349));
#44072=CARTESIAN_POINT('Ctrl Pts',(-4.82250188228803,4.75082730631903,141.05520552882));
#44073=CARTESIAN_POINT('Ctrl Pts',(-4.95130963052875,4.61642907903623,141.063954636291));
#44074=CARTESIAN_POINT('Ctrl Pts',(-5.07436379033277,4.47695444731792,141.072703743762));
#44075=CARTESIAN_POINT('Ctrl Pts',(-5.19741643562717,4.33748153220692,141.081452743552));
#44076=CARTESIAN_POINT('Ctrl Pts',(-5.31471544462688,4.19293255254697,141.090201743341));
#44077=CARTESIAN_POINT('Ctrl Pts',(-5.42586245275545,4.04379841779714,141.098950743131));
#44078=CARTESIAN_POINT('Ctrl Pts',(-5.53702160019067,3.89464799484464,141.107700698473));
#44079=CARTESIAN_POINT('Ctrl Pts',(-5.64202723081164,3.74091164443981,141.116450653815));
#44080=CARTESIAN_POINT('Ctrl Pts',(-5.74052265232879,3.58311159163374,141.125200609157));
#44081=CARTESIAN_POINT('Ctrl Pts',(-5.8390142706684,3.42531763191916,141.13395022664));
#44082=CARTESIAN_POINT('Ctrl Pts',(-5.93099603115672,3.26346052695737,141.142699844122));
#44083=CARTESIAN_POINT('Ctrl Pts',(-6.01615550622695,3.0980900446719,141.151449461605));
#44084=CARTESIAN_POINT('Ctrl Pts',(-6.10131214578758,2.93272506863916,141.160198787756));
#44085=CARTESIAN_POINT('Ctrl Pts',(-6.17964682328721,2.76384720416956,141.168948113907));
#44086=CARTESIAN_POINT('Ctrl Pts',(-6.2508934828855,2.59203002791627,141.177697440058));
#44087=CARTESIAN_POINT('Ctrl Pts',(-6.32213814889323,2.4202176593705,141.18644652139));
#44088=CARTESIAN_POINT('Ctrl Pts',(-6.38629508412583,2.24546640831925,141.195195602721));
#44089=CARTESIAN_POINT('Ctrl Pts',(-6.44314639819814,2.06836976660036,141.203944684053));
#44090=CARTESIAN_POINT('Ctrl Pts',(-6.50000285283705,1.8912571115826,141.212694556487));
#44091=CARTESIAN_POINT('Ctrl Pts',(-6.54955227673256,1.71179891440229,141.221444428922));
#44092=CARTESIAN_POINT('Ctrl Pts',(-6.59162635926393,1.53060476278395,141.230194301356));
#44093=CARTESIAN_POINT('Ctrl Pts',(-6.63369752055202,1.34942319164669,141.238943566279));
#44094=CARTESIAN_POINT('Ctrl Pts',(-6.66829431424257,1.16650618642687,141.247692831201));
#44095=CARTESIAN_POINT('Ctrl Pts',(-6.69529923745418,0.982474997618482,
141.256442096124));
#44096=CARTESIAN_POINT('Ctrl Pts',(-6.72230554731444,0.798434359177678,
141.265191810303));
#44097=CARTESIAN_POINT('Ctrl Pts',(-6.74171916496703,0.613279706240286,
141.273941524483));
#44098=CARTESIAN_POINT('Ctrl Pts',(-6.75347414817275,0.427639953655338,
141.282691238663));
#44099=CARTESIAN_POINT('Ctrl Pts',(-6.7624883775873,0.285283364200832,141.289400897838));
#44100=CARTESIAN_POINT('Ctrl Pts',(-6.76699999999982,0.142641701109683,
141.296110557014));
#44101=CARTESIAN_POINT('Ctrl Pts',(-6.767,8.4381075191075E-12,141.30282021619));
#44102=CARTESIAN_POINT('Ctrl Pts',(-6.76699803346499,-0.00515898061969993,
141.30282021619));
#44103=CARTESIAN_POINT('Ctrl Pts',(-6.76684551847906,-0.205211798397617,
141.3121990332));
#44104=CARTESIAN_POINT('Ctrl Pts',(-6.7578179217659,-0.404900345085272,
141.32157785021));
#44105=CARTESIAN_POINT('Ctrl Pts',(-6.74003529756579,-0.603500776774318,
141.330956667221));
#44106=CARTESIAN_POINT('Ctrl Pts',(-6.72210344891169,-0.803767781442086,
141.340414187398));
#44107=CARTESIAN_POINT('Ctrl Pts',(-6.69526909379508,-1.00292819836621,
141.349871707575));
#44108=CARTESIAN_POINT('Ctrl Pts',(-6.65970477407413,-1.20025885631984,
141.359329227753));
#44109=CARTESIAN_POINT('Ctrl Pts',(-6.6239923058968,-1.39841152443993,141.368826144635));
#44110=CARTESIAN_POINT('Ctrl Pts',(-6.57947708712788,-1.59471904311785,
141.378323061518));
#44111=CARTESIAN_POINT('Ctrl Pts',(-6.52638211645565,-1.78847014792195,
141.3878199784));
#44112=CARTESIAN_POINT('Ctrl Pts',(-6.47303707337058,-1.98313380255237,
141.397361624885));
#44113=CARTESIAN_POINT('Ctrl Pts',(-6.41103134849624,-2.17521679241845,
141.40690327137));
#44114=CARTESIAN_POINT('Ctrl Pts',(-6.34063841920463,-2.36402060839288,
141.416444917855));
#44115=CARTESIAN_POINT('Ctrl Pts',(-6.32600128567985,-2.40327947561456,
141.418428957375));
#44116=CARTESIAN_POINT('Ctrl Pts',(-6.31100167596679,-2.44239664350668,
141.420412996895));
#44117=CARTESIAN_POINT('Ctrl Pts',(-6.29564229928631,-2.48136596241606,
141.422397036415));
#44118=CARTESIAN_POINT('Ctrl Pts',(-6.23250708629875,-2.64155060405269,
141.430552494822));
#44119=CARTESIAN_POINT('Ctrl Pts',(-6.16315136132801,-2.79958535426697,
141.438707953228));
#44120=CARTESIAN_POINT('Ctrl Pts',(-6.08774025173248,-2.95494629857062,
141.446863411635));
#44121=CARTESIAN_POINT('Ctrl Pts',(-6.01242092736996,-3.11011814818318,
141.455008943777));
#44122=CARTESIAN_POINT('Ctrl Pts',(-5.93106104695123,-3.2626223446625,141.463154475919));
#44123=CARTESIAN_POINT('Ctrl Pts',(-5.84387490999866,-3.41195179278491,
141.471300008061));
#44124=CARTESIAN_POINT('Ctrl Pts',(-5.75677655653961,-3.5611308883272,141.479437338861));
#44125=CARTESIAN_POINT('Ctrl Pts',(-5.6638638079716,-3.70714128589627,141.487574669662));
#44126=CARTESIAN_POINT('Ctrl Pts',(-5.56539828393895,-3.84949749202794,
141.495712000462));
#44127=CARTESIAN_POINT('Ctrl Pts',(-5.46701120723309,-3.99174028319601,
141.503842848264));
#44128=CARTESIAN_POINT('Ctrl Pts',(-5.36308037052578,-4.13033438046218,
141.511973696066));
#44129=CARTESIAN_POINT('Ctrl Pts',(-5.25391238953515,-4.26482046551658,
141.520104543868));
#44130=CARTESIAN_POINT('Ctrl Pts',(-5.14480844987737,-4.39922765685088,
141.528230621862));
#44131=CARTESIAN_POINT('Ctrl Pts',(-5.03047371408059,-4.529531352152,141.536356699856));
#44132=CARTESIAN_POINT('Ctrl Pts',(-4.91125702156631,-4.6553027257221,141.54448277785));
#44133=CARTESIAN_POINT('Ctrl Pts',(-4.79161760843506,-4.78152006161099,
141.552637669432));
#44134=CARTESIAN_POINT('Ctrl Pts',(-4.66706177056764,-4.90317257289954,
141.560792561014));
#44135=CARTESIAN_POINT('Ctrl Pts',(-4.53798203647573,-5.01986135631489,
141.568947452596));
#44136=CARTESIAN_POINT('Ctrl Pts',(-4.40940566821507,-5.13609509427424,
141.577070542953));
#44137=CARTESIAN_POINT('Ctrl Pts',(-4.2763409083398,-5.24740351417476,141.585193633309));
#44138=CARTESIAN_POINT('Ctrl Pts',(-4.13921143707729,-5.35343045898315,
141.593316723665));
#44139=CARTESIAN_POINT('Ctrl Pts',(-4.00207119778253,-5.45946572951139,
141.601440451884));
#44140=CARTESIAN_POINT('Ctrl Pts',(-3.86086590071739,-5.5602184750565,141.609564180102));
#44141=CARTESIAN_POINT('Ctrl Pts',(-3.71605079975729,-5.65537403304355,
141.61768790832));
#44142=CARTESIAN_POINT('Ctrl Pts',(-3.57119677635348,-5.75055516631124,
141.625813819981));
#44143=CARTESIAN_POINT('Ctrl Pts',(-3.42273132276988,-5.84013591572219,
141.633939731641));
#44144=CARTESIAN_POINT('Ctrl Pts',(-3.27113699773397,-5.92384602619413,
141.642065643301));
#44145=CARTESIAN_POINT('Ctrl Pts',(-3.11857321123165,-6.00809147152397,
141.650243521011));
#44146=CARTESIAN_POINT('Ctrl Pts',(-2.96284072425621,-6.08639074903449,
141.658421398721));
#44147=CARTESIAN_POINT('Ctrl Pts',(-2.80445396374326,-6.15851662052192,
141.666599276431));
#44148=CARTESIAN_POINT('Ctrl Pts',(-2.64682314888578,-6.23029825086811,
141.674738122905));
#44149=CARTESIAN_POINT('Ctrl Pts',(-2.48656370337479,-6.29596519292917,
141.682876969378));
#44150=CARTESIAN_POINT('Ctrl Pts',(-2.32419978976134,-6.35534297558152,
141.691015815852));
#44151=CARTESIAN_POINT('Ctrl Pts',(-2.16066791008213,-6.41514789277168,
141.69921320918));
#44152=CARTESIAN_POINT('Ctrl Pts',(-1.99500153066225,-6.46857271123967,
141.707410602509));
#44153=CARTESIAN_POINT('Ctrl Pts',(-1.82774818014213,-6.51549120097535,
141.715607995837));
#44154=CARTESIAN_POINT('Ctrl Pts',(-1.66049482962201,-6.56240969071102,
141.723805389165));
#44155=CARTESIAN_POINT('Ctrl Pts',(-1.49165488423451,-6.60282182449964,
141.732002782494));
#44156=CARTESIAN_POINT('Ctrl Pts',(-1.32178227966414,-6.63665432316358,
141.740200175822));
#44157=CARTESIAN_POINT('Ctrl Pts',(-1.15131252789826,-6.67060575202081,
141.748426385159));
#44158=CARTESIAN_POINT('Ctrl Pts',(-0.979295518889764,-6.69803236714227,
141.756652594496));
#44159=CARTESIAN_POINT('Ctrl Pts',(-0.806271845541212,-6.71879562950739,
141.764878803833));
#44160=CARTESIAN_POINT('Ctrl Pts',(-0.63344255687744,-6.73953556523672,
141.773095771376));
#44161=CARTESIAN_POINT('Ctrl Pts',(-0.45960920873851,-6.75362701250998,
141.781312738919));
#44162=CARTESIAN_POINT('Ctrl Pts',(-0.285323950504457,-6.7609821212061,
141.789529706462));
#44163=CARTESIAN_POINT('Ctrl Pts',(-0.11119951384423,-6.76833044298193,
141.797739091806));
#44164=CARTESIAN_POINT('Ctrl Pts',(0.0633756463752362,-6.76895479045135,
141.805948477149));
#44165=CARTESIAN_POINT('Ctrl Pts',(0.237842774754304,-6.76281892515963,
141.814157862493));
#44166=CARTESIAN_POINT('Ctrl Pts',(0.412183919450204,-6.75668749061034,
141.822361319793));
#44167=CARTESIAN_POINT('Ctrl Pts',(0.586416830726529,-6.7438055791375,141.830564777094));
#44168=CARTESIAN_POINT('Ctrl Pts',(0.759981165075346,-6.72418899412641,
141.838768234394));
#44169=CARTESIAN_POINT('Ctrl Pts',(0.933454984232804,-6.70458263932161,
141.846967413526));
#44170=CARTESIAN_POINT('Ctrl Pts',(1.10626056555226,-6.67824864806033,141.855166592658));
#44171=CARTESIAN_POINT('Ctrl Pts',(1.27784101356949,-6.64525479903064,141.86336577179));
#44172=CARTESIAN_POINT('Ctrl Pts',(1.44938913213254,-6.61226716675316,141.87156340602));
#44173=CARTESIAN_POINT('Ctrl Pts',(1.61971222421063,-6.57262223780582,141.87976104025));
#44174=CARTESIAN_POINT('Ctrl Pts',(1.78826163004924,-6.52643925448584,141.887958674479));
#44175=CARTESIAN_POINT('Ctrl Pts',(1.95679886980705,-6.4802596047042,141.896155716995));
#44176=CARTESIAN_POINT('Ctrl Pts',(2.12356233213615,-6.4275429343452,141.904352759511));
#44177=CARTESIAN_POINT('Ctrl Pts',(2.2880166661251,-6.36845889800145,141.912549802026));
#44178=CARTESIAN_POINT('Ctrl Pts',(2.45248901892003,-6.30936838798344,141.920747742669));
#44179=CARTESIAN_POINT('Ctrl Pts',(2.61465140169011,-6.24390924335047,141.928945683312));
#44180=CARTESIAN_POINT('Ctrl Pts',(2.77398660788165,-6.17230000075282,141.937143623955));
#44181=CARTESIAN_POINT('Ctrl Pts',(2.93336823100454,-6.10066989722069,141.945343952791));
#44182=CARTESIAN_POINT('Ctrl Pts',(3.08992070995639,-6.02288627402341,141.953544281627));
#44183=CARTESIAN_POINT('Ctrl Pts',(3.24314964103395,-5.93921454452198,141.961744610463));
#44184=CARTESIAN_POINT('Ctrl Pts',(3.39653824063363,-5.85545562690731,141.969953484254));
#44185=CARTESIAN_POINT('Ctrl Pts',(3.5465960581434,-5.76579651719551,141.978162358046));
#44186=CARTESIAN_POINT('Ctrl Pts',(3.69285513820632,-5.67054758627623,141.986371231837));
#44187=CARTESIAN_POINT('Ctrl Pts',(3.83919271390396,-5.57524753630653,141.99458451124));
#44188=CARTESIAN_POINT('Ctrl Pts',(3.98172719538239,-5.47435189156545,142.002797790644));
#44189=CARTESIAN_POINT('Ctrl Pts',(4.12002225636718,-5.36821251507791,142.011011070047));
#44190=CARTESIAN_POINT('Ctrl Pts',(4.25851959561478,-5.26191789307011,142.019236362663));
#44191=CARTESIAN_POINT('Ctrl Pts',(4.39276484658754,-5.15036444097716,142.027461655278));
#44192=CARTESIAN_POINT('Ctrl Pts',(4.5223562660631,-5.03394306709957,142.035686947894));
#44193=CARTESIAN_POINT('Ctrl Pts',(4.63955613788398,-4.92865391947789,142.043125737006));
#44194=CARTESIAN_POINT('Ctrl Pts',(4.75294996887623,-4.8193839025031,142.050564526118));
#44195=CARTESIAN_POINT('Ctrl Pts',(4.86226871520141,-4.70644578649044,142.05800331523));
#44196=CARTESIAN_POINT('Ctrl Pts',(4.98315908712159,-4.58155292677796,142.066229516249));
#44197=CARTESIAN_POINT('Ctrl Pts',(5.0994033158173,-4.45182470217961,142.074455717268));
#44198=CARTESIAN_POINT('Ctrl Pts',(5.21059208957854,-4.31764045237923,142.082681918286));
#44199=CARTESIAN_POINT('Ctrl Pts',(5.32165596618666,-4.18360693030277,142.090898878902));
#44200=CARTESIAN_POINT('Ctrl Pts',(5.42767546902388,-4.04512762378935,142.099115839518));
#44201=CARTESIAN_POINT('Ctrl Pts',(5.52827763207056,-3.90261904658247,142.107332800134));
#44202=CARTESIAN_POINT('Ctrl Pts',(5.62878698144326,-3.76024194512348,142.115542179935));
#44203=CARTESIAN_POINT('Ctrl Pts',(5.7238887390716,-3.61384326731823,142.123751559737));
#44204=CARTESIAN_POINT('Ctrl Pts',(5.81324974211918,-3.46387303978527,142.131960939538));
#44205=CARTESIAN_POINT('Ctrl Pts',(5.90254623208519,-3.31401108142111,142.140164392679));
#44206=CARTESIAN_POINT('Ctrl Pts',(5.9861100397044,-3.16058301597431,142.148367845819));
#44207=CARTESIAN_POINT('Ctrl Pts',(6.06365088531202,-3.00406839819848,142.15657129896));
#44208=CARTESIAN_POINT('Ctrl Pts',(6.14115130575638,-2.84763537779144,142.16477047531));
#44209=CARTESIAN_POINT('Ctrl Pts',(6.21263486082306,-2.6881193313531,142.17296965166));
#44210=CARTESIAN_POINT('Ctrl Pts',(6.27785682638096,-2.52602507261152,142.18116882801));
#44211=CARTESIAN_POINT('Ctrl Pts',(6.34306651944176,-2.36396131435091,142.189366461561));
#44212=CARTESIAN_POINT('Ctrl Pts',(6.40201683036049,-2.19932064016115,142.197564095113));
#44213=CARTESIAN_POINT('Ctrl Pts',(6.45451075406156,-2.03262882142897,142.205761728664));
#44214=CARTESIAN_POINT('Ctrl Pts',(6.50700089691177,-1.86594900859882,142.213958771785));
#44215=CARTESIAN_POINT('Ctrl Pts',(6.55303547007303,-1.69721868729407,142.222155814905));
#44216=CARTESIAN_POINT('Ctrl Pts',(6.59246705224555,-1.52697975266763,142.230352858026));
#44217=CARTESIAN_POINT('Ctrl Pts',(6.63190296100066,-1.35672213878032,142.238550800557));
#44218=CARTESIAN_POINT('Ctrl Pts',(6.66473435438957,-1.18495593128793,142.246748743088));
#44219=CARTESIAN_POINT('Ctrl Pts',(6.69086472824702,-1.01223425564438,142.254946685619));
#44220=CARTESIAN_POINT('Ctrl Pts',(6.7170027183976,-0.839462236331058,142.263147017628));
#44221=CARTESIAN_POINT('Ctrl Pts',(6.73643574490875,-0.665734548697585,
142.271347349636));
#44222=CARTESIAN_POINT('Ctrl Pts',(6.74911905885693,-0.491610546443122,
142.279547681645));
#44223=CARTESIAN_POINT('Ctrl Pts',(6.76181559224628,-0.317305059916308,
142.287756560615));
#44224=CARTESIAN_POINT('Ctrl Pts',(6.7677483320653,-0.142602791727504,142.295965439586));
#44225=CARTESIAN_POINT('Ctrl Pts',(6.76692464638334,0.0319347799383077,
142.304174318557));
#44226=CARTESIAN_POINT('Ctrl Pts',(6.7661005185278,0.206566047420996,142.312387604244));
#44227=CARTESIAN_POINT('Ctrl Pts',(6.75851275017981,0.381032084133073,142.320600889932));
#44228=CARTESIAN_POINT('Ctrl Pts',(6.74422072020736,0.554775519580439,142.328814175619));
#44229=CARTESIAN_POINT('Ctrl Pts',(6.72990778275652,0.728773120260453,142.337039476331));
#44230=CARTESIAN_POINT('Ctrl Pts',(6.70887102724182,0.902045651135109,142.345264777043));
#44231=CARTESIAN_POINT('Ctrl Pts',(6.68122138693208,1.07404365777253,142.353490077755));
#44232=CARTESIAN_POINT('Ctrl Pts',(6.65621562258789,1.22959510703063,142.360928870049));
#44233=CARTESIAN_POINT('Ctrl Pts',(6.62580187104475,1.38410407259627,142.368367662343));
#44234=CARTESIAN_POINT('Ctrl Pts',(6.59009727604772,1.53717497124708,142.375806454637));
#44235=CARTESIAN_POINT('Ctrl Pts',(6.55096306011718,1.70494916392396,142.383959783471));
#44236=CARTESIAN_POINT('Ctrl Pts',(6.50535651729762,1.87149037648807,142.392113112305));
#44237=CARTESIAN_POINT('Ctrl Pts',(6.45336732036248,2.03625617948175,142.400266441139));
#44238=CARTESIAN_POINT('Ctrl Pts',(6.40143939672394,2.20082779321088,142.408410160643));
#44239=CARTESIAN_POINT('Ctrl Pts',(6.3431439031148,2.3636278176858,142.416553880147));
#44240=CARTESIAN_POINT('Ctrl Pts',(6.27862157673203,2.52412362934049,142.424697599652));
#44241=CARTESIAN_POINT('Ctrl Pts',(6.21416172815082,2.68446403082892,142.432833433487));
#44242=CARTESIAN_POINT('Ctrl Pts',(6.14348718732535,2.84250432495502,142.440969267323));
#44243=CARTESIAN_POINT('Ctrl Pts',(6.06678858213726,2.99772668861739,142.449105101158));
#44244=CARTESIAN_POINT('Ctrl Pts',(5.98742971644171,3.15833287800792,142.457523123143));
#44245=CARTESIAN_POINT('Ctrl Pts',(5.9016214831714,3.31592176199994,142.465941145128));
#44246=CARTESIAN_POINT('Ctrl Pts',(5.80962999299254,3.46994068314164,142.474359167112));
#44247=CARTESIAN_POINT('Ctrl Pts',(5.72083909529676,3.61860093686423,142.482484307029));
#44248=CARTESIAN_POINT('Ctrl Pts',(5.62628816602592,3.7639351178533,142.490609446946));
#44249=CARTESIAN_POINT('Ctrl Pts',(5.52626372034169,3.90547030371955,142.498734586863));
#44250=CARTESIAN_POINT('Ctrl Pts',(5.42626627486101,4.0469672841371,142.506857533511));
#44251=CARTESIAN_POINT('Ctrl Pts',(5.32079846526247,4.18466701266856,142.51498048016));
#44252=CARTESIAN_POINT('Ctrl Pts',(5.21019023318417,4.31812537266257,142.523103426808));
#44253=CARTESIAN_POINT('Ctrl Pts',(5.09959081698206,4.45157309554256,142.531225726028));
#44254=CARTESIAN_POINT('Ctrl Pts',(4.98385202789909,4.58077984192608,142.539348025249));
#44255=CARTESIAN_POINT('Ctrl Pts',(4.86334417652548,4.70533446427092,142.547470324469));
#44256=CARTESIAN_POINT('Ctrl Pts',(4.7428230054427,4.82990285361373,142.555593521446));
#44257=CARTESIAN_POINT('Ctrl Pts',(4.61753197770552,4.94981783330412,142.563716718422));
#44258=CARTESIAN_POINT('Ctrl Pts',(4.48787830738047,5.06470505539502,142.571839915398));
#44259=CARTESIAN_POINT('Ctrl Pts',(4.35813809382838,5.17966896417685,142.579968534571));
#44260=CARTESIAN_POINT('Ctrl Pts',(4.22402969654757,5.28959817118007,142.588097153744));
#44261=CARTESIAN_POINT('Ctrl Pts',(4.08599388627922,5.39415822545918,142.596225772917));
#44262=CARTESIAN_POINT('Ctrl Pts',(3.94790277331778,5.49876017069816,142.604357648742));
#44263=CARTESIAN_POINT('Ctrl Pts',(3.80588141029657,5.59798846612755,142.612489524566));
#44264=CARTESIAN_POINT('Ctrl Pts',(3.66039937943157,5.6915521066803,142.620621400391));
#44265=CARTESIAN_POINT('Ctrl Pts',(3.51477710291696,5.78520594320757,142.628761115398));
#44266=CARTESIAN_POINT('Ctrl Pts',(3.36568781175504,5.8731840362202,142.636900830405));
#44267=CARTESIAN_POINT('Ctrl Pts',(3.21362597947884,5.95524114239035,142.645040545412));
#44268=CARTESIAN_POINT('Ctrl Pts',(3.17565848841867,5.97572953450231,142.647072906539));
#44269=CARTESIAN_POINT('Ctrl Pts',(3.13750578286208,5.99584903144824,142.649105267665));
#44270=CARTESIAN_POINT('Ctrl Pts',(3.09917575053256,6.0155962852664,142.651137628792));
#44271=CARTESIAN_POINT('Origin',(0.,0.,-3.69717978381041));
#44272=CARTESIAN_POINT('',(3.09917575053269,6.01559628526634,145.045580110739));
#44273=CARTESIAN_POINT('',(3.0991757505327,6.01559628526633,144.651598619988));
#44274=CARTESIAN_POINT('',(3.09917575053259,6.01559628526639,-3.69717978381041));
#44275=CARTESIAN_POINT('',(-6.76789295125885,-0.00152640326764282,143.695634344439));
#44276=CARTESIAN_POINT('Ctrl Pts',(-6.76699890218547,-0.00385458436745586,
143.69717978381));
#44277=CARTESIAN_POINT('Ctrl Pts',(-6.76688822840503,-0.198150331811941,
143.706274939033));
#44278=CARTESIAN_POINT('Ctrl Pts',(-6.75840555936475,-0.392127566114781,
143.715370094256));
#44279=CARTESIAN_POINT('Ctrl Pts',(-6.74165716558243,-0.585104829710985,
143.72446524948));
#44280=CARTESIAN_POINT('Ctrl Pts',(-6.72480840539411,-0.779238528642958,
143.73361490832));
#44281=CARTESIAN_POINT('Ctrl Pts',(-6.69959463942678,-0.972360037544215,
143.74276456716));
#44282=CARTESIAN_POINT('Ctrl Pts',(-6.66617399448702,-1.1637926255244,143.751914226001));
#44283=CARTESIAN_POINT('Ctrl Pts',(-6.63265004861101,-1.35581691858995,
143.761092165813));
#44284=CARTESIAN_POINT('Ctrl Pts',(-6.5908685217642,-1.54614165088267,143.770270105625));
#44285=CARTESIAN_POINT('Ctrl Pts',(-6.54103761856071,-1.73410376638008,
143.779448045438));
#44286=CARTESIAN_POINT('Ctrl Pts',(-6.4910067296831,-1.9228202276341,143.788662818949));
#44287=CARTESIAN_POINT('Ctrl Pts',(-6.43286183228391,-2.10915489027211,
143.79787759246));
#44288=CARTESIAN_POINT('Ctrl Pts',(-6.3668609488963,-2.29245952143529,143.807092365972));
#44289=CARTESIAN_POINT('Ctrl Pts',(-6.34417735930147,-2.35545878463785,
143.810259356015));
#44290=CARTESIAN_POINT('Ctrl Pts',(-6.32056622121258,-2.41810034992914,
143.813426346058));
#44291=CARTESIAN_POINT('Ctrl Pts',(-6.29603925657947,-2.480358578837,143.816593336102));
#44292=CARTESIAN_POINT('Ctrl Pts',(-6.23234122283766,-2.64204702357524,
143.824818203779));
#44293=CARTESIAN_POINT('Ctrl Pts',(-6.16232128426089,-2.80150714443053,
143.833043071457));
#44294=CARTESIAN_POINT('Ctrl Pts',(-6.08615524134657,-2.95820948856392,
143.841267939134));
#44295=CARTESIAN_POINT('Ctrl Pts',(-6.01007500800483,-3.11473528996703,
143.849483540578));
#44296=CARTESIAN_POINT('Ctrl Pts',(-5.92786261372773,-3.26850918163377,
143.857699142021));
#44297=CARTESIAN_POINT('Ctrl Pts',(-5.83974274512548,-3.41901940192716,
143.865914743465));
#44298=CARTESIAN_POINT('Ctrl Pts',(-5.75170444836886,-3.56939029613381,
143.874122739793));
#44299=CARTESIAN_POINT('Ctrl Pts',(-5.6577697480437,-3.71650322799807,143.882330736121));
#44300=CARTESIAN_POINT('Ctrl Pts',(-5.55821031525164,-3.85986879199673,
143.890538732449));
#44301=CARTESIAN_POINT('Ctrl Pts',(-5.458723046787,-4.00313043937784,143.89874077932));
#44302=CARTESIAN_POINT('Ctrl Pts',(-5.35361937030534,-4.14264983562056,
143.906942826192));
#44303=CARTESIAN_POINT('Ctrl Pts',(-5.24321558859412,-4.27796438642535,
143.915144873063));
#44304=CARTESIAN_POINT('Ctrl Pts',(-5.13286966152387,-4.41320802865587,
143.923342621835));
#44305=CARTESIAN_POINT('Ctrl Pts',(-5.01722938852348,-4.5442509377589,143.931540370606));
#44306=CARTESIAN_POINT('Ctrl Pts',(-4.89665292325319,-4.67066153228812,
143.939738119378));
#44307=CARTESIAN_POINT('Ctrl Pts',(-4.77609945552222,-4.79704801653503,
143.947934304593));
#44308=CARTESIAN_POINT('Ctrl Pts',(-4.65061191370683,-4.91880368243128,
143.956130489809));
#44309=CARTESIAN_POINT('Ctrl Pts',(-4.52058728115179,-5.03553171308539,
143.964326675025));
#44310=CARTESIAN_POINT('Ctrl Pts',(-4.39057226752552,-5.15225110846332,
143.972522253905));
#44311=CARTESIAN_POINT('Ctrl Pts',(-4.25602109801748,-5.26394336894143,
143.980717832785));
#44312=CARTESIAN_POINT('Ctrl Pts',(-4.11736595633787,-5.37025014143568,
143.988913411665));
#44313=CARTESIAN_POINT('Ctrl Pts',(-3.97869584539161,-5.47656839085322,
143.997109875344));
#44314=CARTESIAN_POINT('Ctrl Pts',(-3.83592116437346,-5.57749977554788,
144.005306339022));
#44315=CARTESIAN_POINT('Ctrl Pts',(-3.68950539311895,-5.6727276467451,144.013502802701));
#44316=CARTESIAN_POINT('Ctrl Pts',(-3.54304717603013,-5.76798312443859,
144.021701642528));
#44317=CARTESIAN_POINT('Ctrl Pts',(-3.39294606691518,-5.85753159959245,
144.029900482356));
#44318=CARTESIAN_POINT('Ctrl Pts',(-3.23969263340999,-5.9411009620296,144.038099322184));
#44319=CARTESIAN_POINT('Ctrl Pts',(-3.08627912233369,-6.02475761504323,
144.046306725933));
#44320=CARTESIAN_POINT('Ctrl Pts',(-2.92970702395475,-6.10242250591931,
144.054514129682));
#44321=CARTESIAN_POINT('Ctrl Pts',(-2.77049041122545,-6.17387008944211,
144.062721533431));
#44322=CARTESIAN_POINT('Ctrl Pts',(-2.61118851365254,-6.24535594407168,
144.0709333335));
#44323=CARTESIAN_POINT('Ctrl Pts',(-2.44923961032437,-6.31061771827833,
144.079145133569));
#44324=CARTESIAN_POINT('Ctrl Pts',(-2.28517555503982,-6.36947891767046,
144.087356933638));
#44325=CARTESIAN_POINT('Ctrl Pts',(-2.12086997454152,-6.42842676897266,
144.095580822624));
#44326=CARTESIAN_POINT('Ctrl Pts',(-1.95444336144118,-6.48095510677064,
144.10380471161));
#44327=CARTESIAN_POINT('Ctrl Pts',(-1.78644170893756,-6.52693764491191,
144.112028600597));
#44328=CARTESIAN_POINT('Ctrl Pts',(-1.63121108639254,-6.56942471522044,
144.119627331847));
#44329=CARTESIAN_POINT('Ctrl Pts',(-1.47463612428513,-6.60632386487549,
144.127226063098));
#44330=CARTESIAN_POINT('Ctrl Pts',(-1.31715250548996,-6.63757472856476,
144.134824794349));
#44331=CARTESIAN_POINT('Ctrl Pts',(-1.14669261750365,-6.67140058781731,
144.143049642671));
#44332=CARTESIAN_POINT('Ctrl Pts',(-0.974689627855077,-6.6987033178731,
144.151274490993));
#44333=CARTESIAN_POINT('Ctrl Pts',(-0.801683994273585,-6.7193445940304,
144.159499339316));
#44334=CARTESIAN_POINT('Ctrl Pts',(-0.62887320339435,-6.73996262353416,
144.167714924635));
#44335=CARTESIAN_POINT('Ctrl Pts',(-0.455062370104183,-6.75393409596503,
144.175930509954));
#44336=CARTESIAN_POINT('Ctrl Pts',(-0.280803496358166,-6.76117137753755,
144.184146095274));
#44337=CARTESIAN_POINT('Ctrl Pts',(-0.106705864663507,-6.76840196244033,
144.192354078697));
#44338=CARTESIAN_POINT('Ctrl Pts',(0.0678386256527802,-6.76891075117247,
144.200562062121));
#44339=CARTESIAN_POINT('Ctrl Pts',(0.242271380931179,-6.76266172287079,
144.208770045544));
#44340=CARTESIAN_POINT('Ctrl Pts',(0.416577768971264,-6.75641722165719,
144.216972082721));
#44341=CARTESIAN_POINT('Ctrl Pts',(0.590772226114278,-6.74342466747038,
144.225174119898));
#44342=CARTESIAN_POINT('Ctrl Pts',(0.764294586920538,-6.72370008138406,
144.233376157075));
#44343=CARTESIAN_POINT('Ctrl Pts',(0.937726084850511,-6.70398582383762,
144.241573899354));
#44344=CARTESIAN_POINT('Ctrl Pts',(1.11048583192282,-6.67754659747403,144.249771641634));
#44345=CARTESIAN_POINT('Ctrl Pts',(1.28201712896983,-6.6444503972133,144.257969383914));
#44346=CARTESIAN_POINT('Ctrl Pts',(1.45351581217918,-6.61136048964737,144.266165567528));
#44347=CARTESIAN_POINT('Ctrl Pts',(1.62378615750544,-6.57161619110681,144.274361751143));
#44348=CARTESIAN_POINT('Ctrl Pts',(1.79227972119302,-6.52533695689351,144.282557934757));
#44349=CARTESIAN_POINT('Ctrl Pts',(1.96076088140341,-6.47906112947756,144.290753515019));
#44350=CARTESIAN_POINT('Ctrl Pts',(2.12746517421121,-6.426251418611,144.29894909528));
#44351=CARTESIAN_POINT('Ctrl Pts',(2.29185748577107,-6.3670776864206,144.307144675541));
#44352=CARTESIAN_POINT('Ctrl Pts',(2.45626760499938,-6.307897544282,144.315341143582));
#44353=CARTESIAN_POINT('Ctrl Pts',(2.61836490632715,-6.24235212892302,144.323537611623));
#44354=CARTESIAN_POINT('Ctrl Pts',(2.77763244260628,-6.17066017649498,144.331734079664));
#44355=CARTESIAN_POINT('Ctrl Pts',(2.93694620838337,-6.09894741453446,144.339932926837));
#44356=CARTESIAN_POINT('Ctrl Pts',(3.0934282459081,-6.02108470902992,144.348131774011));
#44357=CARTESIAN_POINT('Ctrl Pts',(3.24658443415898,-5.93733766193878,144.356330621185));
#44358=CARTESIAN_POINT('Ctrl Pts',(3.39990068551969,-5.85350309103974,144.364538036951));
#44359=CARTESIAN_POINT('Ctrl Pts',(3.54988382808291,-5.76377206462456,144.372745452717));
#44360=CARTESIAN_POINT('Ctrl Pts',(3.69606620807512,-5.66845513217889,144.380952868483));
#44361=CARTESIAN_POINT('Ctrl Pts',(3.84232693668147,-5.57308711320992,144.389164683136));
#44362=CARTESIAN_POINT('Ctrl Pts',(3.98478254927311,-5.47212742718527,144.397376497788));
#44363=CARTESIAN_POINT('Ctrl Pts',(4.12299704562277,-5.36592809882745,144.40558831244));
#44364=CARTESIAN_POINT('Ctrl Pts',(4.26141508383007,-5.25957237581388,144.413812220238));
#44365=CARTESIAN_POINT('Ctrl Pts',(4.39557924810398,-5.14796181940539,144.422036128036));
#44366=CARTESIAN_POINT('Ctrl Pts',(4.52508813375834,-5.03148749195698,144.430260035834));
#44367=CARTESIAN_POINT('Ctrl Pts',(4.6447519522449,-4.92386736452163,144.437858774754));
#44368=CARTESIAN_POINT('Ctrl Pts',(4.7604416149879,-4.81209539836844,144.445457513675));
#44369=CARTESIAN_POINT('Ctrl Pts',(4.87187081025728,-4.69650548899531,144.453056252595));
#44370=CARTESIAN_POINT('Ctrl Pts',(4.99139819418358,-4.57251500838341,144.461207234769));
#44371=CARTESIAN_POINT('Ctrl Pts',(5.1063768628517,-4.44376376357494,144.469358216943));
#44372=CARTESIAN_POINT('Ctrl Pts',(5.21640031467672,-4.31062138873743,144.477509199118));
#44373=CARTESIAN_POINT('Ctrl Pts',(5.32629596406532,-4.17763367110812,144.48565071317));
#44374=CARTESIAN_POINT('Ctrl Pts',(5.43124762368969,-4.04026525580476,144.493792227223));
#44375=CARTESIAN_POINT('Ctrl Pts',(5.53088471846351,-3.89892334254815,144.501933741276));
#44376=CARTESIAN_POINT('Ctrl Pts',(5.63042704281628,-3.75771586750114,144.510067511479));
#44377=CARTESIAN_POINT('Ctrl Pts',(5.72466465678561,-3.61254271560257,144.518201281682));
#44378=CARTESIAN_POINT('Ctrl Pts',(5.81326647395409,-3.46384495940587,144.526335051884));
#44379=CARTESIAN_POINT('Ctrl Pts',(5.90180265175817,-3.31525736377375,144.534462796302));
#44380=CARTESIAN_POINT('Ctrl Pts',(5.9847111598257,-3.16315067589078,144.54259054072));
#44381=CARTESIAN_POINT('Ctrl Pts',(6.06170357407764,-3.00799580784521,144.550718285138));
#44382=CARTESIAN_POINT('Ctrl Pts',(6.13865513669684,-2.85292326387987,144.558841717031));
#44383=CARTESIAN_POINT('Ctrl Pts',(6.20969669476124,-2.69480608758663,144.566965148925));
#44384=CARTESIAN_POINT('Ctrl Pts',(6.27458523912784,-2.53414069793273,144.575088580819));
#44385=CARTESIAN_POINT('Ctrl Pts',(6.33988541090072,-2.3724561102329,144.58326354457));
#44386=CARTESIAN_POINT('Ctrl Pts',(6.39895404780624,-2.20819119318812,144.591438508321));
#44387=CARTESIAN_POINT('Ctrl Pts',(6.45159209329951,-2.04187376242393,144.599613472072));
#44388=CARTESIAN_POINT('Ctrl Pts',(6.50388646344933,-1.87664222304505,144.607735061245));
#44389=CARTESIAN_POINT('Ctrl Pts',(6.54983387689869,-1.70938525286557,144.615856650418));
#44390=CARTESIAN_POINT('Ctrl Pts',(6.58928884327989,-1.54063673194792,144.62397823959));
#44391=CARTESIAN_POINT('Ctrl Pts',(6.62874901852584,-1.37186593276461,144.63210090098));
#44392=CARTESIAN_POINT('Ctrl Pts',(6.66171495610781,-1.20160354703293,144.640223562369));
#44393=CARTESIAN_POINT('Ctrl Pts',(6.68809209491408,-1.03039464767038,144.648346223758));
#44394=CARTESIAN_POINT('Ctrl Pts',(6.71447773903112,-0.859130541982949,
144.6564715043));
#44395=CARTESIAN_POINT('Ctrl Pts',(6.73427029802455,-0.68691967644226,144.664596784842));
#44396=CARTESIAN_POINT('Ctrl Pts',(6.7474269848792,-0.514313215583638,144.672722065384));
#44397=CARTESIAN_POINT('Ctrl Pts',(6.76072701110826,-0.339826243134885,
144.680935869172));
#44398=CARTESIAN_POINT('Ctrl Pts',(6.76724569597574,-0.164935388005928,
144.68914967296));
#44399=CARTESIAN_POINT('Ctrl Pts',(6.76699291840621,0.00978990501790505,
144.697363476749));
#44400=CARTESIAN_POINT('Ctrl Pts',(6.76674243241313,0.182931211112485,144.705502817604));
#44401=CARTESIAN_POINT('Ctrl Pts',(6.75984283251556,0.355909582581761,144.713642158459));
#44402=CARTESIAN_POINT('Ctrl Pts',(6.74635595661114,0.528176397330839,144.721781499313));
#44403=CARTESIAN_POINT('Ctrl Pts',(6.7326840032492,0.702807192019788,144.730032534568));
#44404=CARTESIAN_POINT('Ctrl Pts',(6.71224271718065,0.876706369439806,144.738283569823));
#44405=CARTESIAN_POINT('Ctrl Pts',(6.68514992355707,1.04931382320304,144.746534605078));
#44406=CARTESIAN_POINT('Ctrl Pts',(6.65805712993348,1.22192127696627,144.754785640333));
#44407=CARTESIAN_POINT('Ctrl Pts',(6.62431296874273,1.39323664339194,144.763036675588));
#44408=CARTESIAN_POINT('Ctrl Pts',(6.58408725713041,1.56271686190845,144.771287710843));
#44409=CARTESIAN_POINT('Ctrl Pts',(6.54395130916204,1.73181888545011,144.779520333919));
#44410=CARTESIAN_POINT('Ctrl Pts',(6.49723756827165,1.8996219445071,144.787752956995));
#44411=CARTESIAN_POINT('Ctrl Pts',(6.44404249761946,2.0655762607259,144.795985580071));
#44412=CARTESIAN_POINT('Ctrl Pts',(6.39091198629422,2.23132916920469,144.804208211759));
#44413=CARTESIAN_POINT('Ctrl Pts',(6.33131591745078,2.39523746481411,144.812430843447));
#44414=CARTESIAN_POINT('Ctrl Pts',(6.26540171352483,2.55676169561424,144.820653475135));
#44415=CARTESIAN_POINT('Ctrl Pts',(6.19955429764811,2.71812226080607,144.828867775181));
#44416=CARTESIAN_POINT('Ctrl Pts',(6.12740163149053,2.87710324275143,144.837082075227));
#44417=CARTESIAN_POINT('Ctrl Pts',(6.04914089969554,3.03318040604753,144.845296375274));
#44418=CARTESIAN_POINT('Ctrl Pts',(5.96963345730859,3.19174391272658,144.853641530918));
#44419=CARTESIAN_POINT('Ctrl Pts',(5.88382178386252,3.34730993633217,144.861986686562));
#44420=CARTESIAN_POINT('Ctrl Pts',(5.79196410820693,3.49934862070682,144.870331842207));
#44421=CARTESIAN_POINT('Ctrl Pts',(5.70168008987063,3.64878265841722,144.87853403304));
#44422=CARTESIAN_POINT('Ctrl Pts',(5.60555574342687,3.79480891683922,144.886736223873));
#44423=CARTESIAN_POINT('Ctrl Pts',(5.50388301182707,3.9369481571544,144.894938414706));
#44424=CARTESIAN_POINT('Ctrl Pts',(5.40224546313339,4.0790382115033,144.903137767247));
#44425=CARTESIAN_POINT('Ctrl Pts',(5.29506356124918,4.2172436355249,144.911337119788));
#44426=CARTESIAN_POINT('Ctrl Pts',(5.18267264513429,4.35111402440534,144.919536472329));
#44427=CARTESIAN_POINT('Ctrl Pts',(5.07030023271001,4.48496237328161,144.927734474954));
#44428=CARTESIAN_POINT('Ctrl Pts',(4.95272074510374,4.61447683477543,144.93593247758));
#44429=CARTESIAN_POINT('Ctrl Pts',(4.83030992278301,4.73923992322229,144.944130480205));
#44430=CARTESIAN_POINT('Ctrl Pts',(4.7040745734996,4.86790103135945,144.952584616083));
#44431=CARTESIAN_POINT('Ctrl Pts',(4.57270135312063,4.99150874150268,144.96103875196));
#44432=CARTESIAN_POINT('Ctrl Pts',(4.43664349550639,5.10964612216745,144.969492887838));
#44433=CARTESIAN_POINT('Ctrl Pts',(4.30464012473797,5.22426304128517,144.977695092785));
#44434=CARTESIAN_POINT('Ctrl Pts',(4.16822762356709,5.33373077776102,144.985897297732));
#44435=CARTESIAN_POINT('Ctrl Pts',(4.02785338214885,5.43770964027246,144.994099502679));
#44436=CARTESIAN_POINT('Ctrl Pts',(3.88101174320888,5.54647907284095,145.002679604023));
#44437=CARTESIAN_POINT('Ctrl Pts',(3.72983501078796,5.64924161019091,145.011259705366));
#44438=CARTESIAN_POINT('Ctrl Pts',(3.57486866209415,5.7456594964179,145.019839806709));
#44439=CARTESIAN_POINT('Ctrl Pts',(3.41990231340035,5.84207738264489,145.028419908052));
#44440=CARTESIAN_POINT('Ctrl Pts',(3.26114675272484,5.93215042579056,145.037000009395));
#44441=CARTESIAN_POINT('Ctrl Pts',(3.09917575053269,6.01559628526634,145.045580110739));
#44442=CARTESIAN_POINT('Ctrl Pts',(3.09917575053276,6.0155962852663,143.045751582743));
#44443=CARTESIAN_POINT('Ctrl Pts',(2.93382384459276,6.10078395293754,143.054501030655));
#44444=CARTESIAN_POINT('Ctrl Pts',(2.76495772122989,6.17915010267047,143.063250478567));
#44445=CARTESIAN_POINT('Ctrl Pts',(2.5931509331671,6.25042856433178,143.07199992648));
#44446=CARTESIAN_POINT('Ctrl Pts',(2.4213455324562,6.3217064504145,143.08074930374));
#44447=CARTESIAN_POINT('Ctrl Pts',(2.24659977927598,6.38589665313455,143.089498681));
#44448=CARTESIAN_POINT('Ctrl Pts',(2.06950718689931,6.44278115439071,143.09824805826));
#44449=CARTESIAN_POINT('Ctrl Pts',(1.89241596572878,6.49966521519719,143.106997367774));
#44450=CARTESIAN_POINT('Ctrl Pts',(1.71297821457219,6.5492436000954,143.115746677289));
#44451=CARTESIAN_POINT('Ctrl Pts',(1.5318033733587,6.5913479217355,143.124495986804));
#44452=CARTESIAN_POINT('Ctrl Pts',(1.35062987477807,6.633451931353,143.13324523148));
#44453=CARTESIAN_POINT('Ctrl Pts',(1.16771959102976,6.66808192368234,143.141994476156));
#44454=CARTESIAN_POINT('Ctrl Pts',(0.983693746907072,6.69512028363165,143.150743720832));
#44455=CARTESIAN_POINT('Ctrl Pts',(0.799669205420081,6.72215845218865,143.159492903576));
#44456=CARTESIAN_POINT('Ctrl Pts',(0.614529402873668,6.74160505424577,143.16824208632));
#44457=CARTESIAN_POINT('Ctrl Pts',(0.428903127363422,6.75339404354121,143.176991269065));
#44458=CARTESIAN_POINT('Ctrl Pts',(0.243278104164058,6.7651829533033,143.185740392783));
#44459=CARTESIAN_POINT('Ctrl Pts',(0.0571669005392994,6.76931433552276,
143.194489516502));
#44460=CARTESIAN_POINT('Ctrl Pts',(-0.128798404777326,6.76577415902473,
143.20323864022));
#44461=CARTESIAN_POINT('Ctrl Pts',(-0.314762517258893,6.76223400523442,
143.21198770782));
#44462=CARTESIAN_POINT('Ctrl Pts',(-0.500580446819286,6.7510223966509,143.220736775419));
#44463=CARTESIAN_POINT('Ctrl Pts',(-0.685621118842369,6.732177410125,143.229485843018));
#44464=CARTESIAN_POINT('Ctrl Pts',(-0.870660665414345,6.71333253821774,
143.238234857404));
#44465=CARTESIAN_POINT('Ctrl Pts',(-1.05492267885482,6.68685441030613,143.24698387179));
#44466=CARTESIAN_POINT('Ctrl Pts',(-1.23778137635257,6.65283295028176,143.255732886175));
#44467=CARTESIAN_POINT('Ctrl Pts',(-1.42999922978838,6.61707018861867,143.264929696543));
#44468=CARTESIAN_POINT('Ctrl Pts',(-1.62066601233674,6.57297172934418,143.27412650691));
#44469=CARTESIAN_POINT('Ctrl Pts',(-1.80906628500351,6.52070304311304,143.283323317278));
#44470=CARTESIAN_POINT('Ctrl Pts',(-1.98831342545495,6.47097374915041,143.292073315015));
#44471=CARTESIAN_POINT('Ctrl Pts',(-2.16550875896671,6.41384933989539,143.300823312753));
#44472=CARTESIAN_POINT('Ctrl Pts',(-2.34005036713982,6.34952386240487,143.309573310491));
#44473=CARTESIAN_POINT('Ctrl Pts',(-2.5145884354706,6.28519968948607,143.318323130772));
#44474=CARTESIAN_POINT('Ctrl Pts',(-2.68647261718028,6.21367483971111,143.327072951053));
#44475=CARTESIAN_POINT('Ctrl Pts',(-2.85511905908704,6.13519226743856,143.335822771333));
#44476=CARTESIAN_POINT('Ctrl Pts',(-3.02376230488864,6.05671118252947,143.344572425792));
#44477=CARTESIAN_POINT('Ctrl Pts',(-3.18916767379891,5.97127275992641,143.353322080251));
#44478=CARTESIAN_POINT('Ctrl Pts',(-3.3507733410278,5.87916720438001,143.362071734709));
#44479=CARTESIAN_POINT('Ctrl Pts',(-3.51237616037359,5.78706327195648,143.370821234978));
#44480=CARTESIAN_POINT('Ctrl Pts',(-3.67017916302289,5.68829258362305,143.379570735246));
#44481=CARTESIAN_POINT('Ctrl Pts',(-3.82364636566451,5.5831906174105,143.388320235514));
#44482=CARTESIAN_POINT('Ctrl Pts',(-3.97711106778804,5.47809036367698,143.397069593223));
#44483=CARTESIAN_POINT('Ctrl Pts',(-4.1262398748195,5.36665920043208,143.405818950931));
#44484=CARTESIAN_POINT('Ctrl Pts',(-4.27052628213968,5.24927559512303,143.41456830864));
#44485=CARTESIAN_POINT('Ctrl Pts',(-4.41481053025033,5.1318937464299,143.423317535416));
#44486=CARTESIAN_POINT('Ctrl Pts',(-4.554252301366,5.00855981477291,143.432066762193));
#44487=CARTESIAN_POINT('Ctrl Pts',(-4.68837800630631,4.87969268191997,143.440815988969));
#44488=CARTESIAN_POINT('Ctrl Pts',(-4.82250188228982,4.75082730631721,143.44956509644));
#44489=CARTESIAN_POINT('Ctrl Pts',(-4.95130963053058,4.61642907903428,143.458314203911));
#44490=CARTESIAN_POINT('Ctrl Pts',(-5.07436379033462,4.47695444731582,143.467063311382));
#44491=CARTESIAN_POINT('Ctrl Pts',(-5.19741643562905,4.33748153220467,143.475812311172));
#44492=CARTESIAN_POINT('Ctrl Pts',(-5.31471544462877,4.19293255254458,143.484561310961));
#44493=CARTESIAN_POINT('Ctrl Pts',(-5.42586245275734,4.0437984177946,143.493310310751));
#44494=CARTESIAN_POINT('Ctrl Pts',(-5.53702160019258,3.89464799484194,143.502060266093));
#44495=CARTESIAN_POINT('Ctrl Pts',(-5.64202723081354,3.74091164443695,143.510810221435));
#44496=CARTESIAN_POINT('Ctrl Pts',(-5.74052265233067,3.58311159163072,143.519560176778));
#44497=CARTESIAN_POINT('Ctrl Pts',(-5.83901427067021,3.42531763191609,143.52830979426));
#44498=CARTESIAN_POINT('Ctrl Pts',(-5.93099603115843,3.26346052695425,143.537059411742));
#44499=CARTESIAN_POINT('Ctrl Pts',(-6.01615550622858,3.09809004466874,143.545809029225));
#44500=CARTESIAN_POINT('Ctrl Pts',(-6.101312145789,2.93272506863618,143.554558355376));
#44501=CARTESIAN_POINT('Ctrl Pts',(-6.17964682328844,2.76384720416678,143.563307681527));
#44502=CARTESIAN_POINT('Ctrl Pts',(-6.25089348288656,2.5920300279137,143.572057007678));
#44503=CARTESIAN_POINT('Ctrl Pts',(-6.32213814889422,2.4202176593679,143.58080608901));
#44504=CARTESIAN_POINT('Ctrl Pts',(-6.38629508412675,2.24546640831663,143.589555170341));
#44505=CARTESIAN_POINT('Ctrl Pts',(-6.44314639819898,2.06836976659772,143.598304251673));
#44506=CARTESIAN_POINT('Ctrl Pts',(-6.50000285283783,1.89125711157993,143.607054124107));
#44507=CARTESIAN_POINT('Ctrl Pts',(-6.54955227673327,1.71179891439961,143.615803996542));
#44508=CARTESIAN_POINT('Ctrl Pts',(-6.59162635926456,1.53060476278125,143.624553868976));
#44509=CARTESIAN_POINT('Ctrl Pts',(-6.63369752055257,1.34942319164398,143.633303133899));
#44510=CARTESIAN_POINT('Ctrl Pts',(-6.66829431424304,1.16650618642415,143.642052398821));
#44511=CARTESIAN_POINT('Ctrl Pts',(-6.69529923745459,0.98247499761575,143.650801663744));
#44512=CARTESIAN_POINT('Ctrl Pts',(-6.72230554731477,0.798434359174936,
143.659551377923));
#44513=CARTESIAN_POINT('Ctrl Pts',(-6.74171916496728,0.613279706237536,
143.668301092103));
#44514=CARTESIAN_POINT('Ctrl Pts',(-6.75347414817293,0.427639953652585,
143.677050806283));
#44515=CARTESIAN_POINT('Ctrl Pts',(-6.76248837758735,0.2852833641991,143.683760465459));
#44516=CARTESIAN_POINT('Ctrl Pts',(-6.76699999999982,0.142641701108978,
143.690470124634));
#44517=CARTESIAN_POINT('Ctrl Pts',(-6.767,8.75965874919443E-12,143.69717978381));
#44518=CARTESIAN_POINT('',(-6.76699974675837,-0.00185131634684238,143.302820216147));
#44519=CARTESIAN_POINT('Ctrl Pts',(3.09917575053256,6.0155962852664,142.651137628792));
#44520=CARTESIAN_POINT('Ctrl Pts',(2.94537248680428,6.09483420661211,142.659292690381));
#44521=CARTESIAN_POINT('Ctrl Pts',(2.7887129155403,6.16807472739275,142.66744775197));
#44522=CARTESIAN_POINT('Ctrl Pts',(2.62971668029715,6.23513265146516,142.675602813559));
#44523=CARTESIAN_POINT('Ctrl Pts',(2.51269282237715,6.28448839229172,142.681605073721));
#44524=CARTESIAN_POINT('Ctrl Pts',(2.39440352898993,6.33049591829624,142.687607333883));
#44525=CARTESIAN_POINT('Ctrl Pts',(2.27506026073269,6.37309891732703,142.693609594045));
#44526=CARTESIAN_POINT('Ctrl Pts',(2.1113620730569,6.43153567570255,142.701842644177));
#44527=CARTESIAN_POINT('Ctrl Pts',(1.94517163699043,6.48374673505441,142.710075694309));
#44528=CARTESIAN_POINT('Ctrl Pts',(1.77700268200559,6.5295138002875,142.718308744441));
#44529=CARTESIAN_POINT('Ctrl Pts',(1.6090339903958,6.57522636398105,142.726531990276));
#44530=CARTESIAN_POINT('Ctrl Pts',(1.43909181369065,6.61451012086672,142.734755236111));
#44531=CARTESIAN_POINT('Ctrl Pts',(1.26770897287109,6.64719511975556,142.742978481946));
#44532=CARTESIAN_POINT('Ctrl Pts',(1.09649592002553,6.67984773780793,142.751193581059));
#44533=CARTESIAN_POINT('Ctrl Pts',(0.923845394888543,6.7059145504386,142.759408680172));
#44534=CARTESIAN_POINT('Ctrl Pts',(0.750304561895766,6.72527561252313,142.767623779286));
#44535=CARTESIAN_POINT('Ctrl Pts',(0.576900932762358,6.74462136747566,142.775832383425));
#44536=CARTESIAN_POINT('Ctrl Pts',(0.402608752152995,6.75727189219634,142.784040987564));
#44537=CARTESIAN_POINT('Ctrl Pts',(0.227984638693499,6.76315843408387,142.792249591703));
#44538=CARTESIAN_POINT('Ctrl Pts',(0.0534636558596394,6.76904149945985,
142.800453347952));
#44539=CARTESIAN_POINT('Ctrl Pts',(-0.121388512277072,6.76816852798543,
142.808657104201));
#44540=CARTESIAN_POINT('Ctrl Pts',(-0.2960107754922,6.76052265884765,142.81686086045));
#44541=CARTESIAN_POINT('Ctrl Pts',(-0.470581372381167,6.75287905192983,
142.825062189414));
#44542=CARTESIAN_POINT('Ctrl Pts',(-0.644921842294491,6.73846655089551,
142.833263518378));
#44543=CARTESIAN_POINT('Ctrl Pts',(-0.818471491392515,6.71732040457932,
142.841464847342));
#44544=CARTESIAN_POINT('Ctrl Pts',(-0.991997206337053,6.6961771745186,142.849665045265));
#44545=CARTESIAN_POINT('Ctrl Pts',(-1.16473196205274,6.66830219121516,142.857865243188));
#44546=CARTESIAN_POINT('Ctrl Pts',(-1.33612055799236,6.63378254501233,142.866065441111));
#44547=CARTESIAN_POINT('Ctrl Pts',(-1.5075165769091,6.59926140373601,142.87426599419));
#44548=CARTESIAN_POINT('Ctrl Pts',(-1.67756596863274,6.55809509690823,142.88246654727));
#44549=CARTESIAN_POINT('Ctrl Pts',(-1.84572403230184,6.51042178330893,142.89066710035));
#44550=CARTESIAN_POINT('Ctrl Pts',(-2.01391985256634,6.462737765602,142.898869494703));
#44551=CARTESIAN_POINT('Ctrl Pts',(-2.18022315434341,6.40854392888582,142.907071889057));
#44552=CARTESIAN_POINT('Ctrl Pts',(-2.34410464082515,6.34802823188918,142.91527428341));
#44553=CARTESIAN_POINT('Ctrl Pts',(-2.50813938530545,6.28745594207779,142.923484348444));
#44554=CARTESIAN_POINT('Ctrl Pts',(-2.66974745302628,6.22055010447293,142.931694413477));
#44555=CARTESIAN_POINT('Ctrl Pts',(-2.82841890151393,6.147547113895,142.939904478511));
#44556=CARTESIAN_POINT('Ctrl Pts',(-2.98716628734198,6.07450918538086,142.948118472737));
#44557=CARTESIAN_POINT('Ctrl Pts',(-3.14297393250963,5.99536844806555,142.956332466962));
#44558=CARTESIAN_POINT('Ctrl Pts',(-3.29535681582956,5.91040713118527,142.964546461187));
#44559=CARTESIAN_POINT('Ctrl Pts',(-3.44794744777205,5.82532998373289,142.972771653822));
#44560=CARTESIAN_POINT('Ctrl Pts',(-3.59710368060713,5.7344165842604,142.980996846458));
#44561=CARTESIAN_POINT('Ctrl Pts',(-3.74236875980682,5.63799299978476,142.989222039093));
#44562=CARTESIAN_POINT('Ctrl Pts',(-3.87300533439763,5.55127947678899,142.996618937213));
#44563=CARTESIAN_POINT('Ctrl Pts',(-4.00049525190842,5.46011034373183,143.004015835333));
#44564=CARTESIAN_POINT('Ctrl Pts',(-4.12452997356337,5.36474990071087,143.011412733452));
#44565=CARTESIAN_POINT('Ctrl Pts',(-4.26950967042598,5.25328653031429,143.020058699943));
#44566=CARTESIAN_POINT('Ctrl Pts',(-4.41009750244017,5.1358434511334,143.028704666434));
#44567=CARTESIAN_POINT('Ctrl Pts',(-4.54579968236004,5.01278308406172,143.037350632925));
#44568=CARTESIAN_POINT('Ctrl Pts',(-4.68132828074351,4.8898801279292,143.04598554005));
#44569=CARTESIAN_POINT('Ctrl Pts',(-4.81198346391476,4.76137441564103,143.054620447174));
#44570=CARTESIAN_POINT('Ctrl Pts',(-4.93730352515229,4.62766927302706,143.063255354298));
#44571=CARTESIAN_POINT('Ctrl Pts',(-5.06678411127458,4.4895252275944,143.07217693337));
#44572=CARTESIAN_POINT('Ctrl Pts',(-5.19056897234715,4.34583075751169,143.081098512442));
#44573=CARTESIAN_POINT('Ctrl Pts',(-5.30818699501875,4.19707515133024,143.090020091513));
#44574=CARTESIAN_POINT('Ctrl Pts',(-5.421711262608,4.05349705965723,143.098631150489));
#44575=CARTESIAN_POINT('Ctrl Pts',(-5.52949049087475,3.90520445058976,143.107242209465));
#44576=CARTESIAN_POINT('Ctrl Pts',(-5.63113892221326,3.75267417167211,143.11585326844));
#44577=CARTESIAN_POINT('Ctrl Pts',(-5.73269149438886,3.60028773584836,143.12445620679));
#44578=CARTESIAN_POINT('Ctrl Pts',(-5.82812462812182,3.44367185071973,143.133059145139));
#44579=CARTESIAN_POINT('Ctrl Pts',(-5.91709398212594,3.28333486057834,143.141662083489));
#44580=CARTESIAN_POINT('Ctrl Pts',(-6.00596371103467,3.1231774107755,143.150255388538));
#44581=CARTESIAN_POINT('Ctrl Pts',(-6.08838395204931,2.95930743465205,143.158848693587));
#44582=CARTESIAN_POINT('Ctrl Pts',(-6.16405458437788,2.79226074728168,143.167441998635));
#44583=CARTESIAN_POINT('Ctrl Pts',(-6.17248553142073,2.77364901203428,143.168399433476));
#44584=CARTESIAN_POINT('Ctrl Pts',(-6.18083273707581,2.7549978698738,143.169356868316));
#44585=CARTESIAN_POINT('Ctrl Pts',(-6.18909582082967,2.73630808217728,143.170314303157));
#44586=CARTESIAN_POINT('Ctrl Pts',(-6.26062697767703,2.57451592624766,143.178602543211));
#44587=CARTESIAN_POINT('Ctrl Pts',(-6.32578739031436,2.40996812569131,143.186890783266));
#44588=CARTESIAN_POINT('Ctrl Pts',(-6.3843812733518,2.24320412724186,143.19517902332));
#44589=CARTESIAN_POINT('Ctrl Pts',(-6.44300346685093,2.07635955441253,143.203471267955));
#44590=CARTESIAN_POINT('Ctrl Pts',(-6.49505269240845,1.9072969767779,143.21176351259));
#44591=CARTESIAN_POINT('Ctrl Pts',(-6.54038305502368,1.73657090081549,143.220055757224));
#44592=CARTESIAN_POINT('Ctrl Pts',(-6.58576627920047,1.56564573429979,143.228357671779));
#44593=CARTESIAN_POINT('Ctrl Pts',(-6.62441490038546,1.39305353014417,143.236659586334));
#44594=CARTESIAN_POINT('Ctrl Pts',(-6.65623394311995,1.21935995278584,143.24496150089));
#44595=CARTESIAN_POINT('Ctrl Pts',(-6.68807450098562,1.0455489287735,143.253269028963));
#44596=CARTESIAN_POINT('Ctrl Pts',(-6.71307622229203,0.870635389273911,
143.261576557037));
#44597=CARTESIAN_POINT('Ctrl Pts',(-6.73119600157738,0.695190181424242,
143.26988408511));
#44598=CARTESIAN_POINT('Ctrl Pts',(-6.74934006901336,0.519509802959734,
143.278202748777));
#44599=CARTESIAN_POINT('Ctrl Pts',(-6.76058374549735,0.343296678059089,
143.286521412444));
#44600=CARTESIAN_POINT('Ctrl Pts',(-6.76493599236578,0.167122766833334,
143.294840076111));
#44601=CARTESIAN_POINT('Ctrl Pts',(-6.76632770385839,0.11078789788809,143.29750012279));
#44602=CARTESIAN_POINT('Ctrl Pts',(-6.76701515159437,0.0544570080009674,
143.300160169469));
#44603=CARTESIAN_POINT('Ctrl Pts',(-6.76699974675837,-0.00185131634684155,
143.302820216148));
#44604=CARTESIAN_POINT('Ctrl Pts',(-6.76699974675812,-0.00185131724654051,
143.30282021619));
#44605=CARTESIAN_POINT('Ctrl Pts',(-6.76694879264479,-0.18810057983288,
143.311618768413));
#44606=CARTESIAN_POINT('Ctrl Pts',(-6.7592084520437,-0.374197992708356,
143.320417320637));
#44607=CARTESIAN_POINT('Ctrl Pts',(-6.74381692552782,-0.559662643888693,
143.32921587286));
#44608=CARTESIAN_POINT('Ctrl Pts',(-6.72942699192261,-0.733058311553397,
143.337441865402));
#44609=CARTESIAN_POINT('Ctrl Pts',(-6.70832640600916,-0.906126217035766,
143.345667857943));
#44610=CARTESIAN_POINT('Ctrl Pts',(-6.68053450457218,-1.07830781005268,
143.353893850484));
#44611=CARTESIAN_POINT('Ctrl Pts',(-6.6527717393516,-1.25030889292472,143.362111219136));
#44612=CARTESIAN_POINT('Ctrl Pts',(-6.61833168465202,-1.42142516287446,
143.370328587787));
#44613=CARTESIAN_POINT('Ctrl Pts',(-6.57728557869943,-1.59110132179961,
143.378545956439));
#44614=CARTESIAN_POINT('Ctrl Pts',(-6.53627429113555,-1.76063354866794,
143.386756354501));
#44615=CARTESIAN_POINT('Ctrl Pts',(-6.48866819670722,-1.9287277512246,143.394966752564));
#44616=CARTESIAN_POINT('Ctrl Pts',(-6.43458991820602,-2.09483688733072,
143.403177150626));
#44617=CARTESIAN_POINT('Ctrl Pts',(-6.3805466951786,-2.26083834555534,143.411382226415));
#44618=CARTESIAN_POINT('Ctrl Pts',(-6.32003975573042,-2.42485696105429,
143.419587302204));
#44619=CARTESIAN_POINT('Ctrl Pts',(-6.25324209995986,-2.58635887673957,
143.427792377993));
#44620=CARTESIAN_POINT('Ctrl Pts',(-6.18647438537625,-2.74778840127588,
143.435993775962));
#44621=CARTESIAN_POINT('Ctrl Pts',(-6.11342170885582,-2.90670314306622,
143.444195173932));
#44622=CARTESIAN_POINT('Ctrl Pts',(-6.03430596010193,-3.06258723628868,
143.452396571901));
#44623=CARTESIAN_POINT('Ctrl Pts',(-5.95519640835219,-3.21845911937109,
143.460597327469));
#44624=CARTESIAN_POINT('Ctrl Pts',(-5.87002488458139,-3.37130050354307,
143.468798083037));
#44625=CARTESIAN_POINT('Ctrl Pts',(-5.77906035557741,-3.52061790124881,
143.476998838604));
#44626=CARTESIAN_POINT('Ctrl Pts',(-5.68809628862993,-3.66993454049323,
143.485199552516));
#44627=CARTESIAN_POINT('Ctrl Pts',(-5.59133946059942,-3.81572692231828,
143.493400266428));
#44628=CARTESIAN_POINT('Ctrl Pts',(-5.48910344561935,-3.95752856758985,
143.50160098034));
#44629=CARTESIAN_POINT('Ctrl Pts',(-5.386849422238,-4.09935519056552,143.50980313877));
#44630=CARTESIAN_POINT('Ctrl Pts',(-5.27911449863336,-4.23718938577961,
143.518005297199));
#44631=CARTESIAN_POINT('Ctrl Pts',(-5.16625402251077,-4.37059588327396,
143.526207455629));
#44632=CARTESIAN_POINT('Ctrl Pts',(-5.05335321319236,-4.50405005654085,
143.534412545282));
#44633=CARTESIAN_POINT('Ctrl Pts',(-4.93532343375856,-4.63307310655719,
143.542617634935));
#44634=CARTESIAN_POINT('Ctrl Pts',(-4.81255856699862,-4.75726486956614,
143.550822724588));
#44635=CARTESIAN_POINT('Ctrl Pts',(-4.68965345589309,-4.88159850698095,
143.559037187586));
#44636=CARTESIAN_POINT('Ctrl Pts',(-4.56200270287097,-5.00108957592308,
143.567251650584));
#44637=CARTESIAN_POINT('Ctrl Pts',(-4.43003590176463,-5.11537593037662,
143.575466113581));
#44638=CARTESIAN_POINT('Ctrl Pts',(-4.29799091449966,-5.22972999588296,
143.583685443389));
#44639=CARTESIAN_POINT('Ctrl Pts',(-4.16162506114506,-5.33887297648314,
143.591904773196));
#44640=CARTESIAN_POINT('Ctrl Pts',(-4.02139880848787,-5.44248478391004,
143.600124103004));
#44641=CARTESIAN_POINT('Ctrl Pts',(-3.88095528375388,-5.54625713155074,
143.608356168165));
#44642=CARTESIAN_POINT('Ctrl Pts',(-3.73663970249292,-5.64448097788017,
143.616588233325));
#44643=CARTESIAN_POINT('Ctrl Pts',(-3.58894026976262,-5.73688040140948,
143.624820298486));
#44644=CARTESIAN_POINT('Ctrl Pts',(-3.45617741423368,-5.81993563791387,
143.632219869747));
#44645=CARTESIAN_POINT('Ctrl Pts',(-3.3206810083165,-5.8982854429643,143.639619441007));
#44646=CARTESIAN_POINT('Ctrl Pts',(-3.18281997537517,-5.97176238679611,
143.647019012268));
#44647=CARTESIAN_POINT('Ctrl Pts',(-3.03087604775185,-6.05274520839092,
143.655174470675));
#44648=CARTESIAN_POINT('Ctrl Pts',(-2.87559151159903,-6.12805730365544,
143.663329929082));
#44649=CARTESIAN_POINT('Ctrl Pts',(-2.71743183989417,-6.19740697352767,
143.671485387488));
#44650=CARTESIAN_POINT('Ctrl Pts',(-2.55946466929967,-6.26667223573574,
143.67963091963));
#44651=CARTESIAN_POINT('Ctrl Pts',(-2.39862965996404,-6.32998937288949,
143.687776451772));
#44652=CARTESIAN_POINT('Ctrl Pts',(-2.23541880552875,-6.3871113786976,143.695921983914));
#44653=CARTESIAN_POINT('Ctrl Pts',(-2.0723722801886,-6.44417587112796,143.704059314714));
#44654=CARTESIAN_POINT('Ctrl Pts',(-1.90695501444588,-6.49505753028614,
143.712196645515));
#44655=CARTESIAN_POINT('Ctrl Pts',(-1.73968101121387,-6.53955648184354,
143.720333976315));
#44656=CARTESIAN_POINT('Ctrl Pts',(-1.57254027491464,-6.58401998115689,
143.728464824117));
#44657=CARTESIAN_POINT('Ctrl Pts',(-1.40354609809013,-6.62211080439482,
143.736595671919));
#44658=CARTESIAN_POINT('Ctrl Pts',(-1.23322975786386,-6.65367818310437,
143.744726519721));
#44659=CARTESIAN_POINT('Ctrl Pts',(-1.0630133305006,-6.68522704340764,143.752852597715));
#44660=CARTESIAN_POINT('Ctrl Pts',(-0.891476642852279,-6.71026001384686,
143.760978675709));
#44661=CARTESIAN_POINT('Ctrl Pts',(-0.719163335925261,-6.72867692018727,
143.769104753703));
#44662=CARTESIAN_POINT('Ctrl Pts',(-0.546239037482381,-6.74715912951398,
143.777259645285));
#44663=CARTESIAN_POINT('Ctrl Pts',(-0.37253296306589,-6.7589781802694,143.785414536867));
#44664=CARTESIAN_POINT('Ctrl Pts',(-0.198602602775026,-6.76408500879247,
143.793569428449));
#44665=CARTESIAN_POINT('Ctrl Pts',(-0.0253505100775911,-6.76917192246981,
143.801692518806));
#44666=CARTESIAN_POINT('Ctrl Pts',(0.148123753687154,-6.76759887689182,
143.809815609162));
#44667=CARTESIAN_POINT('Ctrl Pts',(0.321266709299463,-6.75936954911447,
143.817938699518));
#44668=CARTESIAN_POINT('Ctrl Pts',(0.49442326088739,-6.75113957513271,143.826062427737));
#44669=CARTESIAN_POINT('Ctrl Pts',(0.667248087080589,-6.73625229515411,
143.834186155955));
#44670=CARTESIAN_POINT('Ctrl Pts',(0.839190586537864,-6.71476344776689,
143.842309884173));
#44671=CARTESIAN_POINT('Ctrl Pts',(1.01117929956173,-6.69326882474954,143.850435795834));
#44672=CARTESIAN_POINT('Ctrl Pts',(1.18228485079778,-6.66516914665729,143.858561707494));
#44673=CARTESIAN_POINT('Ctrl Pts',(1.35196465532392,-6.63057166244019,143.866687619154));
#44674=CARTESIAN_POINT('Ctrl Pts',(1.52272957984003,-6.59575292371475,143.874865496864));
#44675=CARTESIAN_POINT('Ctrl Pts',(1.69205009072681,-6.55435305714574,143.883043374575));
#44676=CARTESIAN_POINT('Ctrl Pts',(1.85938724408571,-6.50653272308158,143.891221252285));
#44677=CARTESIAN_POINT('Ctrl Pts',(2.025925733503,-6.45894062510083,143.899360098758));
#44678=CARTESIAN_POINT('Ctrl Pts',(2.19049942769433,-6.40498938475211,143.907498945232));
#44679=CARTESIAN_POINT('Ctrl Pts',(2.35259619403884,-6.34488614143658,143.915637791705));
#44680=CARTESIAN_POINT('Ctrl Pts',(2.5158590047264,-6.28435054497517,143.923835185033));
#44681=CARTESIAN_POINT('Ctrl Pts',(2.67660876875601,-6.21757424780426,143.932032578362));
#44682=CARTESIAN_POINT('Ctrl Pts',(2.83434685429409,-6.14481626328674,143.94022997169));
#44683=CARTESIAN_POINT('Ctrl Pts',(2.99208493983216,-6.07205827876922,143.948427365019));
#44684=CARTESIAN_POINT('Ctrl Pts',(3.14681104284906,-5.99331883019363,143.956624758347));
#44685=CARTESIAN_POINT('Ctrl Pts',(3.29805599559148,-5.90890139111689,143.964822151676));
#44686=CARTESIAN_POINT('Ctrl Pts',(3.44983261439606,-5.82418720238604,143.973048361013));
#44687=CARTESIAN_POINT('Ctrl Pts',(3.59855533709777,-5.73350301216,143.98127457035));
#44688=CARTESIAN_POINT('Ctrl Pts',(3.7437228282438,-5.63709396633462,143.989500779687));
#44689=CARTESIAN_POINT('Ctrl Pts',(3.88872722993242,-5.54079323194213,143.99771774723));
#44690=CARTESIAN_POINT('Ctrl Pts',(4.03018405746355,-5.43878064568041,144.005934714773));
#44691=CARTESIAN_POINT('Ctrl Pts',(4.16761605287158,-5.33134743154553,144.014151682316));
#44692=CARTESIAN_POINT('Ctrl Pts',(4.30492123302262,-5.22401335131771,144.022361067659));
#44693=CARTESIAN_POINT('Ctrl Pts',(4.43820869666726,-5.11126882413304,144.030570453003));
#44694=CARTESIAN_POINT('Ctrl Pts',(4.5670296299557,-4.99344864388397,144.038779838346));
#44695=CARTESIAN_POINT('Ctrl Pts',(4.69575754093226,-4.87571354224188,144.046983295646));
#44696=CARTESIAN_POINT('Ctrl Pts',(4.8200250822395,-4.75291032896131,144.055186752947));
#44697=CARTESIAN_POINT('Ctrl Pts',(4.93941598264742,-4.62541444093038,144.063390210247));
#44698=CARTESIAN_POINT('Ctrl Pts',(5.05874461974385,-4.49798504302693,144.071589389379));
#44699=CARTESIAN_POINT('Ctrl Pts',(5.17320143790893,-4.36586810692125,144.079788568511));
#44700=CARTESIAN_POINT('Ctrl Pts',(5.28240649878178,-4.22947639568162,144.087987747643));
#44701=CARTESIAN_POINT('Ctrl Pts',(5.39159098306766,-4.09311038357981,144.096185381872));
#44702=CARTESIAN_POINT('Ctrl Pts',(5.49552545235458,-3.95247147651687,144.104383016102));
#44703=CARTESIAN_POINT('Ctrl Pts',(5.59386961355452,-3.80800626923742,144.112580650332));
#44704=CARTESIAN_POINT('Ctrl Pts',(5.69220667616514,-3.66355148961492,144.120777692847));
#44705=CARTESIAN_POINT('Ctrl Pts',(5.78495403173994,-3.51527125581709,144.128974735363));
#44706=CARTESIAN_POINT('Ctrl Pts',(5.87181421219092,-3.36364190387632,144.137171777878));
#44707=CARTESIAN_POINT('Ctrl Pts',(5.95868390967129,-3.21199593832746,144.145369718521));
#44708=CARTESIAN_POINT('Ctrl Pts',(6.03966496859387,-3.05700043485392,144.153567659164));
#44709=CARTESIAN_POINT('Ctrl Pts',(6.11450543412456,-2.89915716994805,144.161765599807));
#44710=CARTESIAN_POINT('Ctrl Pts',(6.18936770189748,-2.74126792273742,144.169965928643));
#44711=CARTESIAN_POINT('Ctrl Pts',(6.2580856594678,-2.5805295856471,144.178166257478));
#44712=CARTESIAN_POINT('Ctrl Pts',(6.32045511063464,-2.41746482796597,144.186366586314));
#44713=CARTESIAN_POINT('Ctrl Pts',(6.38288955238794,-2.25423015257616,144.194575460106));
#44714=CARTESIAN_POINT('Ctrl Pts',(6.43896214304632,-2.08866454888237,144.202784333897));
#44715=CARTESIAN_POINT('Ctrl Pts',(6.48851797523371,-1.9213077538669,144.210993207688));
#44716=CARTESIAN_POINT('Ctrl Pts',(6.53810040348953,-1.75386114030583,144.219206487092));
#44717=CARTESIAN_POINT('Ctrl Pts',(6.58115901258738,-1.58462176628159,144.227419766495));
#44718=CARTESIAN_POINT('Ctrl Pts',(6.61758987996973,-1.414140438755,144.235633045898));
#44719=CARTESIAN_POINT('Ctrl Pts',(6.65407403322155,-1.24340975549199,144.243858338514));
#44720=CARTESIAN_POINT('Ctrl Pts',(6.6839110103928,-1.07143384184307,144.252083631129));
#44721=CARTESIAN_POINT('Ctrl Pts',(6.70704853533991,-0.898770796474191,
144.260308923745));
#44722=CARTESIAN_POINT('Ctrl Pts',(6.72797364727505,-0.742617812969376,
144.267747712857));
#44723=CARTESIAN_POINT('Ctrl Pts',(6.74341991850449,-0.585903071393837,
144.27518650197));
#44724=CARTESIAN_POINT('Ctrl Pts',(6.75338540460217,-0.429039132138814,
144.282625291083));
#44725=CARTESIAN_POINT('Ctrl Pts',(6.76440575894322,-0.255570805859548,
144.290851492102));
#44726=CARTESIAN_POINT('Ctrl Pts',(6.76875362779252,-0.081435143226303,
144.299077693121));
#44727=CARTESIAN_POINT('Ctrl Pts',(6.76636347128686,0.0928136543552743,
144.307303894141));
#44728=CARTESIAN_POINT('Ctrl Pts',(6.76397599961829,0.266866720137652,144.315520854757));
#44729=CARTESIAN_POINT('Ctrl Pts',(6.75486557891059,0.44103231246453,144.323737815373));
#44730=CARTESIAN_POINT('Ctrl Pts',(6.73901844382689,0.614751505700547,144.331954775989));
#44731=CARTESIAN_POINT('Ctrl Pts',(6.7231859290136,0.788310428858095,144.34016415579));
#44732=CARTESIAN_POINT('Ctrl Pts',(6.70062910993685,0.961423418208949,144.348373535592));
#44733=CARTESIAN_POINT('Ctrl Pts',(6.67138625310781,1.13353185303462,144.356582915394));
#44734=CARTESIAN_POINT('Ctrl Pts',(6.64216450780107,1.30551603628391,144.364786368535));
#44735=CARTESIAN_POINT('Ctrl Pts',(6.60626639893625,1.47649675739657,144.372989821675));
#44736=CARTESIAN_POINT('Ctrl Pts',(6.56378198500671,1.64592073117187,144.381193274816));
#44737=CARTESIAN_POINT('Ctrl Pts',(6.52131971991186,1.81525637741148,144.389392451166));
#44738=CARTESIAN_POINT('Ctrl Pts',(6.47227807732916,1.98303654611663,144.397591627517));
#44739=CARTESIAN_POINT('Ctrl Pts',(6.41679817313314,2.14871827033588,144.405790803867));
#44740=CARTESIAN_POINT('Ctrl Pts',(6.36132870831835,2.31436881903838,144.413988437419));
#44741=CARTESIAN_POINT('Ctrl Pts',(6.2994235028427,2.47792136806083,144.42218607097));
#44742=CARTESIAN_POINT('Ctrl Pts',(6.23127358718948,2.63884794590266,144.430383704522));
#44743=CARTESIAN_POINT('Ctrl Pts',(6.16312858000278,2.79976293308131,144.438580747643));
#44744=CARTESIAN_POINT('Ctrl Pts',(6.08873989744063,2.9580519951231,144.446777790764));
#44745=CARTESIAN_POINT('Ctrl Pts',(6.0083467689822,3.11320704477893,144.454974833885));
#44746=CARTESIAN_POINT('Ctrl Pts',(5.92794481948514,3.26837911863463,144.463172776416));
#44747=CARTESIAN_POINT('Ctrl Pts',(5.84153727655828,3.42041617646988,144.471370718948));
#44748=CARTESIAN_POINT('Ctrl Pts',(5.74940940996816,3.56883460482125,144.479568661479));
#44749=CARTESIAN_POINT('Ctrl Pts',(5.65725469061115,3.71729629310694,144.487768993488));
#44750=CARTESIAN_POINT('Ctrl Pts',(5.55937651560925,3.86213694634304,144.495969325496));
#44751=CARTESIAN_POINT('Ctrl Pts',(5.45610358890816,4.00290177585006,144.504169657505));
#44752=CARTESIAN_POINT('Ctrl Pts',(5.35272302390506,4.14381332035504,144.512378536476));
#44753=CARTESIAN_POINT('Ctrl Pts',(5.243936686171,4.28064026447128,144.520587415447));
#44754=CARTESIAN_POINT('Ctrl Pts',(5.13011432771665,4.41296000260101,144.528796294418));
#44755=CARTESIAN_POINT('Ctrl Pts',(5.01623086678018,4.54535077303533,144.537009580106));
#44756=CARTESIAN_POINT('Ctrl Pts',(4.8973062397233,4.67322925158298,144.545222865793));
#44757=CARTESIAN_POINT('Ctrl Pts',(4.77374712394494,4.796209690644,144.553436151481));
#44758=CARTESIAN_POINT('Ctrl Pts',(4.65000725640862,4.91937003493026,144.561661452193));
#44759=CARTESIAN_POINT('Ctrl Pts',(4.52161961520314,5.03761777751236,144.569886752906));
#44760=CARTESIAN_POINT('Ctrl Pts',(4.38902498581782,5.15060663163737,144.578112053618));
#44761=CARTESIAN_POINT('Ctrl Pts',(4.26910913819172,5.25279142055012,144.585550845909));
#44762=CARTESIAN_POINT('Ctrl Pts',(4.14575295375266,5.35067537461854,144.5929896382));
#44763=CARTESIAN_POINT('Ctrl Pts',(4.01930215292755,5.44403335804181,144.600428430491));
#44764=CARTESIAN_POINT('Ctrl Pts',(3.87432988710954,5.55106564491353,144.608956795407));
#44765=CARTESIAN_POINT('Ctrl Pts',(3.72484198009896,5.65247813014822,144.617485160323));
#44766=CARTESIAN_POINT('Ctrl Pts',(3.57132008783943,5.74786585005205,144.626013525239));
#44767=CARTESIAN_POINT('Ctrl Pts',(3.4177981955799,5.84325356995589,144.634541890156));
#44768=CARTESIAN_POINT('Ctrl Pts',(3.2602426527421,5.93261620916592,144.643070255072));
#44769=CARTESIAN_POINT('Ctrl Pts',(3.0991757505327,6.01559628526633,144.651598619988));
#44770=CARTESIAN_POINT('Origin',(0.,0.,-3.69717978381041));
#44771=CARTESIAN_POINT('',(3.09917575053267,6.01559628526635,147.045751582742));
#44772=CARTESIAN_POINT('',(3.09917575053262,6.01559628526637,146.651454788324));
#44773=CARTESIAN_POINT('',(3.09917575053259,6.01559628526639,-3.69717978381041));
#44774=CARTESIAN_POINT('',(-6.767,8.90224858076955E-12,145.69717978381));
#44775=CARTESIAN_POINT('Ctrl Pts',(-6.767,8.90224859300312E-12,145.69717978381));
#44776=CARTESIAN_POINT('Ctrl Pts',(-6.76700000000025,-0.186007249406894,
145.705929295616));
#44777=CARTESIAN_POINT('Ctrl Pts',(-6.75932637295486,-0.372014355518876,
145.714678807422));
#44778=CARTESIAN_POINT('Ctrl Pts',(-6.74400518266998,-0.557389537146528,
145.723428319228));
#44779=CARTESIAN_POINT('Ctrl Pts',(-6.72868405709738,-0.742763935803023,
145.732177794078));
#44780=CARTESIAN_POINT('Ctrl Pts',(-6.70571545653105,-0.927506129686817,
145.740927268929));
#44781=CARTESIAN_POINT('Ctrl Pts',(-6.67517739415784,-1.1109886392417,145.74967674378));
#44782=CARTESIAN_POINT('Ctrl Pts',(-6.6446394582322,-1.29447038905887,145.758426182402));
#44783=CARTESIAN_POINT('Ctrl Pts',(-6.6065321702729,-1.47669218227628,145.767175621024));
#44784=CARTESIAN_POINT('Ctrl Pts',(-6.56098496116854,-1.65703510503559,
145.775925059646));
#44785=CARTESIAN_POINT('Ctrl Pts',(-6.51543793687668,-1.83737729603489,
145.784674462766));
#44786=CARTESIAN_POINT('Ctrl Pts',(-6.46245112202797,-2.01584035396551,
145.793423865886));
#44787=CARTESIAN_POINT('Ctrl Pts',(-6.40220448416404,-2.19181813637671,
145.802173269006));
#44788=CARTESIAN_POINT('Ctrl Pts',(-6.34195808575363,-2.3677952193547,145.810922637352));
#44789=CARTESIAN_POINT('Ctrl Pts',(-6.27445201489426,-2.54128677544354,
145.819672005697));
#44790=CARTESIAN_POINT('Ctrl Pts',(-6.1999155513639,-2.71170355237368,145.828421374042));
#44791=CARTESIAN_POINT('Ctrl Pts',(-6.12537937789263,-2.88211966612593,
145.837170708339));
#44792=CARTESIAN_POINT('Ctrl Pts',(-6.04381298133861,-3.0494607620996,145.845920042636));
#44793=CARTESIAN_POINT('Ctrl Pts',(-5.9554933942657,-3.21315848206365,145.854669376933));
#44794=CARTESIAN_POINT('Ctrl Pts',(-5.8671741435545,-3.37685557859132,145.863418677909));
#44795=CARTESIAN_POINT('Ctrl Pts',(-5.77210188986554,-3.53690907466794,
145.872167978884));
#44796=CARTESIAN_POINT('Ctrl Pts',(-5.67059953467412,-3.69277536784376,
145.88091727986));
#44797=CARTESIAN_POINT('Ctrl Pts',(-5.56909755762125,-3.84864108035272,
145.889666548241));
#44798=CARTESIAN_POINT('Ctrl Pts',(-5.46116568338445,-4.00031938103767,
145.898415816621));
#44799=CARTESIAN_POINT('Ctrl Pts',(-5.34717048686504,-4.14729511662716,
145.907165085002));
#44800=CARTESIAN_POINT('Ctrl Pts',(-5.23317570555923,-4.29427031687546,
145.915914321515));
#44801=CARTESIAN_POINT('Ctrl Pts',(-5.11311782179226,-4.43654275986644,
145.924663558027));
#44802=CARTESIAN_POINT('Ctrl Pts',(-4.9874045917245,-4.57362924147174,145.93341279454));
#44803=CARTESIAN_POINT('Ctrl Pts',(-4.86169180911277,-4.71071523513975,
145.942161999911));
#44804=CARTESIAN_POINT('Ctrl Pts',(-4.73032391415889,-4.84261509316077,
145.950911205282));
#44805=CARTESIAN_POINT('Ctrl Pts',(-4.5937470723776,-4.96888084331092,145.959660410653));
#44806=CARTESIAN_POINT('Ctrl Pts',(-4.45717070537871,-5.09514615452315,
145.96840958561));
#44807=CARTESIAN_POINT('Ctrl Pts',(-4.31538563819978,-5.21577720253245,
145.977158760566));
#44808=CARTESIAN_POINT('Ctrl Pts',(-4.16887341291117,-5.33036429028284,
145.985907935522));
#44809=CARTESIAN_POINT('Ctrl Pts',(-4.02236168477819,-5.44495098920821,
145.99465708079));
#44810=CARTESIAN_POINT('Ctrl Pts',(-3.87112305634932,-5.55349359238415,
146.003406226058));
#44811=CARTESIAN_POINT('Ctrl Pts',(-3.71567117317237,-5.65562346102142,
146.012155371326));
#44812=CARTESIAN_POINT('Ctrl Pts',(-3.56021980457809,-5.75775299158455,
146.020904487632));
#44813=CARTESIAN_POINT('Ctrl Pts',(-3.400555448629,-5.85346967275056,146.029653603938));
#44814=CARTESIAN_POINT('Ctrl Pts',(-3.23722036323917,-5.94244842803281,
146.038402720244));
#44815=CARTESIAN_POINT('Ctrl Pts',(-3.07388580496584,-6.03142689616201,
146.047151808315));
#44816=CARTESIAN_POINT('Ctrl Pts',(-2.90688079258268,-6.11366734484556,
146.055900896386));
#44817=CARTESIAN_POINT('Ctrl Pts',(-2.73677251095199,-6.18889046787044,
146.064649984457));
#44818=CARTESIAN_POINT('Ctrl Pts',(-2.56666476417235,-6.26411335438029,
146.073399045019));
#44819=CARTESIAN_POINT('Ctrl Pts',(-2.39345402972688,-6.33231884350066,
146.082148105582));
#44820=CARTESIAN_POINT('Ctrl Pts',(-2.21772856474637,-6.39327529620835,
146.090897166144));
#44821=CARTESIAN_POINT('Ctrl Pts',(-2.04200363768883,-6.45423156231887,
146.099646199924));
#44822=CARTESIAN_POINT('Ctrl Pts',(-1.86376426620721,-6.50793874251876,
146.108395233704));
#44823=CARTESIAN_POINT('Ctrl Pts',(-1.6836157819533,-6.55421443795958,146.117144267484));
#44824=CARTESIAN_POINT('Ctrl Pts',(-1.50346783420502,-6.60048999558536,
146.125893275208));
#44825=CARTESIAN_POINT('Ctrl Pts',(-1.32141106257872,-6.63933404145371,
146.134642282932));
#44826=CARTESIAN_POINT('Ctrl Pts',(-1.1380637595966,-6.67061465526925,146.143391290656));
#44827=CARTESIAN_POINT('Ctrl Pts',(-0.954716987425405,-6.70189517852391,
146.152140273051));
#44828=CARTESIAN_POINT('Ctrl Pts',(-0.770079973816217,-6.72561226535755,
146.160889255446));
#44829=CARTESIAN_POINT('Ctrl Pts',(-0.584779770558881,-6.74168536939726,
146.169638237841));
#44830=CARTESIAN_POINT('Ctrl Pts',(-0.391490647560342,-6.75845143942357,
146.178764418517));
#44831=CARTESIAN_POINT('Ctrl Pts',(-0.197480213110766,-6.76689975924008,
146.187890599193));
#44832=CARTESIAN_POINT('Ctrl Pts',(-0.00346532630421726,-6.76699911271707,
146.197016779869));
#44833=CARTESIAN_POINT('Ctrl Pts',(0.184486595289723,-6.76709536139791,
146.205857767399));
#44834=CARTESIAN_POINT('Ctrl Pts',(0.372442378178995,-6.75935659726805,
146.214698754929));
#44835=CARTESIAN_POINT('Ctrl Pts',(0.559750217715953,-6.74380965729067,
146.223539742459));
#44836=CARTESIAN_POINT('Ctrl Pts',(0.745129914451633,-6.72842275717321,
146.232289721057));
#44837=CARTESIAN_POINT('Ctrl Pts',(0.929874656308079,-6.70538772273558,
146.241039699655));
#44838=CARTESIAN_POINT('Ctrl Pts',(1.11335688289169,-6.67478280180844,146.249789678252));
#44839=CARTESIAN_POINT('Ctrl Pts',(1.29683723118251,-6.64417819418142,146.258539567277));
#44840=CARTESIAN_POINT('Ctrl Pts',(1.47905480729632,-6.6060039023021,146.267289456302));
#44841=CARTESIAN_POINT('Ctrl Pts',(1.65939064804209,-6.56038959797286,146.276039345327));
#44842=CARTESIAN_POINT('Ctrl Pts',(1.83972470263675,-6.51477574543423,146.284789147688));
#44843=CARTESIAN_POINT('Ctrl Pts',(2.01817678125268,-6.46172209820281,146.293538950049));
#44844=CARTESIAN_POINT('Ctrl Pts',(2.1941407234711,-6.4014088672421,146.30228875241));
#44845=CARTESIAN_POINT('Ctrl Pts',(2.37010298131527,-6.34109621361587,146.311038471016));
#44846=CARTESIAN_POINT('Ctrl Pts',(2.54357687926344,-6.27352420826201,146.319788189621));
#44847=CARTESIAN_POINT('Ctrl Pts',(2.71397317789404,-6.19892237325745,146.328537908227));
#44848=CARTESIAN_POINT('Ctrl Pts',(2.88436790206646,-6.12432122757225,146.337287545985));
#44849=CARTESIAN_POINT('Ctrl Pts',(3.05168482125713,-6.04269049717691,146.346037183743));
#44850=CARTESIAN_POINT('Ctrl Pts',(3.21535561996858,-5.95430745235216,146.354786821501));
#44851=CARTESIAN_POINT('Ctrl Pts',(3.37902496074756,-5.86592519481819,146.36353638132));
#44852=CARTESIAN_POINT('Ctrl Pts',(3.53904799384358,-5.77079087940549,146.372285941139));
#44853=CARTESIAN_POINT('Ctrl Pts',(3.69488118814475,-5.66922763747356,146.381035500958));
#44854=CARTESIAN_POINT('Ctrl Pts',(3.85071304610335,-5.56766526649396,146.389784985746));
#44855=CARTESIAN_POINT('Ctrl Pts',(4.00235489705481,-5.4596742358107,146.398534470533));
#44856=CARTESIAN_POINT('Ctrl Pts',(4.14929168607179,-5.34562133936697,146.407283955321));
#44857=CARTESIAN_POINT('Ctrl Pts',(4.29622726385282,-5.2315693830892,146.416033367984));
#44858=CARTESIAN_POINT('Ctrl Pts',(4.43845763091594,-5.11145583677613,146.424782780647));
#44859=CARTESIAN_POINT('Ctrl Pts',(4.57549970660492,-4.98568866204643,146.433532193311));
#44860=CARTESIAN_POINT('Ctrl Pts',(4.71254069814829,-4.85992248226612,146.442281536757));
#44861=CARTESIAN_POINT('Ctrl Pts',(4.84439326930854,-4.72850295734473,146.451030880203));
#44862=CARTESIAN_POINT('Ctrl Pts',(4.97060959434246,-4.59187644222171,146.45978022365));
#44863=CARTESIAN_POINT('Ctrl Pts',(5.09682496280072,-4.4552509625717,146.468529500786));
#44864=CARTESIAN_POINT('Ctrl Pts',(5.21740397615406,-4.31341878218849,146.477278777922));
#44865=CARTESIAN_POINT('Ctrl Pts',(5.33193710451512,-4.16686161439217,146.486028055058));
#44866=CARTESIAN_POINT('Ctrl Pts',(5.44646940288973,-4.02030550865069,146.494777268791));
#44867=CARTESIAN_POINT('Ctrl Pts',(5.55495572749267,-3.86902470980705,146.503526482524));
#44868=CARTESIAN_POINT('Ctrl Pts',(5.65702762491071,-3.71353301466368,146.512275696257));
#44869=CARTESIAN_POINT('Ctrl Pts',(5.75909881654779,-3.55804239467499,146.521024849493));
#44870=CARTESIAN_POINT('Ctrl Pts',(5.8547555125042,-3.39834117620177,146.52977400273));
#44871=CARTESIAN_POINT('Ctrl Pts',(5.94367283727745,-3.23497174692612,146.538523155966));
#44872=CARTESIAN_POINT('Ctrl Pts',(6.03258957675987,-3.07160339301603,146.547272251611));
#44873=CARTESIAN_POINT('Ctrl Pts',(6.11476689684985,-2.90456712830135,146.556021347257));
#44874=CARTESIAN_POINT('Ctrl Pts',(6.18992570524986,-2.73443024476528,146.564770442902));
#44875=CARTESIAN_POINT('Ctrl Pts',(6.26508404388437,-2.56429442463666,146.573519483863));
#44876=CARTESIAN_POINT('Ctrl Pts',(6.3332238428307,-2.39105828656642,146.582268524824));
#44877=CARTESIAN_POINT('Ctrl Pts',(6.39411368719803,-2.21531017132743,146.591017565785));
#44878=CARTESIAN_POINT('Ctrl Pts',(6.45500317120682,-2.03956309620174,146.599766554968));
#44879=CARTESIAN_POINT('Ctrl Pts',(6.50864269269886,-1.86130434439289,146.60851554415));
#44880=CARTESIAN_POINT('Ctrl Pts',(6.55485008446166,-1.68113930720596,146.617264533333));
#44881=CARTESIAN_POINT('Ctrl Pts',(6.60199664749259,-1.49731239212479,146.626191346862));
#44882=CARTESIAN_POINT('Ctrl Pts',(6.64140563640784,-1.31150116500296,146.635118160391));
#44883=CARTESIAN_POINT('Ctrl Pts',(6.67293772282069,-1.1243625515627,146.644044973921));
#44884=CARTESIAN_POINT('Ctrl Pts',(6.70384494949784,-0.940932395057531,
146.652794888076));
#44885=CARTESIAN_POINT('Ctrl Pts',(6.7271844934886,-0.756227260512984,146.661544802232));
#44886=CARTESIAN_POINT('Ctrl Pts',(6.74287707373878,-0.570874564548037,
146.670294716387));
#44887=CARTESIAN_POINT('Ctrl Pts',(6.75856934538633,-0.385525513638917,
146.679044458471));
#44888=CARTESIAN_POINT('Ctrl Pts',(6.76661493004084,-0.199529212424761,
146.687794200555));
#44889=CARTESIAN_POINT('Ctrl Pts',(6.76698649908905,-0.0135174386070417,
146.696543942639));
#44890=CARTESIAN_POINT('Ctrl Pts',(6.76735806132406,0.172490924439112,146.705293524285));
#44891=CARTESIAN_POINT('Ctrl Pts',(6.76005588896325,0.358514472894699,146.714043105931));
#44892=CARTESIAN_POINT('Ctrl Pts',(6.74510478454639,0.543921359655468,146.722792687577));
#44893=CARTESIAN_POINT('Ctrl Pts',(6.7301539344076,0.729325093143771,146.731542120416));
#44894=CARTESIAN_POINT('Ctrl Pts',(6.70755443556987,0.914111900249756,146.740291553255));
#44895=CARTESIAN_POINT('Ctrl Pts',(6.67738304682426,1.09765415590887,146.749040986094));
#44896=CARTESIAN_POINT('Ctrl Pts',(6.64721213111984,1.28119353390633,146.757790281755));
#44897=CARTESIAN_POINT('Ctrl Pts',(6.60946960955634,1.46348811672024,146.766539577417));
#44898=CARTESIAN_POINT('Ctrl Pts',(6.56428366991337,1.64391876347605,146.775288873078));
#44899=CARTESIAN_POINT('Ctrl Pts',(6.5190983786789,1.824346821091,146.784038043189));
#44900=CARTESIAN_POINT('Ctrl Pts',(6.46646995272111,2.00291071819832,146.7927872133));
#44901=CARTESIAN_POINT('Ctrl Pts',(6.40657713281757,2.17900400212094,146.80153638341));
#44902=CARTESIAN_POINT('Ctrl Pts',(6.34668509279284,2.35509499309053,146.810285439596));
#44903=CARTESIAN_POINT('Ctrl Pts',(6.27952894037767,2.52871516397523,146.819034495782));
#44904=CARTESIAN_POINT('Ctrl Pts',(6.20533675061705,2.69927486770826,146.827783551968));
#44905=CARTESIAN_POINT('Ctrl Pts',(6.12832117908181,2.87632521635362,146.83686555325));
#44906=CARTESIAN_POINT('Ctrl Pts',(6.04372366626347,3.05007728919468,146.845947554532));
#44907=CARTESIAN_POINT('Ctrl Pts',(5.95185378008137,3.21989527477697,146.855029555815));
#44908=CARTESIAN_POINT('Ctrl Pts',(5.86334450817657,3.38350129286257,146.863779336122));
#44909=CARTESIAN_POINT('Ctrl Pts',(5.76808562057557,3.54345567124471,146.872529116429));
#44910=CARTESIAN_POINT('Ctrl Pts',(5.66640068804801,3.69921508464823,146.881278896736));
#44911=CARTESIAN_POINT('Ctrl Pts',(5.56471941108251,3.8549688985181,146.890028362489));
#44912=CARTESIAN_POINT('Ctrl Pts',(5.45661270815451,4.00652780919178,146.898777828243));
#44913=CARTESIAN_POINT('Ctrl Pts',(5.3424477644946,4.15337704568785,146.907527293996));
#44914=CARTESIAN_POINT('Ctrl Pts',(5.22828631819954,4.30022178355814,146.916276491716));
#44915=CARTESIAN_POINT('Ctrl Pts',(5.1080671784444,4.44235690972252,146.925025689436));
#44916=CARTESIAN_POINT('Ctrl Pts',(4.98219864545103,4.57929969070227,146.933774887155));
#44917=CARTESIAN_POINT('Ctrl Pts',(4.85633329944421,4.71623900429592,146.942523863345));
#44918=CARTESIAN_POINT('Ctrl Pts',(4.72481904034057,4.84798602483218,146.951272839536));
#44919=CARTESIAN_POINT('Ctrl Pts',(4.58810250737619,4.97409332258737,146.960021815726));
#44920=CARTESIAN_POINT('Ctrl Pts',(4.45137708686068,5.10020881821763,146.968771360662));
#44921=CARTESIAN_POINT('Ctrl Pts',(4.30944892636482,5.22068366307578,146.977520905598));
#44922=CARTESIAN_POINT('Ctrl Pts',(4.16280009467095,5.33510865604512,146.986270450534));
#44923=CARTESIAN_POINT('Ctrl Pts',(4.01615988349229,5.44952692272567,146.995019481143));
#44924=CARTESIAN_POINT('Ctrl Pts',(3.86479978232677,5.55789587288316,147.003768511751));
#44925=CARTESIAN_POINT('Ctrl Pts',(3.70923383581518,5.65984746713583,147.012517542359));
#44926=CARTESIAN_POINT('Ctrl Pts',(3.55366577800002,5.76180044505098,147.021266691707));
#44927=CARTESIAN_POINT('Ctrl Pts',(3.39389200027312,5.85733573570785,147.030015841055));
#44928=CARTESIAN_POINT('Ctrl Pts',(3.23045513626524,5.94612887621666,147.038764990403));
#44929=CARTESIAN_POINT('Ctrl Pts',(3.18695122151905,5.96976399206515,147.041093854516));
#44930=CARTESIAN_POINT('Ctrl Pts',(3.14318791262833,5.99292165435246,147.043422718629));
#44931=CARTESIAN_POINT('Ctrl Pts',(3.09917575053267,6.01559628526635,147.045751582743));
#44932=CARTESIAN_POINT('Ctrl Pts',(3.09917575053269,6.01559628526634,145.045580110739));
#44933=CARTESIAN_POINT('Ctrl Pts',(2.9439233683427,6.09558077812104,145.05380430615));
#44934=CARTESIAN_POINT('Ctrl Pts',(2.78571726968034,6.16947671695349,145.062028501561));
#44935=CARTESIAN_POINT('Ctrl Pts',(2.62508186159937,6.23708539462961,145.070252696972));
#44936=CARTESIAN_POINT('Ctrl Pts',(2.49964395324186,6.28988005065112,145.076674854344));
#44937=CARTESIAN_POINT('Ctrl Pts',(2.37272511858934,6.33884180682753,145.083097011717));
#44938=CARTESIAN_POINT('Ctrl Pts',(2.24458091329037,6.38389736161951,145.089519169089));
#44939=CARTESIAN_POINT('Ctrl Pts',(2.0720689977826,6.44455262139732,145.098164887149));
#44940=CARTESIAN_POINT('Ctrl Pts',(1.89694273773663,6.4982653745132,145.106810605209));
#44941=CARTESIAN_POINT('Ctrl Pts',(1.71977518678143,6.54481950147832,145.115456323269));
#44942=CARTESIAN_POINT('Ctrl Pts',(1.54283508285712,6.59131386243156,145.124090941989));
#44943=CARTESIAN_POINT('Ctrl Pts',(1.36385920719454,6.63066784586529,145.132725560709));
#44944=CARTESIAN_POINT('Ctrl Pts',(1.18343739809782,6.66271453123901,145.141360179429));
#44945=CARTESIAN_POINT('Ctrl Pts',(0.996643791826336,6.69589298100611,145.150299739327));
#44946=CARTESIAN_POINT('Ctrl Pts',(0.808300551939153,6.72123844830351,145.159239299226));
#44947=CARTESIAN_POINT('Ctrl Pts',(0.619078821817926,6.73862229334577,145.168178859125));
#44948=CARTESIAN_POINT('Ctrl Pts',(0.436818986978534,6.75536654742401,145.176789512402));
#44949=CARTESIAN_POINT('Ctrl Pts',(0.253744494266675,6.76472450344558,145.18540016568));
#44950=CARTESIAN_POINT('Ctrl Pts',(0.0704653816734188,6.76663310886482,
145.194010818958));
#44951=CARTESIAN_POINT('Ctrl Pts',(-0.112640244974695,6.76853990766132,
145.202613321676));
#44952=CARTESIAN_POINT('Ctrl Pts',(-0.295949801375999,6.76301141110478,
145.211215824394));
#44953=CARTESIAN_POINT('Ctrl Pts',(-0.478849452261388,6.75003645931405,
145.219818327112));
#44954=CARTESIAN_POINT('Ctrl Pts',(-0.661543253267038,6.73707611057069,
145.228411147886));
#44955=CARTESIAN_POINT('Ctrl Pts',(-0.84382776553683,6.71668604764664,145.237003968661));
#44956=CARTESIAN_POINT('Ctrl Pts',(-1.02509026510326,6.68890715650849,145.245596789435));
#44957=CARTESIAN_POINT('Ctrl Pts',(-1.04645287332205,6.68563328811566,145.246609492361));
#44958=CARTESIAN_POINT('Ctrl Pts',(-1.06780128811058,6.68225685065292,145.247622195287));
#44959=CARTESIAN_POINT('Ctrl Pts',(-1.08913450867068,6.67877795873038,145.248634898213));
#44960=CARTESIAN_POINT('Ctrl Pts',(-1.27019898926127,6.64925106394149,145.25723015596));
#44961=CARTESIAN_POINT('Ctrl Pts',(-1.44995535059435,6.61237420054901,145.265825413708));
#44962=CARTESIAN_POINT('Ctrl Pts',(-1.62780734683736,6.56829751469757,145.274420671455));
#44963=CARTESIAN_POINT('Ctrl Pts',(-1.80582589392731,6.52417955290033,145.283023978297));
#44964=CARTESIAN_POINT('Ctrl Pts',(-1.98193621989576,6.47284838414931,145.291627285139));
#44965=CARTESIAN_POINT('Ctrl Pts',(-2.15555740029556,6.41450397879922,145.30023059198));
#44966=CARTESIAN_POINT('Ctrl Pts',(-2.33637697543853,6.35374059403776,145.309190594927));
#44967=CARTESIAN_POINT('Ctrl Pts',(-2.51449624819373,6.28537017245824,145.318150597873));
#44968=CARTESIAN_POINT('Ctrl Pts',(-2.6892834913913,6.20967336523671,145.327110600819));
#44969=CARTESIAN_POINT('Ctrl Pts',(-2.85757162120232,6.13679119210479,145.335737444011));
#44970=CARTESIAN_POINT('Ctrl Pts',(-3.02277079659474,6.05711781313992,145.344364287202));
#44971=CARTESIAN_POINT('Ctrl Pts',(-3.18434321852858,5.97095028170651,145.352991130394));
#44972=CARTESIAN_POINT('Ctrl Pts',(-3.34607006285292,5.88470039589586,145.361626218667));
#44973=CARTESIAN_POINT('Ctrl Pts',(-3.50416297030758,5.79194411997024,145.370261306939));
#44974=CARTESIAN_POINT('Ctrl Pts',(-3.65811206393917,5.69302249491979,145.378896395212));
#44975=CARTESIAN_POINT('Ctrl Pts',(-3.81228980286979,5.59395395140424,145.387544308324));
#44976=CARTESIAN_POINT('Ctrl Pts',(-3.96231117723578,5.48870193191362,145.396192221436));
#44977=CARTESIAN_POINT('Ctrl Pts',(-4.10769718875882,5.37764937546721,145.404840134547));
#44978=CARTESIAN_POINT('Ctrl Pts',(-4.12400728703292,5.3651909684289,145.40581029881));
#44979=CARTESIAN_POINT('Ctrl Pts',(-4.14025908368601,5.35265959902519,145.406780463073));
#44980=CARTESIAN_POINT('Ctrl Pts',(-4.15645193036076,5.34005583777925,145.407750627336));
#44981=CARTESIAN_POINT('Ctrl Pts',(-4.29185953005773,5.23466083887976,145.41586332159));
#44982=CARTESIAN_POINT('Ctrl Pts',(-4.42346060361134,5.12395270312488,145.423976015843));
#44983=CARTESIAN_POINT('Ctrl Pts',(-4.55080472908244,5.00823974244054,145.432088710096));
#44984=CARTESIAN_POINT('Ctrl Pts',(-4.67801292831267,4.89265029297204,145.440192744916));
#44985=CARTESIAN_POINT('Ctrl Pts',(-4.80097295277972,4.77206689778212,145.448296779735));
#44986=CARTESIAN_POINT('Ctrl Pts',(-4.91926491135886,4.64683997269903,145.456400814555));
#44987=CARTESIAN_POINT('Ctrl Pts',(-5.03745599628963,4.52171983506759,145.464497938646));
#44988=CARTESIAN_POINT('Ctrl Pts',(-5.15098668773628,4.39196431732556,145.472595062737));
#44989=CARTESIAN_POINT('Ctrl Pts',(-5.25947168751103,4.25796272509165,145.480692186829));
#44990=CARTESIAN_POINT('Ctrl Pts',(-5.36788744554687,4.12404666084116,145.488784142842));
#44991=CARTESIAN_POINT('Ctrl Pts',(-5.47126369259091,3.98589020426211,145.496876098855));
#44992=CARTESIAN_POINT('Ctrl Pts',(-5.56925343928991,3.84391793993544,145.504968054869));
#44993=CARTESIAN_POINT('Ctrl Pts',(-5.66721119758169,3.70199202195374,145.513057369291));
#44994=CARTESIAN_POINT('Ctrl Pts',(-5.75978574337875,3.55625307726772,145.521146683714));
#44995=CARTESIAN_POINT('Ctrl Pts',(-5.84667163970565,3.40715713424868,145.529235998137));
#44996=CARTESIAN_POINT('Ctrl Pts',(-5.93354430905497,3.25808388868432,145.537324081092));
#44997=CARTESIAN_POINT('Ctrl Pts',(-6.01472986596867,3.10565498064337,145.545412164047));
#44998=CARTESIAN_POINT('Ctrl Pts',(-6.08996739788074,2.95035355385582,145.553500247002));
#44999=CARTESIAN_POINT('Ctrl Pts',(-6.16520808407557,2.79504561616076,145.561588669045));
#45000=CARTESIAN_POINT('Ctrl Pts',(-6.2345000875311,2.63686525240069,145.569677091087));
#45001=CARTESIAN_POINT('Ctrl Pts',(-6.29762951322042,2.47631813671328,145.577765513129));
#45002=CARTESIAN_POINT('Ctrl Pts',(-6.36077384375081,2.3157331158934,145.585855844846));
#45003=CARTESIAN_POINT('Ctrl Pts',(-6.41775256505008,2.15278057455462,145.593946176563));
#45004=CARTESIAN_POINT('Ctrl Pts',(-6.46840080796771,1.9879839002071,145.60203650828));
#45005=CARTESIAN_POINT('Ctrl Pts',(-6.51909944905326,1.82302324286654,145.610134890383));
#45006=CARTESIAN_POINT('Ctrl Pts',(-6.5634549203035,1.65621514058114,145.618233272485));
#45007=CARTESIAN_POINT('Ctrl Pts',(-6.60135270114207,1.48809660812874,145.626331654588));
#45008=CARTESIAN_POINT('Ctrl Pts',(-6.63926980182875,1.31989237080289,145.634434165152));
#45009=CARTESIAN_POINT('Ctrl Pts',(-6.67072258577455,1.15037673503887,145.642536675715));
#45010=CARTESIAN_POINT('Ctrl Pts',(-6.69564817523386,0.980094135013302,
145.650639186279));
#45011=CARTESIAN_POINT('Ctrl Pts',(-6.72061010657903,0.809563260385306,
145.658753510425));
#45012=CARTESIAN_POINT('Ctrl Pts',(-6.73902578995366,0.63826355426418,145.666867834572));
#45013=CARTESIAN_POINT('Ctrl Pts',(-6.75088439156448,0.466742896819157,
145.674982158718));
#45014=CARTESIAN_POINT('Ctrl Pts',(-6.76163788249994,0.311206359239643,
145.682340303803));
#45015=CARTESIAN_POINT('Ctrl Pts',(-6.76700013085047,0.155488341605922,
145.689698448888));
#45016=CARTESIAN_POINT('Ctrl Pts',(-6.76699999999761,-5.6946322475613E-6,
145.697056593973));
#45017=CARTESIAN_POINT('',(-6.76699866775558,0.00424624472223871,145.302820216218));
#45018=CARTESIAN_POINT('Ctrl Pts',(3.0991757505327,6.01559628526633,144.651598619988));
#45019=CARTESIAN_POINT('Ctrl Pts',(2.94554257394182,6.09474657939993,144.65973337502));
#45020=CARTESIAN_POINT('Ctrl Pts',(2.78871523524756,6.16808998521787,144.667868130051));
#45021=CARTESIAN_POINT('Ctrl Pts',(2.62917701709088,6.23536023119764,144.676002885083));
#45022=CARTESIAN_POINT('Ctrl Pts',(2.46975342994266,6.30258214232559,144.684131795151));
#45023=CARTESIAN_POINT('Ctrl Pts',(2.30762317732625,6.36373944112315,144.692260705218));
#45024=CARTESIAN_POINT('Ctrl Pts',(2.14329310126062,6.41861228631927,144.700389615286));
#45025=CARTESIAN_POINT('Ctrl Pts',(1.97904658299517,6.4734572300238,144.708514392003));
#45026=CARTESIAN_POINT('Ctrl Pts',(1.81260281499707,6.52202396866606,144.716639168719));
#45027=CARTESIAN_POINT('Ctrl Pts',(1.64448752408125,6.56414120682524,144.724763945436));
#45028=CARTESIAN_POINT('Ctrl Pts',(1.47639578656538,6.6062525442472,144.73288758385));
#45029=CARTESIAN_POINT('Ctrl Pts',(1.30663334483601,6.6419160836238,144.741011222264));
#45030=CARTESIAN_POINT('Ctrl Pts',(1.13574020417337,6.67101065721111,144.749134860678));
#45031=CARTESIAN_POINT('Ctrl Pts',(0.964853908587294,6.70010406542349,144.757258173702));
#45032=CARTESIAN_POINT('Ctrl Pts',(0.792837364671338,6.72262896917097,144.765381486726));
#45033=CARTESIAN_POINT('Ctrl Pts',(0.620239680184277,6.73851554417773,144.77350479975));
#45034=CARTESIAN_POINT('Ctrl Pts',(0.447616073412362,6.75440450517434,144.781629332806));
#45035=CARTESIAN_POINT('Ctrl Pts',(0.274411516545912,6.76365311816404,144.789753865863));
#45036=CARTESIAN_POINT('Ctrl Pts',(0.101179091980249,6.76624355099239,144.79787839892));
#45037=CARTESIAN_POINT('Ctrl Pts',(-0.0721123087947992,6.76883486572208,
144.806005697938));
#45038=CARTESIAN_POINT('Ctrl Pts',(-0.24543123060132,6.76476348102892,144.814132996955));
#45039=CARTESIAN_POINT('Ctrl Pts',(-0.418225783397205,6.75406368004491,
144.822260295973));
#45040=CARTESIAN_POINT('Ctrl Pts',(-0.591219031196919,6.74335157544968,
144.830396940504));
#45041=CARTESIAN_POINT('Ctrl Pts',(-0.7636863400305,6.72599585161625,144.838533585035));
#45042=CARTESIAN_POINT('Ctrl Pts',(-0.935081153500462,6.70208267901615,
144.846670229565));
#45043=CARTESIAN_POINT('Ctrl Pts',(-1.10657756852881,6.6781553308669,144.854811697438));
#45044=CARTESIAN_POINT('Ctrl Pts',(-1.27699986206859,6.64766285280158,144.86295316531));
#45045=CARTESIAN_POINT('Ctrl Pts',(-1.44581314006289,6.61074227027657,144.871094633183));
#45046=CARTESIAN_POINT('Ctrl Pts',(-1.61489533330733,6.57376287420443,144.879249070206));
#45047=CARTESIAN_POINT('Ctrl Pts',(-1.78236303600487,6.53033500518731,144.887403507229));
#45048=CARTESIAN_POINT('Ctrl Pts',(-1.94769672303461,6.4806455291954,144.895557944253));
#45049=CARTESIAN_POINT('Ctrl Pts',(-2.10093493824198,6.43459123286666,144.903115819468));
#45050=CARTESIAN_POINT('Ctrl Pts',(-2.25233994001898,6.38315859856928,144.910673694684));
#45051=CARTESIAN_POINT('Ctrl Pts',(-2.40151557817402,6.32653237783444,144.918231569899));
#45052=CARTESIAN_POINT('Ctrl Pts',(-2.56401766669649,6.26484751260877,144.92646462003));
#45053=CARTESIAN_POINT('Ctrl Pts',(-2.72437915358357,6.19680745619827,144.934697670162));
#45054=CARTESIAN_POINT('Ctrl Pts',(-2.88206742583381,6.12257922390129,144.942930720293));
#45055=CARTESIAN_POINT('Ctrl Pts',(-3.03956791559096,6.04843938601893,144.951153966127));
#45056=CARTESIAN_POINT('Ctrl Pts',(-3.19440120872991,5.96812619713585,144.959377211961));
#45057=CARTESIAN_POINT('Ctrl Pts',(-3.34605151341352,5.88185585249954,144.967600457795));
#45058=CARTESIAN_POINT('Ctrl Pts',(-3.49755157903101,5.79567097538695,144.975815556908));
#45059=CARTESIAN_POINT('Ctrl Pts',(-3.64587462697365,5.703540871759,144.984030656021));
#45060=CARTESIAN_POINT('Ctrl Pts',(-3.79052637866044,5.60572910268409,144.992245755134));
#45061=CARTESIAN_POINT('Ctrl Pts',(-3.93506376660752,5.50799466499003,145.000454359272));
#45062=CARTESIAN_POINT('Ctrl Pts',(-4.07593534427567,5.40458770875781,145.00866296341));
#45063=CARTESIAN_POINT('Ctrl Pts',(-4.21267283740553,5.29581689307567,145.016871567548));
#45064=CARTESIAN_POINT('Ctrl Pts',(-4.34932957523257,5.1871103159572,145.025075323796));
#45065=CARTESIAN_POINT('Ctrl Pts',(-4.48185681282941,5.07304641250351,145.033279080045));
#45066=CARTESIAN_POINT('Ctrl Pts',(-4.60981652639567,4.95397624065451,145.041482836293));
#45067=CARTESIAN_POINT('Ctrl Pts',(-4.73773837990794,4.83494129866817,145.049684165256));
#45068=CARTESIAN_POINT('Ctrl Pts',(-4.86109513684568,4.71090327970509,145.05788549422));
#45069=CARTESIAN_POINT('Ctrl Pts',(-4.9794828705545,4.58225264928226,145.066086823184));
#45070=CARTESIAN_POINT('Ctrl Pts',(-5.09785427746469,4.4536197610095,145.074287021106));
#45071=CARTESIAN_POINT('Ctrl Pts',(-5.2112577828604,4.32037579122047,145.082487219028));
#45072=CARTESIAN_POINT('Ctrl Pts',(-5.31932726298064,4.18294710333647,145.09068741695));
#45073=CARTESIAN_POINT('Ctrl Pts',(-5.4274014236763,4.04551246330632,145.098887970029));
#45074=CARTESIAN_POINT('Ctrl Pts',(-5.53014087731727,3.90389302571494,145.107088523108));
#45075=CARTESIAN_POINT('Ctrl Pts',(-5.62722061241426,3.75854721657452,145.115289076187));
#45076=CARTESIAN_POINT('Ctrl Pts',(-5.72432214486191,3.61316877288308,145.123491470539));
#45077=CARTESIAN_POINT('Ctrl Pts',(-5.81576122877437,3.46406258908148,145.131693864892));
#45078=CARTESIAN_POINT('Ctrl Pts',(-5.9012568753538,3.31171500752851,145.139896259244));
#45079=CARTESIAN_POINT('Ctrl Pts',(-5.98683247539223,3.15922495420528,145.148106324277));
#45080=CARTESIAN_POINT('Ctrl Pts',(-6.06645335779164,3.00348775974395,145.156316389311));
#45081=CARTESIAN_POINT('Ctrl Pts',(-6.13988467878509,2.84501408278062,145.164526454344));
#45082=CARTESIAN_POINT('Ctrl Pts',(-6.21335114270621,2.6864645631266,145.172740448568));
#45083=CARTESIAN_POINT('Ctrl Pts',(-6.28062200120726,2.52517628027051,145.180954442793));
#45084=CARTESIAN_POINT('Ctrl Pts',(-6.341511105684,2.36167861837434,145.189168437017));
#45085=CARTESIAN_POINT('Ctrl Pts',(-6.40248322228989,2.19795805471039,145.197393629652));
#45086=CARTESIAN_POINT('Ctrl Pts',(-6.4570560849287,2.03202243269057,145.205618822286));
#45087=CARTESIAN_POINT('Ctrl Pts',(-6.50509349167212,1.86441617258728,145.213844014921));
#45088=CARTESIAN_POINT('Ctrl Pts',(-6.54829342872336,1.71368822166918,145.22124091305));
#45089=CARTESIAN_POINT('Ctrl Pts',(-6.58620854212007,1.56160951137961,145.228637811178));
#45090=CARTESIAN_POINT('Ctrl Pts',(-6.61877538971471,1.408581321936,145.236034709307));
#45091=CARTESIAN_POINT('Ctrl Pts',(-6.66778227040013,1.17830314718247,145.247165627121));
#45092=CARTESIAN_POINT('Ctrl Pts',(-6.70477811017182,0.945412940415503,
145.258296544934));
#45093=CARTESIAN_POINT('Ctrl Pts',(-6.72954515647865,0.710992958414298,
145.269427462748));
#45094=CARTESIAN_POINT('Ctrl Pts',(-6.75431220278549,0.476572976413092,
145.280558380562));
#45095=CARTESIAN_POINT('Ctrl Pts',(-6.76685034307383,0.24062281924469,145.291689298376));
#45096=CARTESIAN_POINT('Ctrl Pts',(-6.7669986677552,0.00424624532204132,
145.30282021619));
#45097=CARTESIAN_POINT('Ctrl Pts',(-6.76699866775558,0.00424624472224321,
145.302820216218));
#45098=CARTESIAN_POINT('Ctrl Pts',(-6.76710532578424,-0.165728588349608,
145.31082429152));
#45099=CARTESIAN_POINT('Ctrl Pts',(-6.76080360179688,-0.335917030645911,
145.318828366822));
#45100=CARTESIAN_POINT('Ctrl Pts',(-6.74807175566877,-0.505783135687022,
145.326832442124));
#45101=CARTESIAN_POINT('Ctrl Pts',(-6.73534832620318,-0.67553694706182,
145.334831226159));
#45102=CARTESIAN_POINT('Ctrl Pts',(-6.71620325708614,-0.844968469928021,
145.342830010194));
#45103=CARTESIAN_POINT('Ctrl Pts',(-6.69066686053985,-1.01354129727105,
145.350828794229));
#45104=CARTESIAN_POINT('Ctrl Pts',(-6.66514176758924,-1.18203950644778,
145.35882403763));
#45105=CARTESIAN_POINT('Ctrl Pts',(-6.63323103058441,-1.34967940315641,
145.366819281032));
#45106=CARTESIAN_POINT('Ctrl Pts',(-6.59501682831114,-1.51592942919285,
145.374814524433));
#45107=CARTESIAN_POINT('Ctrl Pts',(-6.56295873406291,-1.65539744596142,
145.381521775959));
#45108=CARTESIAN_POINT('Ctrl Pts',(-6.52646542676354,-1.79388728555138,
145.388229027485));
#45109=CARTESIAN_POINT('Ctrl Pts',(-6.48561325923976,-1.93109027535571,
145.39493627901));
#45110=CARTESIAN_POINT('Ctrl Pts',(-6.43325868069639,-2.10692438995726,
145.403532036545));
#45111=CARTESIAN_POINT('Ctrl Pts',(-6.37378001956298,-2.2805249665359,145.41212779408));
#45112=CARTESIAN_POINT('Ctrl Pts',(-6.30740207231591,-2.45131966461843,
145.420723551615));
#45113=CARTESIAN_POINT('Ctrl Pts',(-6.24096219218916,-2.62227371995626,
145.429327329284));
#45114=CARTESIAN_POINT('Ctrl Pts',(-6.16761028752212,-2.7904163866458,145.437931106953));
#45115=CARTESIAN_POINT('Ctrl Pts',(-6.08761862570831,-2.95519685772865,
145.446534884621));
#45116=CARTESIAN_POINT('Ctrl Pts',(-6.00448322145325,-3.12645334579485,
145.455476798296));
#45117=CARTESIAN_POINT('Ctrl Pts',(-5.91417578569463,-3.29407768641138,
145.46441871197));
#45118=CARTESIAN_POINT('Ctrl Pts',(-5.81705280286035,-3.4574825652105,145.473360625644));
#45119=CARTESIAN_POINT('Ctrl Pts',(-5.72334807106682,-3.61513639641286,
145.481987827962));
#45120=CARTESIAN_POINT('Ctrl Pts',(-5.6232995659211,-3.7688624904389,145.490615030279));
#45121=CARTESIAN_POINT('Ctrl Pts',(-5.51727027242546,-3.91816509874332,
145.499242232597));
#45122=CARTESIAN_POINT('Ctrl Pts',(-5.41114000225819,-4.06760989492768,
145.507877651004));
#45123=CARTESIAN_POINT('Ctrl Pts',(-5.29901775843554,-4.21262255349265,
145.51651306941));
#45124=CARTESIAN_POINT('Ctrl Pts',(-5.18130661292036,-4.35274060597548,
145.525148487817));
#45125=CARTESIAN_POINT('Ctrl Pts',(-5.06342156595441,-4.4930656629225,145.533796663825));
#45126=CARTESIAN_POINT('Ctrl Pts',(-4.93993131965913,-4.62848143545159,
145.542444839833));
#45127=CARTESIAN_POINT('Ctrl Pts',(-4.81127657989389,-4.75856140779591,
145.55109301584));
#45128=CARTESIAN_POINT('Ctrl Pts',(-4.79766539534225,-4.77232337656039,
145.552007960132));
#45129=CARTESIAN_POINT('Ctrl Pts',(-4.78399643654703,-4.78602565922484,
145.552922904423));
#45130=CARTESIAN_POINT('Ctrl Pts',(-4.77027024711876,-4.79966777698764,
145.553837848714));
#45131=CARTESIAN_POINT('Ctrl Pts',(-4.64686215219463,-4.92232000852181,
145.56206384126));
#45132=CARTESIAN_POINT('Ctrl Pts',(-4.51855863337628,-5.04037059823362,
145.570289833807));
#45133=CARTESIAN_POINT('Ctrl Pts',(-4.38573665410778,-5.15340693142076,
145.578515826354));
#45134=CARTESIAN_POINT('Ctrl Pts',(-4.2530539215162,-5.26632476062344,145.58673319501));
#45135=CARTESIAN_POINT('Ctrl Pts',(-4.1158624322524,-5.37423857123331,145.594950563667));
#45136=CARTESIAN_POINT('Ctrl Pts',(-3.97457654674478,-5.47677188442849,
145.603167932324));
#45137=CARTESIAN_POINT('Ctrl Pts',(-3.83341051053263,-5.57921822116947,
145.611378330392));
#45138=CARTESIAN_POINT('Ctrl Pts',(-3.68815728371712,-5.6762929413398,145.619588728459));
#45139=CARTESIAN_POINT('Ctrl Pts',(-3.53926498510135,-5.76765917554389,
145.627799126527));
#45140=CARTESIAN_POINT('Ctrl Pts',(-3.39046920379679,-5.8589661828884,145.636004202321));
#45141=CARTESIAN_POINT('Ctrl Pts',(-3.23803935388692,-5.9445718885637,145.644209278115));
#45142=CARTESIAN_POINT('Ctrl Pts',(-3.08245334911492,-6.02418213125485,
145.652414353909));
#45143=CARTESIAN_POINT('Ctrl Pts',(-2.9269370837608,-6.10375668968255,145.660615751884));
#45144=CARTESIAN_POINT('Ctrl Pts',(-2.76826780034502,-6.17734097632867,
145.668817149859));
#45145=CARTESIAN_POINT('Ctrl Pts',(-2.60694895810223,-6.24468623149712,
145.677018547834));
#45146=CARTESIAN_POINT('Ctrl Pts',(-2.44564275169426,-6.31202621162449,
145.685219303407));
#45147=CARTESIAN_POINT('Ctrl Pts',(-2.28168772685584,-6.37312798772671,
145.69342005898));
#45148=CARTESIAN_POINT('Ctrl Pts',(-2.11560866349979,-6.42779036550856,
145.701620814553));
#45149=CARTESIAN_POINT('Ctrl Pts',(-1.94953044374658,-6.48245246563147,
145.70982152847));
#45150=CARTESIAN_POINT('Ctrl Pts',(-1.78132854704235,-6.53067511953306,
145.718022242387));
#45151=CARTESIAN_POINT('Ctrl Pts',(-1.61154419120836,-6.57230662094995,
145.726222956304));
#45152=CARTESIAN_POINT('Ctrl Pts',(-1.44172992864499,-6.61394545556336,
145.734425114739));
#45153=CARTESIAN_POINT('Ctrl Pts',(-1.27033299967155,-6.6489907392495,145.742627273174));
#45154=CARTESIAN_POINT('Ctrl Pts',(-1.09790617863893,-6.67734161346463,
145.750829431609));
#45155=CARTESIAN_POINT('Ctrl Pts',(-0.925417737055973,-6.70570261949372,
145.759034521267));
#45156=CARTESIAN_POINT('Ctrl Pts',(-0.751899023627536,-6.72736439215343,
145.767239610926));
#45157=CARTESIAN_POINT('Ctrl Pts',(-0.577909376777984,-6.74227778664096,
145.775444700584));
#45158=CARTESIAN_POINT('Ctrl Pts',(-0.40372096732874,-6.75720821791838,
145.783659163587));
#45159=CARTESIAN_POINT('Ctrl Pts',(-0.229060907082588,-6.76537483871306,
145.79187362659));
#45160=CARTESIAN_POINT('Ctrl Pts',(-0.0544910606802038,-6.76678060264303,
145.800088089593));
#45161=CARTESIAN_POINT('Ctrl Pts',(0.12018221283816,-6.7681871994437,145.808307419406));
#45162=CARTESIAN_POINT('Ctrl Pts',(0.29476480836678,-6.76282496567511,145.816526749218));
#45163=CARTESIAN_POINT('Ctrl Pts',(0.468698637813905,-6.75074889082029,
145.824746079031));
#45164=CARTESIAN_POINT('Ctrl Pts',(0.642901967182734,-6.73865410481976,
145.832978144197));
#45165=CARTESIAN_POINT('Ctrl Pts',(0.816454165608605,-6.71982472772884,
145.841210209363));
#45166=CARTESIAN_POINT('Ctrl Pts',(0.988804675396828,-6.6943673572574,145.849442274529));
#45167=CARTESIAN_POINT('Ctrl Pts',(1.14372568761367,-6.67148444494887,145.856841845726));
#45168=CARTESIAN_POINT('Ctrl Pts',(1.29767573289346,-6.64324703872476,145.864241416924));
#45169=CARTESIAN_POINT('Ctrl Pts',(1.45026540971424,-6.60976695817533,145.871640988122));
#45170=CARTESIAN_POINT('Ctrl Pts',(1.61844255534776,-6.57286679232076,145.879796446531));
#45171=CARTESIAN_POINT('Ctrl Pts',(1.78548477583121,-6.52948366823578,145.88795190494));
#45172=CARTESIAN_POINT('Ctrl Pts',(1.95084858414145,-6.47969743134302,145.896107363348));
#45173=CARTESIAN_POINT('Ctrl Pts',(2.11601112296054,-6.42997179084476,145.904252895492));
#45174=CARTESIAN_POINT('Ctrl Pts',(2.2794989698499,-6.37385865492978,145.912398427636));
#45175=CARTESIAN_POINT('Ctrl Pts',(2.44077743612675,-6.31148908794862,145.92054395978));
#45176=CARTESIAN_POINT('Ctrl Pts',(2.60189351893728,-6.24918231785978,145.928681290583));
#45177=CARTESIAN_POINT('Ctrl Pts',(2.76080431140704,-6.18063178833523,145.936818621386));
#45178=CARTESIAN_POINT('Ctrl Pts',(2.91698893908493,-6.10601871347085,145.944955952188));
#45179=CARTESIAN_POINT('Ctrl Pts',(3.07304913471808,-6.03146508272467,145.953086799993));
#45180=CARTESIAN_POINT('Ctrl Pts',(3.22638716187806,-5.95085868063015,145.961217647797));
#45181=CARTESIAN_POINT('Ctrl Pts',(3.37650084473444,-5.86442930262678,145.969348495601));
#45182=CARTESIAN_POINT('Ctrl Pts',(3.52652646623596,-5.77805062678448,145.977474573597));
#45183=CARTESIAN_POINT('Ctrl Pts',(3.67333119436201,-5.68585595972377,145.985600651593));
#45184=CARTESIAN_POINT('Ctrl Pts',(3.81643625478613,-5.58812162655342,145.993726729589));
#45185=CARTESIAN_POINT('Ctrl Pts',(3.96004873955535,-5.49004074533051,146.00188162117));
#45186=CARTESIAN_POINT('Ctrl Pts',(4.09993493891927,-5.38638100644084,146.01003651275));
#45187=CARTESIAN_POINT('Ctrl Pts',(4.23563868442833,-5.27746662092469,146.018191404331));
#45188=CARTESIAN_POINT('Ctrl Pts',(4.37081323283637,-5.16897696338387,146.02631449469));
#45189=CARTESIAN_POINT('Ctrl Pts',(4.50183761251203,-5.05527381211952,146.034437585048));
#45190=CARTESIAN_POINT('Ctrl Pts',(4.62829291269694,-4.93671892194394,146.042560675407));
#45191=CARTESIAN_POINT('Ctrl Pts',(4.75475814272944,-4.81815472229703,146.050684403627));
#45192=CARTESIAN_POINT('Ctrl Pts',(4.87665331169783,-4.69473827504831,146.058808131848));
#45193=CARTESIAN_POINT('Ctrl Pts',(4.99359546364005,-4.56686909660366,146.066931860069));
#45194=CARTESIAN_POINT('Ctrl Pts',(5.11056904651986,-4.43896555032756,146.075057771731));
#45195=CARTESIAN_POINT('Ctrl Pts',(5.2225867148445,-4.3066071596935,146.083183683394));
#45196=CARTESIAN_POINT('Ctrl Pts',(5.32930502132712,-4.17022745059038,146.091309595056));
#45197=CARTESIAN_POINT('Ctrl Pts',(5.43670580239076,-4.03297557917606,146.099487472763));
#45198=CARTESIAN_POINT('Ctrl Pts',(5.53873897495106,-3.89165107307566,146.107665350469));
#45199=CARTESIAN_POINT('Ctrl Pts',(5.63509850285464,-3.74672575232367,146.115843228175));
#45200=CARTESIAN_POINT('Ctrl Pts',(5.73099812770412,-3.60249212858475,146.12398207465));
#45201=CARTESIAN_POINT('Ctrl Pts',(5.82127800915604,-3.45469233096788,146.132120921126));
#45202=CARTESIAN_POINT('Ctrl Pts',(5.90568266291211,-3.30381616997366,146.140259767602));
#45203=CARTESIAN_POINT('Ctrl Pts',(5.9906944820993,-3.15185468032441,146.148457160923));
#45204=CARTESIAN_POINT('Ctrl Pts',(6.06974605637035,-2.99677273730642,146.156654554244));
#45205=CARTESIAN_POINT('Ctrl Pts',(6.14262582048684,-2.83909088080822,146.164851947565));
#45206=CARTESIAN_POINT('Ctrl Pts',(6.21550558460327,-2.68140902431015,146.173049340887));
#45207=CARTESIAN_POINT('Ctrl Pts',(6.28221345195744,-2.52112762147068,146.181246734208));
#45208=CARTESIAN_POINT('Ctrl Pts',(6.34258911909827,-2.35878194547446,146.189444127529));
#45209=CARTESIAN_POINT('Ctrl Pts',(6.40317702262229,-2.19586558163773,146.197670336849));
#45210=CARTESIAN_POINT('Ctrl Pts',(6.45756855974203,-2.03038557931949,146.205896546168));
#45211=CARTESIAN_POINT('Ctrl Pts',(6.50554111361607,-1.86285367623198,146.214122755487));
#45212=CARTESIAN_POINT('Ctrl Pts',(6.55345977238034,-1.69550998806275,146.222339723013));
#45213=CARTESIAN_POINT('Ctrl Pts',(6.59497371003025,-1.52611933109708,146.230556690538));
#45214=CARTESIAN_POINT('Ctrl Pts',(6.62990852064688,-1.35521290130148,146.238773658064));
#45215=CARTESIAN_POINT('Ctrl Pts',(6.66481109519662,-1.1844641752691,146.246983043389));
#45216=CARTESIAN_POINT('Ctrl Pts',(6.69314656173241,-1.01220281108887,146.255192428715));
#45217=CARTESIAN_POINT('Ctrl Pts',(6.71479042235199,-0.838974721842076,
146.263401814041));
#45218=CARTESIAN_POINT('Ctrl Pts',(6.73641865381941,-0.665871721562182,
146.271605271324));
#45219=CARTESIAN_POINT('Ctrl Pts',(6.75136485969259,-0.491803741093733,
146.279808728607));
#45220=CARTESIAN_POINT('Ctrl Pts',(6.75955567154628,-0.317326524681699,
146.288012185889));
#45221=CARTESIAN_POINT('Ctrl Pts',(6.76774221182591,-0.142940299536919,
146.296211365004));
#45222=CARTESIAN_POINT('Ctrl Pts',(6.769180359736,0.0318543789915835,146.304410544118));
#45223=CARTESIAN_POINT('Ctrl Pts',(6.76384861027529,0.206496918323283,146.312609723232));
#45224=CARTESIAN_POINT('Ctrl Pts',(6.75851786543104,0.381106551238395,146.320807357444));
#45225=CARTESIAN_POINT('Ctrl Pts',(6.74641976878472,0.555563743767707,146.329004991656));
#45226=CARTESIAN_POINT('Ctrl Pts',(6.72758493374229,0.729307863171511,146.337202625868));
#45227=CARTESIAN_POINT('Ctrl Pts',(6.70875145821885,0.903039441534751,146.345399668366));
#45228=CARTESIAN_POINT('Ctrl Pts',(6.68318225050078,1.07605769259408,146.353596710864));
#45229=CARTESIAN_POINT('Ctrl Pts',(6.65095980993641,1.24780711915372,146.361793753362));
#45230=CARTESIAN_POINT('Ctrl Pts',(6.61873383884821,1.41957536382374,146.369991693987));
#45231=CARTESIAN_POINT('Ctrl Pts',(6.57985324873458,1.59007415442005,146.378189634613));
#45232=CARTESIAN_POINT('Ctrl Pts',(6.53445168184405,1.75875814643328,146.386387575238));
#45233=CARTESIAN_POINT('Ctrl Pts',(6.48903688873982,1.92749127883262,146.394587904056));
#45234=CARTESIAN_POINT('Ctrl Pts',(6.43709742815154,2.09440821331476,146.402788232875));
#45235=CARTESIAN_POINT('Ctrl Pts',(6.37881684499615,2.2589786758607,146.410988561693));
#45236=CARTESIAN_POINT('Ctrl Pts',(6.32047553195928,2.42372062510332,146.419197435467));
#45237=CARTESIAN_POINT('Ctrl Pts',(6.25578001523389,2.58611087894923,146.427406309242));
#45238=CARTESIAN_POINT('Ctrl Pts',(6.18496242640183,2.74563813784657,146.435615183016));
#45239=CARTESIAN_POINT('Ctrl Pts',(6.1141068305503,2.90525101326567,146.443828462402));
#45240=CARTESIAN_POINT('Ctrl Pts',(6.03712277050334,3.06199750896016,146.452041741788));
#45241=CARTESIAN_POINT('Ctrl Pts',(5.95428836567338,3.21539096509378,146.460255021174));
#45242=CARTESIAN_POINT('Ctrl Pts',(5.87133280250385,3.36900878327216,146.468480313773));
#45243=CARTESIAN_POINT('Ctrl Pts',(5.7825099763599,3.51926345212565,146.476705606371));
#45244=CARTESIAN_POINT('Ctrl Pts',(5.688142047697,3.66569625654136,146.48493089897));
#45245=CARTESIAN_POINT('Ctrl Pts',(5.60279758952673,3.79812714199456,146.492369688292));
#45246=CARTESIAN_POINT('Ctrl Pts',(5.51291844001722,3.92743235224374,146.499808477615));
#45247=CARTESIAN_POINT('Ctrl Pts',(5.41877068292729,4.0532965948531,146.507247266937));
#45248=CARTESIAN_POINT('Ctrl Pts',(5.31465068167149,4.19249253008954,146.515473981811));
#45249=CARTESIAN_POINT('Ctrl Pts',(5.20501825343316,4.32786854475823,146.523700696685));
#45250=CARTESIAN_POINT('Ctrl Pts',(5.09018299449507,4.45896020194767,146.531927411558));
#45251=CARTESIAN_POINT('Ctrl Pts',(4.97547307725163,4.58990877372399,146.540145147044));
#45252=CARTESIAN_POINT('Ctrl Pts',(4.85557187037958,4.71658203140227,146.548362882529));
#45253=CARTESIAN_POINT('Ctrl Pts',(4.73083148838794,4.8385454868666,146.556580618015));
#45254=CARTESIAN_POINT('Ctrl Pts',(4.60623003637546,4.96037310516212,146.564789200973));
#45255=CARTESIAN_POINT('Ctrl Pts',(4.47680040494159,5.07750112571033,146.57299778393));
#45256=CARTESIAN_POINT('Ctrl Pts',(4.34293390232146,5.18952927731089,146.581206366888));
#45257=CARTESIAN_POINT('Ctrl Pts',(4.20915413810584,5.30148484060192,146.589409631119));
#45258=CARTESIAN_POINT('Ctrl Pts',(4.07094350009997,5.4083468846326,146.597612895349));
#45259=CARTESIAN_POINT('Ctrl Pts',(3.92872934099403,5.50975269546761,146.60581615958));
#45260=CARTESIAN_POINT('Ctrl Pts',(3.78658379393986,5.61110958247685,146.614015466098));
#45261=CARTESIAN_POINT('Ctrl Pts',(3.64043886376392,5.70701527105099,146.622214772615));
#45262=CARTESIAN_POINT('Ctrl Pts',(3.49075412609444,5.79714797388808,146.630414079133));
#45263=CARTESIAN_POINT('Ctrl Pts',(3.36271593860724,5.87424620103042,146.637427648864));
#45264=CARTESIAN_POINT('Ctrl Pts',(3.23208837159504,5.94712101654775,146.644441218594));
#45265=CARTESIAN_POINT('Ctrl Pts',(3.09917575053262,6.01559628526637,146.651454788324));
#45266=CARTESIAN_POINT('Origin',(0.,0.,-3.69717978381041));
#45267=CARTESIAN_POINT('',(3.09917575053273,6.01559628526631,149.045786479356));
#45268=CARTESIAN_POINT('',(3.09917575053258,6.01559628526639,148.651204821489));
#45269=CARTESIAN_POINT('',(3.09917575053259,6.01559628526639,-3.69717978381041));
#45270=CARTESIAN_POINT('',(-6.767,3.61801146291416E-8,147.697179782109));
#45271=CARTESIAN_POINT('Ctrl Pts',(-6.76699999998963,1.18489098065876E-5,
147.697431498484));
#45272=CARTESIAN_POINT('Ctrl Pts',(-6.76700030221227,-0.172589739342158,
147.705556329219));
#45273=CARTESIAN_POINT('Ctrl Pts',(-6.76039261620527,-0.345365153995567,
147.713681159955));
#45274=CARTESIAN_POINT('Ctrl Pts',(-6.74716305906021,-0.517764091506218,
147.72180599069));
#45275=CARTESIAN_POINT('Ctrl Pts',(-6.73394247234798,-0.69004613220238,
147.729925312303));
#45276=CARTESIAN_POINT('Ctrl Pts',(-6.71410898296127,-0.861951839635234,
147.738044633917));
#45277=CARTESIAN_POINT('Ctrl Pts',(-6.68770077749777,-1.03293141624008,
147.74616395553));
#45278=CARTESIAN_POINT('Ctrl Pts',(-6.66130489176939,-1.20383122888302,
147.754279489385));
#45279=CARTESIAN_POINT('Ctrl Pts',(-6.62834045449182,-1.3738054093097,147.76239502324));
#45280=CARTESIAN_POINT('Ctrl Pts',(-6.58889743896392,-1.54230980636663,
147.770510557096));
#45281=CARTESIAN_POINT('Ctrl Pts',(-6.54945813819784,-1.7107983335999,147.778625326626));
#45282=CARTESIAN_POINT('Ctrl Pts',(-6.50354154946792,-1.87781699413692,
147.786740096157));
#45283=CARTESIAN_POINT('Ctrl Pts',(-6.45128870527251,-2.0428321128334,147.794854865687));
#45284=CARTESIAN_POINT('Ctrl Pts',(-6.39903587011488,-2.20784720298848,
147.802969633814));
#45285=CARTESIAN_POINT('Ctrl Pts',(-6.34044689170832,-2.37085840179826,
147.811084401941));
#45286=CARTESIAN_POINT('Ctrl Pts',(-6.27571253911645,-2.53134768974485,
147.819199170068));
#45287=CARTESIAN_POINT('Ctrl Pts',(-6.21096579408922,-2.69186770099439,
147.827315491647));
#45288=CARTESIAN_POINT('Ctrl Pts',(-6.14007146962038,-2.8498644996653,147.835431813226));
#45289=CARTESIAN_POINT('Ctrl Pts',(-6.06326826634064,-3.00484058319016,
147.843548134806));
#45290=CARTESIAN_POINT('Ctrl Pts',(-5.98643564276011,-3.15987603198623,
147.85166756543));
#45291=CARTESIAN_POINT('Ctrl Pts',(-5.90368979646056,-3.31188813315499,
147.859786996055));
#45292=CARTESIAN_POINT('Ctrl Pts',(-5.81531506766974,-3.46040455203338,
147.867906426679));
#45293=CARTESIAN_POINT('Ctrl Pts',(-5.72684077024805,-3.60908829902345,
147.876035005174));
#45294=CARTESIAN_POINT('Ctrl Pts',(-5.63272511365515,-3.75426818334733,
147.88416358367));
#45295=CARTESIAN_POINT('Ctrl Pts',(-5.53329587632421,-3.89550070530779,
147.892292162165));
#45296=CARTESIAN_POINT('Ctrl Pts',(-5.433803534497,-4.03682286294679,147.900425899604));
#45297=CARTESIAN_POINT('Ctrl Pts',(-5.32899111528955,-4.17419237636698,
147.908559637043));
#45298=CARTESIAN_POINT('Ctrl Pts',(-5.21922603288083,-4.30719962594016,
147.916693374482));
#45299=CARTESIAN_POINT('Ctrl Pts',(-5.10930377981723,-4.44039732621095,
147.924838758473));
#45300=CARTESIAN_POINT('Ctrl Pts',(-4.99441494525329,-4.56922001643452,
147.932984142465));
#45301=CARTESIAN_POINT('Ctrl Pts',(-4.87496369336073,-4.6932950033441,147.941129526457));
#45302=CARTESIAN_POINT('Ctrl Pts',(-4.81399306195092,-4.75662569410024,
147.945287115408));
#45303=CARTESIAN_POINT('Ctrl Pts',(-4.75183431668322,-4.818720103377,147.949444704359));
#45304=CARTESIAN_POINT('Ctrl Pts',(-4.6885443610219,-4.87953284390317,147.953602293311));
#45305=CARTESIAN_POINT('Ctrl Pts',(-4.5644196466217,-4.99879922623558,147.961756186543));
#45306=CARTESIAN_POINT('Ctrl Pts',(-4.43553781951026,-5.11352168817597,
147.969910079775));
#45307=CARTESIAN_POINT('Ctrl Pts',(-4.30226700957082,-5.22329279079381,
147.978063973008));
#45308=CARTESIAN_POINT('Ctrl Pts',(-4.16915882717726,-5.33292994206074,
147.986207916217));
#45309=CARTESIAN_POINT('Ctrl Pts',(-4.03167260190153,-5.43762753094104,
147.994351859426));
#45310=CARTESIAN_POINT('Ctrl Pts',(-3.89021417056718,-5.53701387998245,
148.002495802636));
#45311=CARTESIAN_POINT('Ctrl Pts',(-3.74889858379892,-5.63629986879952,
148.0106315221));
#45312=CARTESIAN_POINT('Ctrl Pts',(-3.60361907328117,-5.73028508639669,
148.018767241564));
#45313=CARTESIAN_POINT('Ctrl Pts',(-3.45481550655504,-5.81863719574153,
148.026902961029));
#45314=CARTESIAN_POINT('Ctrl Pts',(-3.30613090065821,-5.90691867210069,
148.035032176402));
#45315=CARTESIAN_POINT('Ctrl Pts',(-3.1539281610335,-5.98957582110507,148.043161391776));
#45316=CARTESIAN_POINT('Ctrl Pts',(-2.998677167291,-6.06631883817259,148.051290607149));
#45317=CARTESIAN_POINT('Ctrl Pts',(-2.84351764533614,-6.14301663929146,
148.059415032899));
#45318=CARTESIAN_POINT('Ctrl Pts',(-2.68531377287162,-6.21380708614292,
148.067539458649));
#45319=CARTESIAN_POINT('Ctrl Pts',(-2.52456112158583,-6.27844567893816,
148.075663884398));
#45320=CARTESIAN_POINT('Ctrl Pts',(-2.36283263342434,-6.34347665544801,
148.083837628863));
#45321=CARTESIAN_POINT('Ctrl Pts',(-2.19852464358827,-6.40228065315007,
148.092011373328));
#45322=CARTESIAN_POINT('Ctrl Pts',(-2.0321639654529,-6.45465712625503,148.100185117793));
#45323=CARTESIAN_POINT('Ctrl Pts',(-1.86686857706813,-6.50669820688264,
148.108306521727));
#45324=CARTESIAN_POINT('Ctrl Pts',(-1.69954707236529,-6.55239375033596,
148.116427925661));
#45325=CARTESIAN_POINT('Ctrl Pts',(-1.53073283787493,-6.59159661835062,
148.124549329596));
#45326=CARTESIAN_POINT('Ctrl Pts',(-1.36190555159674,-6.63080251731536,
148.132671361432));
#45327=CARTESIAN_POINT('Ctrl Pts',(-1.1915856621398,-6.66351465811254,148.140793393268));
#45328=CARTESIAN_POINT('Ctrl Pts',(-1.02031796570017,-6.68963678004041,
148.148915425105));
#45329=CARTESIAN_POINT('Ctrl Pts',(-0.849004414479253,-6.71576589583937,
148.157039631514));
#45330=CARTESIAN_POINT('Ctrl Pts',(-0.676742912638536,-6.73530142438346,
148.165163837922));
#45331=CARTESIAN_POINT('Ctrl Pts',(-0.504084569463769,-6.74819885205145,
148.173288044331));
#45332=CARTESIAN_POINT('Ctrl Pts',(-0.32955738407196,-6.76123588060333,
148.1815001866));
#45333=CARTESIAN_POINT('Ctrl Pts',(-0.154625098924222,-6.76749023865297,
148.189712328869));
#45334=CARTESIAN_POINT('Ctrl Pts',(0.0201426923150803,-6.76697002150492,
148.197924471137));
#45335=CARTESIAN_POINT('Ctrl Pts',(0.19331511027857,-6.76645455317546,148.206061648608));
#45336=CARTESIAN_POINT('Ctrl Pts',(0.366325662320664,-6.75928775695696,
148.214198826078));
#45337=CARTESIAN_POINT('Ctrl Pts',(0.538625371183535,-6.74552975751478,
148.222336003548));
#45338=CARTESIAN_POINT('Ctrl Pts',(0.713306080042034,-6.73158163705134,
148.230585628216));
#45339=CARTESIAN_POINT('Ctrl Pts',(0.887255765966873,-6.71085885889615,
148.238835252884));
#45340=CARTESIAN_POINT('Ctrl Pts',(1.05991347156252,-6.68347757030727,148.247084877552));
#45341=CARTESIAN_POINT('Ctrl Pts',(1.23257117715829,-6.65609628171836,148.255334502221));
#45342=CARTESIAN_POINT('Ctrl Pts',(1.40393653734784,-6.62205661971031,148.263584126889));
#45343=CARTESIAN_POINT('Ctrl Pts',(1.57346533802009,-6.58152686160661,148.271833751557));
#45344=CARTESIAN_POINT('Ctrl Pts',(1.74248533610249,-6.5411187444619,148.280058616831));
#45345=CARTESIAN_POINT('Ctrl Pts',(1.91018504262813,-6.49413881720199,148.288283482105));
#45346=CARTESIAN_POINT('Ctrl Pts',(2.07601559175624,-6.44068694028712,148.29650834738));
#45347=CARTESIAN_POINT('Ctrl Pts',(2.24165931412539,-6.38729528292152,148.304723946418));
#45348=CARTESIAN_POINT('Ctrl Pts',(2.40543773395594,-6.32744630395622,148.312939545457));
#45349=CARTESIAN_POINT('Ctrl Pts',(2.56681265041902,-6.26129074693461,148.321155144495));
#45350=CARTESIAN_POINT('Ctrl Pts',(2.72803818340686,-6.19519642958537,148.329363138419));
#45351=CARTESIAN_POINT('Ctrl Pts',(2.88686431410104,-6.12280729580259,148.337571132343));
#45352=CARTESIAN_POINT('Ctrl Pts',(3.04276839207491,-6.04432374316514,148.345779126267));
#45353=CARTESIAN_POINT('Ctrl Pts',(3.19855946508222,-5.96589707827147,148.353981170738));
#45354=CARTESIAN_POINT('Ctrl Pts',(3.35143238488852,-5.8813849539298,148.362183215208));
#45355=CARTESIAN_POINT('Ctrl Pts',(3.50088479236352,-5.79103571657073,148.370385259679));
#45356=CARTESIAN_POINT('Ctrl Pts',(3.65025888270915,-5.70073382467119,148.378583006054));
#45357=CARTESIAN_POINT('Ctrl Pts',(3.79621572525279,-5.60460109855421,148.38678075243));
#45358=CARTESIAN_POINT('Ctrl Pts',(3.93827780206285,-5.50293166900871,148.394978498806));
#45359=CARTESIAN_POINT('Ctrl Pts',(4.08031278365309,-5.40128163067305,148.403174681642));
#45360=CARTESIAN_POINT('Ctrl Pts',(4.21845418407797,-5.2940971958665,148.411370864478));
#45361=CARTESIAN_POINT('Ctrl Pts',(4.35225346470765,-5.18171581418166,148.419567047314));
#45362=CARTESIAN_POINT('Ctrl Pts',(4.4860428473285,-5.06934274608343,148.427762623824));
#45363=CARTESIAN_POINT('Ctrl Pts',(4.61549047452351,-4.95177372684966,148.435958200335));
#45364=CARTESIAN_POINT('Ctrl Pts',(4.74018095837061,-4.82938644984026,148.444153776845));
#45365=CARTESIAN_POINT('Ctrl Pts',(4.8648849040407,-4.70698595966649,148.452350238166));
#45366=CARTESIAN_POINT('Ctrl Pts',(4.98483042699659,-4.57976642674965,148.460546699486));
#45367=CARTESIAN_POINT('Ctrl Pts',(5.09963904573666,-4.44814237667794,148.468743160807));
#45368=CARTESIAN_POINT('Ctrl Pts',(5.21448094762456,-4.31648016864593,148.476941998291));
#45369=CARTESIAN_POINT('Ctrl Pts',(5.32418274320228,-4.18041117043751,148.485140835775));
#45370=CARTESIAN_POINT('Ctrl Pts',(5.42840625351473,-4.04038297031385,148.493339673259));
#45371=CARTESIAN_POINT('Ctrl Pts',(5.53273862871813,-3.90020850612087,148.501547074699));
#45372=CARTESIAN_POINT('Ctrl Pts',(5.63158107181388,-3.7560668660245,148.509754476139));
#45373=CARTESIAN_POINT('Ctrl Pts',(5.72463821485365,-3.6084354378369,148.517961877579));
#45374=CARTESIAN_POINT('Ctrl Pts',(5.81774520441193,-3.46072493014529,148.526173675354));
#45375=CARTESIAN_POINT('Ctrl Pts',(5.90506053685541,-3.30952121826683,148.534385473129));
#45376=CARTESIAN_POINT('Ctrl Pts',(5.98633491887672,-3.15532616999214,148.542597270904));
#45377=CARTESIAN_POINT('Ctrl Pts',(6.06772894864998,-3.00090412410236,148.550821157644));
#45378=CARTESIAN_POINT('Ctrl Pts',(6.14306410036819,-2.84348226485778,148.559045044384));
#45379=CARTESIAN_POINT('Ctrl Pts',(6.21213881171551,-2.68358349674047,148.567268931124));
#45380=CARTESIAN_POINT('Ctrl Pts',(6.27596290606529,-2.53583920851005,148.574867690684));
#45381=CARTESIAN_POINT('Ctrl Pts',(6.33444260790102,-2.38598066718417,148.582466450244));
#45382=CARTESIAN_POINT('Ctrl Pts',(6.38745708405515,-2.23443079985791,148.590065209804));
#45383=CARTESIAN_POINT('Ctrl Pts',(6.44483961693894,-2.07039418427202,148.598290058976));
#45384=CARTESIAN_POINT('Ctrl Pts',(6.49597967538635,-1.90391545841032,148.606514908149));
#45385=CARTESIAN_POINT('Ctrl Pts',(6.54066455293232,-1.73551035894767,148.614739757322));
#45386=CARTESIAN_POINT('Ctrl Pts',(6.58529910532507,-1.56729492124308,148.622955343477));
#45387=CARTESIAN_POINT('Ctrl Pts',(6.62349286201827,-1.39715777363023,148.631170929632));
#45388=CARTESIAN_POINT('Ctrl Pts',(6.65508168916922,-1.2256331875747,148.639386515787));
#45389=CARTESIAN_POINT('Ctrl Pts',(6.68664128706593,-1.05426731382947,148.647594500031));
#45390=CARTESIAN_POINT('Ctrl Pts',(6.71160806215666,-0.881516908974152,
148.655802484276));
#45391=CARTESIAN_POINT('Ctrl Pts',(6.72986806023965,-0.707930004849491,
148.66401046852));
#45392=CARTESIAN_POINT('Ctrl Pts',(6.74811482989324,-0.534468855508366,
148.672212506501));
#45393=CARTESIAN_POINT('Ctrl Pts',(6.75966446280209,-0.360172769293801,
148.680414544483));
#45394=CARTESIAN_POINT('Ctrl Pts',(6.76445431274541,-0.185598628173927,
148.688616582465));
#45395=CARTESIAN_POINT('Ctrl Pts',(6.7692416545327,-0.0111159010211107,
148.696814325533));
#45396=CARTESIAN_POINT('Ctrl Pts',(6.76727625517002,0.163644233189768,148.705012068601));
#45397=CARTESIAN_POINT('Ctrl Pts',(6.75854741509987,0.338121040231024,148.713209811669));
#45398=CARTESIAN_POINT('Ctrl Pts',(6.74982023470305,0.512564672818135,148.721405996045));
#45399=CARTESIAN_POINT('Ctrl Pts',(6.7343321867894,0.686724727267406,148.729602180421));
#45400=CARTESIAN_POINT('Ctrl Pts',(6.71212468128308,0.860041430926754,148.737798364797));
#45401=CARTESIAN_POINT('Ctrl Pts',(6.68991881060401,1.03334537570733,148.745993945803));
#45402=CARTESIAN_POINT('Ctrl Pts',(6.66099451217594,1.20580573731151,148.754189526809));
#45403=CARTESIAN_POINT('Ctrl Pts',(6.62544497345568,1.37686887673116,148.762385107815));
#45404=CARTESIAN_POINT('Ctrl Pts',(6.58989158393448,1.54795054607048,148.770581576583));
#45405=CARTESIAN_POINT('Ctrl Pts',(6.54771159734892,1.71763434029412,148.778778045352));
#45406=CARTESIAN_POINT('Ctrl Pts',(6.49904913891051,1.88537775791128,148.78697451412));
#45407=CARTESIAN_POINT('Ctrl Pts',(6.45037255566012,2.05316986489414,148.795173362003));
#45408=CARTESIAN_POINT('Ctrl Pts',(6.39520985258252,2.21902012888161,148.803372209887));
#45409=CARTESIAN_POINT('Ctrl Pts',(6.33375475728329,2.38240208079814,148.81157105777));
#45410=CARTESIAN_POINT('Ctrl Pts',(6.27223543567658,2.54595478209566,148.819778474214));
#45411=CARTESIAN_POINT('Ctrl Pts',(6.2044107100859,2.70703368127936,148.827985890659));
#45412=CARTESIAN_POINT('Ctrl Pts',(6.13052252148254,2.86513221572677,148.836193307103));
#45413=CARTESIAN_POINT('Ctrl Pts',(6.05659473155843,3.02331548510802,148.844405122417));
#45414=CARTESIAN_POINT('Ctrl Pts',(5.97659716433209,3.17851488671776,148.852616937731));
#45415=CARTESIAN_POINT('Ctrl Pts',(5.89081726300164,3.33024938614541,148.860828753045));
#45416=CARTESIAN_POINT('Ctrl Pts',(5.80491103808832,3.48220733704962,148.869052661471));
#45417=CARTESIAN_POINT('Ctrl Pts',(5.71320564995931,3.63068988310866,148.877276569897));
#45418=CARTESIAN_POINT('Ctrl Pts',(5.61603204282505,3.77524477272168,148.885500478323));
#45419=CARTESIAN_POINT('Ctrl Pts',(5.52624553783209,3.9088106523958,148.893099208232));
#45420=CARTESIAN_POINT('Ctrl Pts',(5.43179119289796,4.03902350447473,148.900697938142));
#45421=CARTESIAN_POINT('Ctrl Pts',(5.33295947919684,4.16555304770502,148.908296668051));
#45422=CARTESIAN_POINT('Ctrl Pts',(5.22693461647475,4.30129163756545,148.916448447124));
#45423=CARTESIAN_POINT('Ctrl Pts',(5.11555741577803,4.43319289296123,148.924600226197));
#45424=CARTESIAN_POINT('Ctrl Pts',(4.99913698328774,4.56080238799323,148.932752005271));
#45425=CARTESIAN_POINT('Ctrl Pts',(4.88284860610434,4.68826713600216,148.940894537808));
#45426=CARTESIAN_POINT('Ctrl Pts',(4.76152862715262,4.8114495455013,148.949037070345));
#45427=CARTESIAN_POINT('Ctrl Pts',(4.63552842812275,4.92992547530547,148.957179602883));
#45428=CARTESIAN_POINT('Ctrl Pts',(4.50967383726271,5.04826449212506,148.965312725759));
#45429=CARTESIAN_POINT('Ctrl Pts',(4.37915006662856,5.16190761644505,148.973445848634));
#45430=CARTESIAN_POINT('Ctrl Pts',(4.24434734603993,5.27046531211086,148.98157897151));
#45431=CARTESIAN_POINT('Ctrl Pts',(4.10963473767697,5.37895043968956,148.989706657598));
#45432=CARTESIAN_POINT('Ctrl Pts',(3.9706491556476,5.48235667595469,148.997834343685));
#45433=CARTESIAN_POINT('Ctrl Pts',(3.82781643569586,5.58033245735562,149.005962029773));
#45434=CARTESIAN_POINT('Ctrl Pts',(3.68505784274448,5.67825739150822,149.014085497773));
#45435=CARTESIAN_POINT('Ctrl Pts',(3.53845638861122,5.77075727651909,149.022208965772));
#45436=CARTESIAN_POINT('Ctrl Pts',(3.38846954371261,5.85752192922332,149.030332433772));
#45437=CARTESIAN_POINT('Ctrl Pts',(3.2933581315994,5.91254214546822,149.0354837823));
#45438=CARTESIAN_POINT('Ctrl Pts',(3.19688601129499,5.96525692464893,149.040635130828));
#45439=CARTESIAN_POINT('Ctrl Pts',(3.09917575053273,6.01559628526631,149.045786479356));
#45440=CARTESIAN_POINT('Ctrl Pts',(3.09917575053267,6.01559628526635,147.045751582743));
#45441=CARTESIAN_POINT('Ctrl Pts',(2.9338238445929,6.10078395293747,147.054501030655));
#45442=CARTESIAN_POINT('Ctrl Pts',(2.76495772123027,6.17915010267029,147.063250478567));
#45443=CARTESIAN_POINT('Ctrl Pts',(2.59315093316772,6.25042856433152,147.07199992648));
#45444=CARTESIAN_POINT('Ctrl Pts',(2.42134553245695,6.32170645041421,147.08074930374));
#45445=CARTESIAN_POINT('Ctrl Pts',(2.24659977927686,6.38589665313423,147.089498681));
#45446=CARTESIAN_POINT('Ctrl Pts',(2.06950718690031,6.44278115439039,147.09824805826));
#45447=CARTESIAN_POINT('Ctrl Pts',(1.89241596572979,6.49966521519689,147.106997367774));
#45448=CARTESIAN_POINT('Ctrl Pts',(1.71297821457321,6.54924360009514,147.115746677289));
#45449=CARTESIAN_POINT('Ctrl Pts',(1.53180337335973,6.59134792173526,147.124495986804));
#45450=CARTESIAN_POINT('Ctrl Pts',(1.35062987477911,6.63345193135279,147.13324523148));
#45451=CARTESIAN_POINT('Ctrl Pts',(1.1677195910308,6.66808192368215,147.141994476156));
#45452=CARTESIAN_POINT('Ctrl Pts',(0.98369374690812,6.6951202836315,147.150743720832));
#45453=CARTESIAN_POINT('Ctrl Pts',(0.79966920542126,6.7221584521885,147.159492903576));
#45454=CARTESIAN_POINT('Ctrl Pts',(0.614529402874977,6.74160505424565,147.16824208632));
#45455=CARTESIAN_POINT('Ctrl Pts',(0.428903127364861,6.75339404354112,147.176991269065));
#45456=CARTESIAN_POINT('Ctrl Pts',(0.243278104165756,6.76518295330323,147.185740392783));
#45457=CARTESIAN_POINT('Ctrl Pts',(0.0571669005412571,6.76931433552273,
147.194489516502));
#45458=CARTESIAN_POINT('Ctrl Pts',(-0.128798404775113,6.76577415902478,
147.20323864022));
#45459=CARTESIAN_POINT('Ctrl Pts',(-0.314762517256553,6.76223400523453,
147.21198770782));
#45460=CARTESIAN_POINT('Ctrl Pts',(-0.500580446816821,6.75102239665108,
147.220736775419));
#45461=CARTESIAN_POINT('Ctrl Pts',(-0.685621118839784,6.73217741012526,
147.229485843018));
#45462=CARTESIAN_POINT('Ctrl Pts',(-0.870660665411512,6.7133325382181,147.238234857404));
#45463=CARTESIAN_POINT('Ctrl Pts',(-1.05492267885174,6.68685441030661,147.246983871789));
#45464=CARTESIAN_POINT('Ctrl Pts',(-1.23778137634926,6.65283295028238,147.255732886175));
#45465=CARTESIAN_POINT('Ctrl Pts',(-1.42999922904426,6.61707018875721,147.264929696507));
#45466=CARTESIAN_POINT('Ctrl Pts',(-1.62066601086376,6.57297172968495,147.274126506839));
#45467=CARTESIAN_POINT('Ctrl Pts',(-1.8090662828219,6.52070304371829,147.283323317171));
#45468=CARTESIAN_POINT('Ctrl Pts',(-1.98831342328973,6.4709737498157,147.292073314909));
#45469=CARTESIAN_POINT('Ctrl Pts',(-2.16550875682036,6.41384934062005,147.300823312647));
#45470=CARTESIAN_POINT('Ctrl Pts',(-2.34005036501476,6.34952386318803,147.309573310384));
#45471=CARTESIAN_POINT('Ctrl Pts',(-2.51458843336683,6.28519969032774,147.318323130665));
#45472=CARTESIAN_POINT('Ctrl Pts',(-2.68647261510021,6.21367484061042,147.327072950946));
#45473=CARTESIAN_POINT('Ctrl Pts',(-2.85511905703302,6.13519226839444,147.335822771227));
#45474=CARTESIAN_POINT('Ctrl Pts',(-3.02376230286066,6.05671118354192,147.344572425685));
#45475=CARTESIAN_POINT('Ctrl Pts',(-3.18916767179931,5.97127276099435,147.353322080144));
#45476=CARTESIAN_POINT('Ctrl Pts',(-3.35077333905882,5.8791672055022,147.362071734602));
#45477=CARTESIAN_POINT('Ctrl Pts',(-3.51237615843546,5.7870632731328,147.370821234871));
#45478=CARTESIAN_POINT('Ctrl Pts',(-3.67017916111784,5.68829258485222,147.379570735139));
#45479=CARTESIAN_POINT('Ctrl Pts',(-3.82364636379465,5.58319061869107,147.388320235408));
#45480=CARTESIAN_POINT('Ctrl Pts',(-3.97711106595286,5.47809036500931,147.397069593116));
#45481=CARTESIAN_POINT('Ctrl Pts',(-4.12623987302113,5.36665920181476,147.405818950825));
#45482=CARTESIAN_POINT('Ctrl Pts',(-4.27052628038016,5.24927559655448,147.414568308533));
#45483=CARTESIAN_POINT('Ctrl Pts',(-4.41481052852976,5.13189374791003,147.42331753531));
#45484=CARTESIAN_POINT('Ctrl Pts',(-4.5542522996864,5.00855981630014,147.432066762086));
#45485=CARTESIAN_POINT('Ctrl Pts',(-4.68837800466957,4.87969268349254,147.440815988863));
#45486=CARTESIAN_POINT('Ctrl Pts',(-4.82250188069621,4.75082730793486,147.449565096333));
#45487=CARTESIAN_POINT('Ctrl Pts',(-4.95130962898196,4.61642908069523,147.458314203804));
#45488=CARTESIAN_POINT('Ctrl Pts',(-5.07436378883271,4.47695444901814,147.467063311275));
#45489=CARTESIAN_POINT('Ctrl Pts',(-5.19741643417376,4.33748153394847,147.475812311065));
#45490=CARTESIAN_POINT('Ctrl Pts',(-5.31471544322182,4.19293255432793,147.484561310855));
#45491=CARTESIAN_POINT('Ctrl Pts',(-5.42586245140029,4.04379841961546,147.493310310644));
#45492=CARTESIAN_POINT('Ctrl Pts',(-5.53702159888527,3.89464799670051,147.502060265986));
#45493=CARTESIAN_POINT('Ctrl Pts',(-5.64202722955755,3.74091164633121,147.510810221329));
#45494=CARTESIAN_POINT('Ctrl Pts',(-5.7405226511274,3.58311159355849,147.519560176671));
#45495=CARTESIAN_POINT('Ctrl Pts',(-5.83901426951965,3.42531763387737,147.528309794153));
#45496=CARTESIAN_POINT('Ctrl Pts',(-5.930996030062,3.26346052894687,147.537059411636));
#45497=CARTESIAN_POINT('Ctrl Pts',(-6.01615550518748,3.09809004669044,147.545809029118));
#45498=CARTESIAN_POINT('Ctrl Pts',(-6.1013121448033,2.93272507068684,147.554558355269));
#45499=CARTESIAN_POINT('Ctrl Pts',(-6.17964682235935,2.76384720624411,147.56330768142));
#45500=CARTESIAN_POINT('Ctrl Pts',(-6.25089348201509,2.59203003001534,147.572057007571));
#45501=CARTESIAN_POINT('Ctrl Pts',(-6.32213814808036,2.42021766149385,147.580806088903));
#45502=CARTESIAN_POINT('Ctrl Pts',(-6.38629508337152,2.24546641046453,147.589555170234));
#45503=CARTESIAN_POINT('Ctrl Pts',(-6.44314639750321,2.0683697687651,147.598304251566));
#45504=CARTESIAN_POINT('Ctrl Pts',(-6.50000285220132,1.89125711376742,147.607054124));
#45505=CARTESIAN_POINT('Ctrl Pts',(-6.54955227615689,1.71179891660476,147.615803996435));
#45506=CARTESIAN_POINT('Ctrl Pts',(-6.59162635874899,1.53060476500157,147.624553868869));
#45507=CARTESIAN_POINT('Ctrl Pts',(-6.63369752009797,1.34942319387872,147.633303133791));
#45508=CARTESIAN_POINT('Ctrl Pts',(-6.66829431385002,1.1665061886708,147.642052398714));
#45509=CARTESIAN_POINT('Ctrl Pts',(-6.69529923712354,0.982474999871755,
147.650801663636));
#45510=CARTESIAN_POINT('Ctrl Pts',(-6.72230554704547,0.798434361441817,
147.659551377816));
#45511=CARTESIAN_POINT('Ctrl Pts',(-6.74171916476026,0.613279708512756,
147.668301091996));
#45512=CARTESIAN_POINT('Ctrl Pts',(-6.75347414802849,0.427639955933567,
147.677050806175));
#45513=CARTESIAN_POINT('Ctrl Pts',(-6.76248837677719,0.285283377755817,
147.68376046482));
#45514=CARTESIAN_POINT('Ctrl Pts',(-6.76699999923736,0.142641725985062,
147.690470123464));
#45515=CARTESIAN_POINT('Ctrl Pts',(-6.767,3.61801116239577E-8,147.697179782109));
#45516=CARTESIAN_POINT('',(-6.76699988085942,0.00126982229687558,147.302820216159));
#45517=CARTESIAN_POINT('Ctrl Pts',(3.09917575053262,6.01559628526637,146.651454788324));
#45518=CARTESIAN_POINT('Ctrl Pts',(2.94383551293841,6.095626040357,146.659651824689));
#45519=CARTESIAN_POINT('Ctrl Pts',(2.78537370919825,6.16964506113875,146.667848861055));
#45520=CARTESIAN_POINT('Ctrl Pts',(2.62429879734114,6.23741491503282,146.67604589742));
#45521=CARTESIAN_POINT('Ctrl Pts',(2.46321043893686,6.30519042635998,146.684243618075));
#45522=CARTESIAN_POINT('Ctrl Pts',(2.29950886843622,6.36671559218961,146.69244133873));
#45523=CARTESIAN_POINT('Ctrl Pts',(2.13372239599045,6.42180019440412,146.700639059385));
#45524=CARTESIAN_POINT('Ctrl Pts',(1.96789195217928,6.47689940664764,146.708838954312));
#45525=CARTESIAN_POINT('Ctrl Pts',(1.79997584528955,6.52555453960363,146.717038849239));
#45526=CARTESIAN_POINT('Ctrl Pts',(1.6305174559355,6.56762528056296,146.725238744166));
#45527=CARTESIAN_POINT('Ctrl Pts',(1.45862578677847,6.61030012194282,146.733556382681));
#45528=CARTESIAN_POINT('Ctrl Pts',(1.28514757403759,6.64619993402496,146.741874021196));
#45529=CARTESIAN_POINT('Ctrl Pts',(1.11065980228004,6.675232116084,146.750191659711));
#45530=CARTESIAN_POINT('Ctrl Pts',(0.938374859555118,6.70389778000326,146.75840429181));
#45531=CARTESIAN_POINT('Ctrl Pts',(0.765106062686008,6.72586821508305,146.766616923908));
#45532=CARTESIAN_POINT('Ctrl Pts',(0.591412879740036,6.74110671964757,146.774829556007));
#45533=CARTESIAN_POINT('Ctrl Pts',(0.414388444682558,6.75663748266257,146.78319969773));
#45534=CARTESIAN_POINT('Ctrl Pts',(0.236923576271659,6.76517546696643,146.791569839453));
#45535=CARTESIAN_POINT('Ctrl Pts',(0.0596090533561449,6.76673745321614,
146.799939981176));
#45536=CARTESIAN_POINT('Ctrl Pts',(-0.117705469559497,6.76829943946584,
146.808310122899));
#45537=CARTESIAN_POINT('Ctrl Pts',(-0.294869260590996,6.76288549758536,
146.816680264622));
#45538=CARTESIAN_POINT('Ctrl Pts',(-0.471298878222098,6.75056785517979,
146.825050406345));
#45539=CARTESIAN_POINT('Ctrl Pts',(-0.643142130747061,6.73857041527806,
146.833202962572));
#45540=CARTESIAN_POINT('Ctrl Pts',(-0.814795756546637,6.71998823285555,
146.841355518798));
#45541=CARTESIAN_POINT('Ctrl Pts',(-0.985710125587109,6.69482371301254,
146.849508075025));
#45542=CARTESIAN_POINT('Ctrl Pts',(-1.15642648621514,6.66968834687178,146.857651186319));
#45543=CARTESIAN_POINT('Ctrl Pts',(-1.32640493695681,6.63798587589216,146.865794297613));
#45544=CARTESIAN_POINT('Ctrl Pts',(-1.49509738735121,6.5997706628591,146.873937408907));
#45545=CARTESIAN_POINT('Ctrl Pts',(-1.66362986896612,6.56159168879803,146.882072798198));
#45546=CARTESIAN_POINT('Ctrl Pts',(-1.83087842402008,6.5169123484129,146.890208187489));
#45547=CARTESIAN_POINT('Ctrl Pts',(-1.99630161783497,6.46583860381849,146.89834357678));
#45548=CARTESIAN_POINT('Ctrl Pts',(-2.16160270246582,6.41480255994268,146.906472960832));
#45549=CARTESIAN_POINT('Ctrl Pts',(-2.32508076097357,6.35738161781102,146.914602344885));
#45550=CARTESIAN_POINT('Ctrl Pts',(-2.48620607010074,6.29373246785993,146.922731728937));
#45551=CARTESIAN_POINT('Ctrl Pts',(-2.64724628660119,6.23011693195363,146.930856819744));
#45552=CARTESIAN_POINT('Ctrl Pts',(-2.80593588901788,6.16027987283074,146.93898191055));
#45553=CARTESIAN_POINT('Ctrl Pts',(-2.96176180886218,6.08442733439766,146.947107001356));
#45554=CARTESIAN_POINT('Ctrl Pts',(-3.11818254958853,6.0082852505933,146.955263107373));
#45555=CARTESIAN_POINT('Ctrl Pts',(-3.27171734868893,5.92608178937322,146.963419213389));
#45556=CARTESIAN_POINT('Ctrl Pts',(-3.42186849673354,5.83807373977604,146.971575319406));
#45557=CARTESIAN_POINT('Ctrl Pts',(-3.57141531398624,5.75041990641363,146.979698598594));
#45558=CARTESIAN_POINT('Ctrl Pts',(-3.71760535988774,5.65700832756984,146.987821877781));
#45559=CARTESIAN_POINT('Ctrl Pts',(-3.859972841208,5.55813805740165,146.995945156969));
#45560=CARTESIAN_POINT('Ctrl Pts',(-4.00235927996356,5.45925462182005,147.00406951784));
#45561=CARTESIAN_POINT('Ctrl Pts',(-4.14092183978618,5.35491125581414,147.012193878712));
#45562=CARTESIAN_POINT('Ctrl Pts',(-4.27522504620788,5.24544943777717,147.020318239583));
#45563=CARTESIAN_POINT('Ctrl Pts',(-4.40957168811507,5.13595221829794,147.028445227983));
#45564=CARTESIAN_POINT('Ctrl Pts',(-4.53965595009455,5.02133348140751,147.036572216383));
#45565=CARTESIAN_POINT('Ctrl Pts',(-4.66507671893109,4.90197390920098,147.044699204784));
#45566=CARTESIAN_POINT('Ctrl Pts',(-4.79130831812865,4.78184269154912,147.052878733198));
#45567=CARTESIAN_POINT('Ctrl Pts',(-4.91281564503122,4.65690938727829,147.061058261612));
#45568=CARTESIAN_POINT('Ctrl Pts',(-5.02922924669246,4.52759783817128,147.069237790026));
#45569=CARTESIAN_POINT('Ctrl Pts',(-5.14509461975249,4.39889525819394,147.077378798444));
#45570=CARTESIAN_POINT('Ctrl Pts',(-5.2559139558375,4.26585590360896,147.085519806863));
#45571=CARTESIAN_POINT('Ctrl Pts',(-5.36136533585237,4.12892852148359,147.093660815281));
#45572=CARTESIAN_POINT('Ctrl Pts',(-5.46756514649457,3.99102931095266,147.101859603693));
#45573=CARTESIAN_POINT('Ctrl Pts',(-5.56832030529724,3.84918698802021,147.110058392105));
#45574=CARTESIAN_POINT('Ctrl Pts',(-5.66334819405037,3.70388663878181,147.118257180517));
#45575=CARTESIAN_POINT('Ctrl Pts',(-5.75837608280357,3.55858628954329,147.126455968929));
#45576=CARTESIAN_POINT('Ctrl Pts',(-5.84767656591252,3.40982826574327,147.134654757341));
#45577=CARTESIAN_POINT('Ctrl Pts',(-5.93101572523069,3.25811931443068,147.142853545753));
#45578=CARTESIAN_POINT('Ctrl Pts',(-6.02009273654493,3.09596529124274,147.151616815914));
#45579=CARTESIAN_POINT('Ctrl Pts',(-6.10260743088169,2.92998977387308,147.160380086075));
#45580=CARTESIAN_POINT('Ctrl Pts',(-6.17823994314578,2.76073182415788,147.169143356237));
#45581=CARTESIAN_POINT('Ctrl Pts',(-6.253739347016,2.59177175763023,147.177891203602));
#45582=CARTESIAN_POINT('Ctrl Pts',(-6.32238060641745,2.41954103964781,147.186639050967));
#45583=CARTESIAN_POINT('Ctrl Pts',(-6.38388932885875,2.24460375943804,147.195386898333));
#45584=CARTESIAN_POINT('Ctrl Pts',(-6.44683896903127,2.06556835754892,147.204339674818));
#45585=CARTESIAN_POINT('Ctrl Pts',(-6.50231761661049,1.88369826451708,147.213292451304));
#45586=CARTESIAN_POINT('Ctrl Pts',(-6.5500813497716,1.69962446186629,147.222245227789));
#45587=CARTESIAN_POINT('Ctrl Pts',(-6.59655721135478,1.52051391068235,147.230956607181));
#45588=CARTESIAN_POINT('Ctrl Pts',(-6.63572867129488,1.33931724643213,147.239667986573));
#45589=CARTESIAN_POINT('Ctrl Pts',(-6.66741942644637,1.1566361536134,147.248379365964));
#45590=CARTESIAN_POINT('Ctrl Pts',(-6.70042743386985,0.966361771098127,
147.257452840997));
#45591=CARTESIAN_POINT('Ctrl Pts',(-6.725319414712,0.774477178504855,147.266526316029));
#45592=CARTESIAN_POINT('Ctrl Pts',(-6.74195345813885,0.581680813066479,
147.275599791062));
#45593=CARTESIAN_POINT('Ctrl Pts',(-6.7585875015657,0.388884447627976,147.284673266094));
#45594=CARTESIAN_POINT('Ctrl Pts',(-6.76696349439261,0.195176652538027,
147.293746741127));
#45595=CARTESIAN_POINT('Ctrl Pts',(-6.76699988085942,0.0012698222966961,
147.302820216159));
#45596=CARTESIAN_POINT('Ctrl Pts',(-6.76699988085954,0.00126982163972021,
147.30282021619));
#45597=CARTESIAN_POINT('Ctrl Pts',(-6.76703393944407,-0.180231603618993,
147.311313205573));
#45598=CARTESIAN_POINT('Ctrl Pts',(-6.75976143043599,-0.361630771729502,
147.319806194955));
#45599=CARTESIAN_POINT('Ctrl Pts',(-6.74523311582971,-0.542327588376448,
147.328299184338));
#45600=CARTESIAN_POINT('Ctrl Pts',(-6.73069223038859,-0.723180755563819,
147.336799522402));
#45601=CARTESIAN_POINT('Ctrl Pts',(-6.70888303755105,-0.903330040991249,
147.345299860467));
#45602=CARTESIAN_POINT('Ctrl Pts',(-6.67990792922329,-1.0821825433354,147.353800198532));
#45603=CARTESIAN_POINT('Ctrl Pts',(-6.64955444747541,-1.26954322906799,
147.362704905751));
#45604=CARTESIAN_POINT('Ctrl Pts',(-6.61133672238485,-1.45548034105547,
147.37160961297));
#45605=CARTESIAN_POINT('Ctrl Pts',(-6.56543161974002,-1.63932810825592,
147.380514320189));
#45606=CARTESIAN_POINT('Ctrl Pts',(-6.52149101612976,-1.8153081496402,147.38903795237));
#45607=CARTESIAN_POINT('Ctrl Pts',(-6.4705074268006,-1.98937366922607,147.397561584551));
#45608=CARTESIAN_POINT('Ctrl Pts',(-6.41268614305828,-2.16095937736654,
147.406085216732));
#45609=CARTESIAN_POINT('Ctrl Pts',(-6.35480723427398,-2.33271608886416,
147.414617343617));
#45610=CARTESIAN_POINT('Ctrl Pts',(-6.29007714417336,-2.50198775953929,
147.423149470501));
#45611=CARTESIAN_POINT('Ctrl Pts',(-6.21874885537241,-2.66823006388211,
147.431681597386));
#45612=CARTESIAN_POINT('Ctrl Pts',(-6.14730614356766,-2.83473904984793,
147.440227411289));
#45613=CARTESIAN_POINT('Ctrl Pts',(-6.0692442182562,-2.99820867128655,147.448773225192));
#45614=CARTESIAN_POINT('Ctrl Pts',(-5.98486208498972,-3.15811887421175,
147.457319039094));
#45615=CARTESIAN_POINT('Ctrl Pts',(-5.97387667941093,-3.17893700676326,
147.458431587783));
#45616=CARTESIAN_POINT('Ctrl Pts',(-5.96278421573265,-3.19969485310094,
147.459544136472));
#45617=CARTESIAN_POINT('Ctrl Pts',(-5.95158540696316,-3.22039130287348,
147.460656685161));
#45618=CARTESIAN_POINT('Ctrl Pts',(-5.86455592316925,-3.38122995787209,
147.469302652788));
#45619=CARTESIAN_POINT('Ctrl Pts',(-5.77092524741157,-3.53868192027616,
147.477948620414));
#45620=CARTESIAN_POINT('Ctrl Pts',(-5.67097279947118,-3.69220212172331,
147.486594588041));
#45621=CARTESIAN_POINT('Ctrl Pts',(-5.57114820444209,-3.84552594974385,
147.495229496288));
#45622=CARTESIAN_POINT('Ctrl Pts',(-5.46501812760932,-3.99492779111802,
147.503864404535));
#45623=CARTESIAN_POINT('Ctrl Pts',(-5.35290746851323,-4.13988775615177,
147.512499312781));
#45624=CARTESIAN_POINT('Ctrl Pts',(-5.2370748484061,-4.28966024608161,147.521420891288));
#45625=CARTESIAN_POINT('Ctrl Pts',(-5.11485785024722,-4.43469056379052,
147.530342469795));
#45626=CARTESIAN_POINT('Ctrl Pts',(-4.9866647519595,-4.57443588342483,147.539264048302));
#45627=CARTESIAN_POINT('Ctrl Pts',(-4.86293345640356,-4.70931732148341,
147.54787510835));
#45628=CARTESIAN_POINT('Ctrl Pts',(-4.73363525331509,-4.83927517159217,
147.556486168397));
#45629=CARTESIAN_POINT('Ctrl Pts',(-4.59917969044027,-4.96385285590153,
147.565097228445));
#45630=CARTESIAN_POINT('Ctrl Pts',(-4.46485092571184,-5.08831305738522,
147.573700167844));
#45631=CARTESIAN_POINT('Ctrl Pts',(-4.32537472098508,-5.20740300223337,
147.582303107243));
#45632=CARTESIAN_POINT('Ctrl Pts',(-4.18119829727038,-5.32070200245262,
147.590906046641));
#45633=CARTESIAN_POINT('Ctrl Pts',(-4.03718331838328,-5.43387413354107,
147.599499352703));
#45634=CARTESIAN_POINT('Ctrl Pts',(-3.8884788596687,-5.54126806845471,147.608092658764));
#45635=CARTESIAN_POINT('Ctrl Pts',(-3.73556628575502,-5.64250241690072,
147.616685964826));
#45636=CARTESIAN_POINT('Ctrl Pts',(-3.71852941001364,-5.65378152215081,
147.617643394839));
#45637=CARTESIAN_POINT('Ctrl Pts',(-3.70144033134603,-5.66498420615577,
147.618600824852));
#45638=CARTESIAN_POINT('Ctrl Pts',(-3.68429974104188,-5.67610997234539,
147.619558254864));
#45639=CARTESIAN_POINT('Ctrl Pts',(-3.53041242883121,-5.7759965121217,147.628154010825));
#45640=CARTESIAN_POINT('Ctrl Pts',(-3.37255098090347,-5.8695626523731,147.636749766786));
#45641=CARTESIAN_POINT('Ctrl Pts',(-3.21125769516597,-5.95651853142735,
147.645345522747));
#45642=CARTESIAN_POINT('Ctrl Pts',(-3.04981391785115,-6.04355554298091,
147.653949298812));
#45643=CARTESIAN_POINT('Ctrl Pts',(-2.8849321801368,-6.12396983774937,147.662553074876));
#45644=CARTESIAN_POINT('Ctrl Pts',(-2.71717694824763,-6.1975187318726,147.671156850941));
#45645=CARTESIAN_POINT('Ctrl Pts',(-2.54282874066887,-6.27395818306215,
147.68009876541));
#45646=CARTESIAN_POINT('Ctrl Pts',(-2.36537695821387,-6.34298154504423,
147.689040679879));
#45647=CARTESIAN_POINT('Ctrl Pts',(-2.18547384835621,-6.40437296369841,
147.697982594348));
#45648=CARTESIAN_POINT('Ctrl Pts',(-2.0119024912119,-6.46360368995572,147.706609795017));
#45649=CARTESIAN_POINT('Ctrl Pts',(-1.83604971473384,-6.51573049723694,
147.715236995687));
#45650=CARTESIAN_POINT('Ctrl Pts',(-1.65851332944963,-6.56061144528754,
147.723864196357));
#45651=CARTESIAN_POINT('Ctrl Pts',(-1.48080786809786,-6.6055351355298,147.732499613107));
#45652=CARTESIAN_POINT('Ctrl Pts',(-1.30141589509124,-6.64319912676801,
147.741135029856));
#45653=CARTESIAN_POINT('Ctrl Pts',(-1.12094415059955,-6.67351280895127,
147.749770446606));
#45654=CARTESIAN_POINT('Ctrl Pts',(-0.940205784786006,-6.7038712752864,
147.758418620955));
#45655=CARTESIAN_POINT('Ctrl Pts',(-0.758384761661105,-6.72685769002199,
147.767066795305));
#45656=CARTESIAN_POINT('Ctrl Pts',(-0.576093150510847,-6.74243321672039,
147.775714969654));
#45657=CARTESIAN_POINT('Ctrl Pts',(-0.556807229401932,-6.74408106204492,
147.776629921292));
#45658=CARTESIAN_POINT('Ctrl Pts',(-0.537516040892551,-6.74564600519852,
147.77754487293));
#45659=CARTESIAN_POINT('Ctrl Pts',(-0.518220309308166,-6.74712803428396,
147.778459824568));
#45660=CARTESIAN_POINT('Ctrl Pts',(-0.344739502314164,-6.76045241126372,
147.78668581734));
#45661=CARTESIAN_POINT('Ctrl Pts',(-0.170516782363119,-6.76709922487563,
147.794911810112));
#45662=CARTESIAN_POINT('Ctrl Pts',(0.00389331571225554,-6.76699888001267,
147.803137802884));
#45663=CARTESIAN_POINT('Ctrl Pts',(0.178120567359625,-6.76689864034833,
147.811355171766));
#45664=CARTESIAN_POINT('Ctrl Pts',(0.352534450596516,-6.76006532841609,
147.819572540649));
#45665=CARTESIAN_POINT('Ctrl Pts',(0.526575400606224,-6.74648110850956,
147.827789909531));
#45666=CARTESIAN_POINT('Ctrl Pts',(0.700468716025642,-6.73290841175744,
147.836000307825));
#45667=CARTESIAN_POINT('Ctrl Pts',(0.873989373075183,-6.71259624010123,
147.844210706118));
#45668=CARTESIAN_POINT('Ctrl Pts',(1.04657779932796,-6.68557880141681,147.852421104412));
#45669=CARTESIAN_POINT('Ctrl Pts',(1.21905434759662,-6.65857887640143,147.860626180432));
#45670=CARTESIAN_POINT('Ctrl Pts',(1.39059951608976,-6.62488239767228,147.868831256452));
#45671=CARTESIAN_POINT('Ctrl Pts',(1.56065875125951,-6.58457540484708,147.877036332472));
#45672=CARTESIAN_POINT('Ctrl Pts',(1.73064175957193,-6.5442864791112,147.885237730673));
#45673=CARTESIAN_POINT('Ctrl Pts',(1.89913981362772,-6.49739302505692,147.893439128874));
#45674=CARTESIAN_POINT('Ctrl Pts',(2.0656083602185,-6.4440322083456,147.901640527075));
#45675=CARTESIAN_POINT('Ctrl Pts',(2.23206386758617,-6.39067557130431,147.909841282872));
#45676=CARTESIAN_POINT('Ctrl Pts',(2.39648984055659,-6.33085268162535,147.91804203867));
#45677=CARTESIAN_POINT('Ctrl Pts',(2.55835634539918,-6.26475073805461,147.926242794468));
#45678=CARTESIAN_POINT('Ctrl Pts',(2.7202220280246,-6.19864913025533,147.93444350861));
#45679=CARTESIAN_POINT('Ctrl Pts',(2.87952793624065,-6.12626866659616,147.942644222751));
#45680=CARTESIAN_POINT('Ctrl Pts',(3.03576371935655,-6.04784487567584,147.950844936892));
#45681=CARTESIAN_POINT('Ctrl Pts',(3.19202702266656,-5.96940727077575,147.959047095551));
#45682=CARTESIAN_POINT('Ctrl Pts',(3.34521880315717,-5.88492437854656,147.967249254209));
#45683=CARTESIAN_POINT('Ctrl Pts',(3.49485289058715,-5.79467792661116,147.975451412867));
#45684=CARTESIAN_POINT('Ctrl Pts',(3.64454045305823,-5.70439922311592,147.983656502748));
#45685=CARTESIAN_POINT('Ctrl Pts',(3.79066748304104,-5.6083530417684,147.991861592629));
#45686=CARTESIAN_POINT('Ctrl Pts',(3.93277635253836,-5.50686473058083,148.000066682509));
#45687=CARTESIAN_POINT('Ctrl Pts',(4.075047564563,-5.40526048103565,148.008281145732));
#45688=CARTESIAN_POINT('Ctrl Pts',(4.21329115361369,-5.29820188968842,148.016495608954));
#45689=CARTESIAN_POINT('Ctrl Pts',(4.34708135694208,-5.18605559902,148.024710072177));
#45690=CARTESIAN_POINT('Ctrl Pts',(4.48095082671527,-5.07384286523736,148.032929402208));
#45691=CARTESIAN_POINT('Ctrl Pts',(4.61036138616766,-4.95653666375602,148.041148732239));
#45692=CARTESIAN_POINT('Ctrl Pts',(4.73492389474723,-4.8345407962858,148.04936806227));
#45693=CARTESIAN_POINT('Ctrl Pts',(4.85967940531258,-4.71235590368316,148.05760012765));
#45694=CARTESIAN_POINT('Ctrl Pts',(4.97957160763023,-4.58546708439416,148.06583219303));
#45695=CARTESIAN_POINT('Ctrl Pts',(5.094250563344,-4.45431253931169,148.07406425841));
#45696=CARTESIAN_POINT('Ctrl Pts',(5.19733220223208,-4.33642146356397,148.081463826932));
#45697=CARTESIAN_POINT('Ctrl Pts',(5.29620213894733,-4.21508438956819,148.088863395454));
#45698=CARTESIAN_POINT('Ctrl Pts',(5.39063649034132,-4.09063897563701,148.096262963976));
#45699=CARTESIAN_POINT('Ctrl Pts',(5.49471763035978,-3.9534810414655,148.104418423467));
#45700=CARTESIAN_POINT('Ctrl Pts',(5.59373040297787,-3.81212447922415,148.112573882958));
#45701=CARTESIAN_POINT('Ctrl Pts',(5.68731290183461,-3.66698254108546,148.12072934245));
#45702=CARTESIAN_POINT('Ctrl Pts',(5.78078149854195,-3.522017259682,148.12887487568));
#45703=CARTESIAN_POINT('Ctrl Pts',(5.86883278182236,-3.37327607722917,148.137020408909));
#45704=CARTESIAN_POINT('Ctrl Pts',(5.95114476016919,-3.22120552643119,148.145165942139));
#45705=CARTESIAN_POINT('Ctrl Pts',(6.03337386261268,-3.06928808802974,148.15330327403));
#45706=CARTESIAN_POINT('Ctrl Pts',(6.10987499165739,-2.91404827390774,148.161440605921));
#45707=CARTESIAN_POINT('Ctrl Pts',(6.18036919521648,-2.75596183043583,148.169577937812));
#45708=CARTESIAN_POINT('Ctrl Pts',(6.25080723617763,-2.59800133413285,148.177708786706));
#45709=CARTESIAN_POINT('Ctrl Pts',(6.3152477324257,-2.43719905642263,148.1858396356));
#45710=CARTESIAN_POINT('Ctrl Pts',(6.37345747199705,-2.27405559576826,148.193970484495));
#45711=CARTESIAN_POINT('Ctrl Pts',(6.43163306393536,-2.11100784011223,148.202096563581));
#45712=CARTESIAN_POINT('Ctrl Pts',(6.4835850558457,-1.94562198001445,148.210222642668));
#45713=CARTESIAN_POINT('Ctrl Pts',(6.52912822500949,-1.77841885431537,148.218348721755));
#45714=CARTESIAN_POINT('Ctrl Pts',(6.57483287196891,-1.61062289345233,148.226503612656));
#45715=CARTESIAN_POINT('Ctrl Pts',(6.61408302073444,-1.44099709884985,148.234658503557));
#45716=CARTESIAN_POINT('Ctrl Pts',(6.64674171189912,-1.27008409772752,148.242813394458));
#45717=CARTESIAN_POINT('Ctrl Pts',(6.67927305267028,-1.09983756048281,148.250936485905));
#45718=CARTESIAN_POINT('Ctrl Pts',(6.70526419716062,-0.928314202450003,
148.259059577352));
#45719=CARTESIAN_POINT('Ctrl Pts',(6.72463089436373,-0.756061065370284,
148.267182668798));
#45720=CARTESIAN_POINT('Ctrl Pts',(6.74399911232347,-0.583794402231071,
148.275306398105));
#45721=CARTESIAN_POINT('Ctrl Pts',(6.7567418059398,-0.410798209435841,148.283430127412));
#45722=CARTESIAN_POINT('Ctrl Pts',(6.76282658223518,-0.237624953683721,
148.291553856719));
#45723=CARTESIAN_POINT('Ctrl Pts',(6.7689129939542,-0.0644051536344399,
148.299679769465));
#45724=CARTESIAN_POINT('Ctrl Pts',(6.76833791234505,0.108991438684712,148.307805682211));
#45725=CARTESIAN_POINT('Ctrl Pts',(6.76112107417796,0.282012092483061,148.315931594957));
#45726=CARTESIAN_POINT('Ctrl Pts',(6.75385808633422,0.456139165331137,148.324109470659));
#45727=CARTESIAN_POINT('Ctrl Pts',(6.73986811838416,0.629885099653434,148.332287346361));
#45728=CARTESIAN_POINT('Ctrl Pts',(6.71922421894785,0.802692279459984,148.340465222064));
#45729=CARTESIAN_POINT('Ctrl Pts',(6.69867884061792,0.97467475293634,148.348604069608));
#45730=CARTESIAN_POINT('Ctrl Pts',(6.67154302027316,1.14572706080913,148.356742917153));
#45731=CARTESIAN_POINT('Ctrl Pts',(6.6379399531208,1.31531067765859,148.364881764697));
#45732=CARTESIAN_POINT('Ctrl Pts',(6.60409518114556,1.48611409917312,148.373079154478));
#45733=CARTESIAN_POINT('Ctrl Pts',(6.56368986228207,1.65542725416067,148.381276544259));
#45734=CARTESIAN_POINT('Ctrl Pts',(6.51690055096956,1.82271671105869,148.38947393404));
#45735=CARTESIAN_POINT('Ctrl Pts',(6.47011123965706,1.99000616795671,148.397671323821));
#45736=CARTESIAN_POINT('Ctrl Pts',(6.416938108077,2.15527159113971,148.405868713602));
#45737=CARTESIAN_POINT('Ctrl Pts',(6.35760628504209,2.31800157989449,148.414066103384));
#45738=CARTESIAN_POINT('Ctrl Pts',(6.29805504077451,2.48133337747458,148.422293808791));
#45739=CARTESIAN_POINT('Ctrl Pts',(6.23212231044813,2.64259718578998,148.430521514198));
#45740=CARTESIAN_POINT('Ctrl Pts',(6.15997062115693,2.80125881461952,148.438749219605));
#45741=CARTESIAN_POINT('Ctrl Pts',(6.08790258433046,2.95973649160482,148.446967385834));
#45742=CARTESIAN_POINT('Ctrl Pts',(6.00963009503864,3.11561767361745,148.455185552063));
#45743=CARTESIAN_POINT('Ctrl Pts',(5.92536500898667,3.26838469435231,148.463403718292));
#45744=CARTESIAN_POINT('Ctrl Pts',(5.84119797321572,3.42097395642084,148.471612321918));
#45745=CARTESIAN_POINT('Ctrl Pts',(5.75105241082793,3.57045596734108,148.479820925545));
#45746=CARTESIAN_POINT('Ctrl Pts',(5.65518754507125,3.71633459608672,148.488029529171));
#45747=CARTESIAN_POINT('Ctrl Pts',(5.55938678915395,3.86211566817921,148.496232643276));
#45748=CARTESIAN_POINT('Ctrl Pts',(5.45787454183872,4.00429785801297,148.504435757381));
#45749=CARTESIAN_POINT('Ctrl Pts',(5.3509553530199,4.14241062788175,148.512638871486));
#45750=CARTESIAN_POINT('Ctrl Pts',(5.24408823251829,4.28045613854671,148.520837990776));
#45751=CARTESIAN_POINT('Ctrl Pts',(5.13181963362406,4.41443589324564,148.529037110066));
#45752=CARTESIAN_POINT('Ctrl Pts',(5.01449675683676,4.54390925037832,148.537236229356));
#45753=CARTESIAN_POINT('Ctrl Pts',(4.89720969107976,4.67334308773068,148.545432845989));
#45754=CARTESIAN_POINT('Ctrl Pts',(4.77487166154099,4.79827300251162,148.553629462623));
#45755=CARTESIAN_POINT('Ctrl Pts',(4.64786942653458,4.9182922639759,148.561826079256));
#45756=CARTESIAN_POINT('Ctrl Pts',(4.52085719900817,5.03832096854069,148.570023340798));
#45757=CARTESIAN_POINT('Ctrl Pts',(4.38918028835731,5.153437996135,148.57822060234));
#45758=CARTESIAN_POINT('Ctrl Pts',(4.25326179248185,5.26327399292627,148.586417863882));
#45759=CARTESIAN_POINT('Ctrl Pts',(4.11733958182613,5.3731129916386,148.594615349463));
#45760=CARTESIAN_POINT('Ctrl Pts',(3.97717583715614,5.47767045050518,148.602812835043));
#45761=CARTESIAN_POINT('Ctrl Pts',(3.83322589023906,5.57661799609772,148.611010320624));
#45762=CARTESIAN_POINT('Ctrl Pts',(3.68919908197937,5.67561837422939,148.619212183211));
#45763=CARTESIAN_POINT('Ctrl Pts',(3.54138233098872,5.76900265545213,148.627414045797));
#45764=CARTESIAN_POINT('Ctrl Pts',(3.39025952851201,5.85648609059507,148.635615908384));
#45765=CARTESIAN_POINT('Ctrl Pts',(3.29451541302883,5.91191137374175,148.640812212752));
#45766=CARTESIAN_POINT('Ctrl Pts',(3.19744483268801,5.96496902539041,148.646008517121));
#45767=CARTESIAN_POINT('Ctrl Pts',(3.09917575053258,6.01559628526639,148.651204821489));
#45768=CARTESIAN_POINT('Origin',(0.,0.,-3.69717978381041));
#45769=CARTESIAN_POINT('',(3.09917575053262,6.01559628526637,151.045614412788));
#45770=CARTESIAN_POINT('',(3.09917575053255,6.01559628526641,150.651392015123));
#45771=CARTESIAN_POINT('',(3.09917575053259,6.01559628526639,-3.69717978381041));
#45772=CARTESIAN_POINT('',(-6.76699997627813,0.000566614310235722,149.697179783767));
#45773=CARTESIAN_POINT('Ctrl Pts',(-6.76699997627821,0.000566613400196833,
149.69717978381));
#45774=CARTESIAN_POINT('Ctrl Pts',(-6.76700396482936,-0.0470682034863547,
149.699411627096));
#45775=CARTESIAN_POINT('Ctrl Pts',(-6.76650495248852,-0.094704481331748,
149.701643470382));
#45776=CARTESIAN_POINT('Ctrl Pts',(-6.76550302050593,-0.142330177844389,
149.703875313668));
#45777=CARTESIAN_POINT('Ctrl Pts',(-6.76164443078019,-0.325743849067885,
149.712470475538));
#45778=CARTESIAN_POINT('Ctrl Pts',(-6.75032524002114,-0.508892452664186,
149.721065637408));
#45779=CARTESIAN_POINT('Ctrl Pts',(-6.73161054280729,-0.691164596869533,
149.729660799278));
#45780=CARTESIAN_POINT('Ctrl Pts',(-6.7128783227168,-0.873607405460162,
149.738264008939));
#45781=CARTESIAN_POINT('Ctrl Pts',(-6.68673680573006,-1.05517181285975,
149.746867218599));
#45782=CARTESIAN_POINT('Ctrl Pts',(-6.65330256622685,-1.23525461433637,
149.75547042826));
#45783=CARTESIAN_POINT('Ctrl Pts',(-6.61848155058639,-1.42280684043653,
149.764430479471));
#45784=CARTESIAN_POINT('Ctrl Pts',(-6.57575002775779,-1.60875156095252,
149.773390530682));
#45785=CARTESIAN_POINT('Ctrl Pts',(-6.52529734598111,-1.79242393047288,
149.782350581893));
#45786=CARTESIAN_POINT('Ctrl Pts',(-6.47672146268755,-1.96926383812271,
149.790977326529));
#45787=CARTESIAN_POINT('Ctrl Pts',(-6.42098863317139,-2.14399713628271,
149.799604071166));
#45788=CARTESIAN_POINT('Ctrl Pts',(-6.35831760155604,-2.316049714005,149.808230815803));
#45789=CARTESIAN_POINT('Ctrl Pts',(-6.29558667263248,-2.48826672952273,
149.816865805378));
#45790=CARTESIAN_POINT('Ctrl Pts',(-6.22590441835218,-2.65779762737199,
149.825500794953));
#45791=CARTESIAN_POINT('Ctrl Pts',(-6.14953704952157,-2.82408977841738,
149.834135784528));
#45792=CARTESIAN_POINT('Ctrl Pts',(-6.07305625398113,-2.99062891939909,
149.842783599456));
#45793=CARTESIAN_POINT('Ctrl Pts',(-5.98987063636119,-3.15391942696104,
149.851431414384));
#45794=CARTESIAN_POINT('Ctrl Pts',(-5.90029221948735,-3.31343337410866,
149.860079229312));
#45795=CARTESIAN_POINT('Ctrl Pts',(-5.89023820993247,-3.33133673526112,
149.861049833805));
#45796=CARTESIAN_POINT('Ctrl Pts',(-5.88010371402478,-3.34919255304436,
149.862020438298));
#45797=CARTESIAN_POINT('Ctrl Pts',(-5.86988920644516,-3.36700010455281,
149.862991042791));
#45798=CARTESIAN_POINT('Ctrl Pts',(-5.78333435411803,-3.51789626661514,
149.871215671137));
#45799=CARTESIAN_POINT('Ctrl Pts',(-5.69084309843223,-3.66565158696293,
149.879440299483));
#45800=CARTESIAN_POINT('Ctrl Pts',(-5.59266957079819,-3.80976850633578,
149.887664927829));
#45801=CARTESIAN_POINT('Ctrl Pts',(-5.49459923989674,-3.95373393481747,
149.895880910721));
#45802=CARTESIAN_POINT('Ctrl Pts',(-5.39085873155815,-4.09406828460298,
149.904096893612));
#45803=CARTESIAN_POINT('Ctrl Pts',(-5.28174781080178,-4.23029893306497,
149.912312876503));
#45804=CARTESIAN_POINT('Ctrl Pts',(-5.17272972786479,-4.3664136686903,149.920521868766));
#45805=CARTESIAN_POINT('Ctrl Pts',(-5.05835055591938,-4.49843137887082,
149.928730861029));
#45806=CARTESIAN_POINT('Ctrl Pts',(-4.9389531043467,-4.62590869268559,149.936939853291));
#45807=CARTESIAN_POINT('Ctrl Pts',(-4.81963333329541,-4.7533030691841,149.945143504747));
#45808=CARTESIAN_POINT('Ctrl Pts',(-4.69530203017841,-4.87616267276169,
149.953347156202));
#45809=CARTESIAN_POINT('Ctrl Pts',(-4.56634204662254,-4.99407742363363,
149.961550807657));
#45810=CARTESIAN_POINT('Ctrl Pts',(-4.43744014567412,-5.1119390665879,149.969750764249));
#45811=CARTESIAN_POINT('Ctrl Pts',(-4.30391398159691,-5.22486005251954,
149.977950720842));
#45812=CARTESIAN_POINT('Ctrl Pts',(-4.16618306273024,-5.33246731708875,
149.986150677434));
#45813=CARTESIAN_POINT('Ctrl Pts',(-4.02846316007205,-5.44006597484643,
149.994349978164));
#45814=CARTESIAN_POINT('Ctrl Pts',(-3.88653944934674,-5.54235153041358,
150.002549278895));
#45815=CARTESIAN_POINT('Ctrl Pts',(-3.74086459358734,-5.63899114136959,
150.010748579625));
#45816=CARTESIAN_POINT('Ctrl Pts',(-3.59519068936305,-5.7356301210843,150.018947826799));
#45817=CARTESIAN_POINT('Ctrl Pts',(-3.44576598706677,-5.82662303054573,
150.027147073972));
#45818=CARTESIAN_POINT('Ctrl Pts',(-3.29307210356225,-5.91168039737773,
150.035346321146));
#45819=CARTESIAN_POINT('Ctrl Pts',(-3.14035151623339,-5.996752639442,150.043547002242));
#45820=CARTESIAN_POINT('Ctrl Pts',(-2.98436092183173,-6.07588709629209,
150.051747683339));
#45821=CARTESIAN_POINT('Ctrl Pts',(-2.82560654218276,-6.14884027022771,
150.059948364435));
#45822=CARTESIAN_POINT('Ctrl Pts',(-2.66679559782668,-6.22181943761892,
150.068151967461));
#45823=CARTESIAN_POINT('Ctrl Pts',(-2.50521923212617,-6.28861278517178,
150.076355570487));
#45824=CARTESIAN_POINT('Ctrl Pts',(-2.34140368498817,-6.34902494749578,
150.084559173513));
#45825=CARTESIAN_POINT('Ctrl Pts',(-2.1774004699578,-6.40950631828855,150.092772174627));
#45826=CARTESIAN_POINT('Ctrl Pts',(-2.01115328531376,-6.46359177480447,
150.100985175741));
#45827=CARTESIAN_POINT('Ctrl Pts',(-1.84320460156978,-6.51113552283717,
150.109198176854));
#45828=CARTESIAN_POINT('Ctrl Pts',(-1.67515653678631,-6.5587074041484,150.117416037885));
#45829=CARTESIAN_POINT('Ctrl Pts',(-1.50540531381688,-6.59972977664111,
150.125633898915));
#45830=CARTESIAN_POINT('Ctrl Pts',(-1.3345035309375,-6.63410802790514,150.133851759945));
#45831=CARTESIAN_POINT('Ctrl Pts',(-1.16333518430878,-6.66853990058492,
150.14208243877));
#45832=CARTESIAN_POINT('Ctrl Pts',(-0.991013045163549,-6.69630688502552,
150.150313117594));
#45833=CARTESIAN_POINT('Ctrl Pts',(-0.818096122069102,-6.71736613078783,
150.158543796418));
#45834=CARTESIAN_POINT('Ctrl Pts',(-0.659278447110338,-6.73670825409481,
150.166103364625));
#45835=CARTESIAN_POINT('Ctrl Pts',(-0.499959279506673,-6.75039250432336,
150.173662932831));
#45836=CARTESIAN_POINT('Ctrl Pts',(-0.340570660280462,-6.75842441885356,
150.181222501038));
#45837=CARTESIAN_POINT('Ctrl Pts',(-0.168647099917588,-6.76708799439156,
150.1893765831));
#45838=CARTESIAN_POINT('Ctrl Pts',(0.00388881049175518,-6.7692012821825,
150.197530665162));
#45839=CARTESIAN_POINT('Ctrl Pts',(0.176491945955157,-6.76469804152506,
150.205684747223));
#45840=CARTESIAN_POINT('Ctrl Pts',(0.348884466162331,-6.76020029584998,
150.213828879442));
#45841=CARTESIAN_POINT('Ctrl Pts',(0.521343686668807,-6.74910210203667,
150.221973011661));
#45842=CARTESIAN_POINT('Ctrl Pts',(0.693319462283189,-6.73138894458041,
150.23011714388));
#45843=CARTESIAN_POINT('Ctrl Pts',(0.865121581854534,-6.71369367334575,
150.238253052396));
#45844=CARTESIAN_POINT('Ctrl Pts',(1.03644086740629,-6.68939677341782,150.246388960911));
#45845=CARTESIAN_POINT('Ctrl Pts',(1.20672727565984,-6.65853574610654,150.254524869427));
#45846=CARTESIAN_POINT('Ctrl Pts',(1.37687754983429,-6.62769939039164,150.262654273756));
#45847=CARTESIAN_POINT('Ctrl Pts',(1.54599623272606,-6.59030942079538,150.270783678086));
#45848=CARTESIAN_POINT('Ctrl Pts',(1.71353850991623,-6.54645513045297,150.278913082416));
#45849=CARTESIAN_POINT('Ctrl Pts',(1.88098207103713,-6.5026266791002,150.287037696893));
#45850=CARTESIAN_POINT('Ctrl Pts',(2.0468507233365,-6.45234158439991,150.29516231137));
#45851=CARTESIAN_POINT('Ctrl Pts',(2.21060996053383,-6.3957401919081,150.303286925847));
#45852=CARTESIAN_POINT('Ctrl Pts',(2.37535707894493,-6.33879735026647,150.31146055224));
#45853=CARTESIAN_POINT('Ctrl Pts',(2.53796888007013,-6.27546182363841,150.319634178634));
#45854=CARTESIAN_POINT('Ctrl Pts',(2.69791614876294,-6.2059276062684,150.327807805027));
#45855=CARTESIAN_POINT('Ctrl Pts',(2.85684515792853,-6.13683605903512,150.335929396315));
#45856=CARTESIAN_POINT('Ctrl Pts',(3.01314313174157,-6.06162468484079,150.344050987603));
#45857=CARTESIAN_POINT('Ctrl Pts',(3.16631085115103,-5.98053213300316,150.352172578891));
#45858=CARTESIAN_POINT('Ctrl Pts',(3.31949039946434,-5.89943331851433,150.360294797397));
#45859=CARTESIAN_POINT('Ctrl Pts',(3.46953888837857,-5.81245259286801,150.368417015903));
#45860=CARTESIAN_POINT('Ctrl Pts',(3.61598184378114,-5.71987450084747,150.376539234409));
#45861=CARTESIAN_POINT('Ctrl Pts',(3.76246399203482,-5.62727163194801,150.384663626682));
#45862=CARTESIAN_POINT('Ctrl Pts',(3.90533837616407,-5.52906860929183,150.392788018955));
#45863=CARTESIAN_POINT('Ctrl Pts',(4.04415968501874,-5.4255931880366,150.400912411228));
#45864=CARTESIAN_POINT('Ctrl Pts',(4.18447445378208,-5.32100456309202,150.4091242069));
#45865=CARTESIAN_POINT('Ctrl Pts',(4.32064812564791,-5.21102966677564,150.417336002571));
#45866=CARTESIAN_POINT('Ctrl Pts',(4.45225600858948,-5.096048021161,150.425547798243));
#45867=CARTESIAN_POINT('Ctrl Pts',(4.58267093414513,-4.98210862469067,150.433685158234));
#45868=CARTESIAN_POINT('Ctrl Pts',(4.7086022792593,-4.86325316794276,150.441822518225));
#45869=CARTESIAN_POINT('Ctrl Pts',(4.82967494894583,-4.73988701210536,150.449959878216));
#45870=CARTESIAN_POINT('Ctrl Pts',(4.95240886869547,-4.61482813705478,150.458208891727));
#45871=CARTESIAN_POINT('Ctrl Pts',(5.07014954707028,-4.48513416966097,150.466457905239));
#45872=CARTESIAN_POINT('Ctrl Pts',(5.18254967333258,-4.35126049363175,150.47470691875));
#45873=CARTESIAN_POINT('Ctrl Pts',(5.29494979959488,-4.21738681760252,150.482955932262));
#45874=CARTESIAN_POINT('Ctrl Pts',(5.40200918801733,-4.07933377557342,150.491204945774));
#45875=CARTESIAN_POINT('Ctrl Pts',(5.50342733123436,-3.93758512413671,150.499453959285));
#45876=CARTESIAN_POINT('Ctrl Pts',(5.60454655662779,-3.79625425986352,150.507678659818));
#45877=CARTESIAN_POINT('Ctrl Pts',(5.70036008965199,-3.65082725855684,150.515903360351));
#45878=CARTESIAN_POINT('Ctrl Pts',(5.79051899991666,-3.50173938373548,150.524128060883));
#45879=CARTESIAN_POINT('Ctrl Pts',(5.88057634176751,-3.35281946368334,150.532343495889));
#45880=CARTESIAN_POINT('Ctrl Pts',(5.96499156158994,-3.20024718656367,150.540558930896));
#45881=CARTESIAN_POINT('Ctrl Pts',(6.04345714430163,-3.04448924205516,150.548774365902));
#45882=CARTESIAN_POINT('Ctrl Pts',(6.12185009874917,-2.8888754681339,150.556982196647));
#45883=CARTESIAN_POINT('Ctrl Pts',(6.19430422302675,-2.73008221757033,150.565190027391));
#45884=CARTESIAN_POINT('Ctrl Pts',(6.26055630029154,-2.56860347482438,150.573397858136));
#45885=CARTESIAN_POINT('Ctrl Pts',(6.32676036273262,-2.40724176045984,150.581599740426));
#45886=CARTESIAN_POINT('Ctrl Pts',(6.38677119532312,-2.24319876107158,150.589801622715));
#45887=CARTESIAN_POINT('Ctrl Pts',(6.4403723410656,-2.07699135974064,150.598003505004));
#45888=CARTESIAN_POINT('Ctrl Pts',(6.49394540526051,-1.91087103417984,150.606201090341));
#45889=CARTESIAN_POINT('Ctrl Pts',(6.54111536246229,-1.74258890629774,150.614398675679));
#45890=CARTESIAN_POINT('Ctrl Pts',(6.58171453172264,-1.57268014005107,150.622596261016));
#45891=CARTESIAN_POINT('Ctrl Pts',(6.62230596857683,-1.40280373416089,150.630792285064));
#45892=CARTESIAN_POINT('Ctrl Pts',(6.6563290208704,-1.23130165416054,150.638988309111));
#45893=CARTESIAN_POINT('Ctrl Pts',(6.68366629150933,-1.05872277001204,150.647184333159));
#45894=CARTESIAN_POINT('Ctrl Pts',(6.71100154442281,-0.886156623667957,
150.65537975227));
#45895=CARTESIAN_POINT('Ctrl Pts',(6.73165194140962,-0.712514185737677,
150.66357517138));
#45896=CARTESIAN_POINT('Ctrl Pts',(6.74555150261371,-0.538352974902165,
150.671770590491));
#45897=CARTESIAN_POINT('Ctrl Pts',(6.7594525670483,-0.364172928619752,150.679966895932));
#45898=CARTESIAN_POINT('Ctrl Pts',(6.76660131256587,-0.189474355435032,
150.688163201373));
#45899=CARTESIAN_POINT('Ctrl Pts',(6.76698377532349,-0.0148183841432244,
150.696359506814));
#45900=CARTESIAN_POINT('Ctrl Pts',(6.76736634903676,0.159888256305075,150.704558190072));
#45901=CARTESIAN_POINT('Ctrl Pts',(6.7609787292514,0.334551911487722,150.71275687333));
#45902=CARTESIAN_POINT('Ctrl Pts',(6.74785906062422,0.508612915635836,150.720955556588));
#45903=CARTESIAN_POINT('Ctrl Pts',(6.73472568236196,0.682855807979336,150.729162807208));
#45904=CARTESIAN_POINT('Ctrl Pts',(6.71484622770233,0.856494432818047,150.737370057828));
#45905=CARTESIAN_POINT('Ctrl Pts',(6.68831070415793,1.02897469582418,150.745577308449));
#45906=CARTESIAN_POINT('Ctrl Pts',(6.66176096118246,1.20154738478935,150.753788957039));
#45907=CARTESIAN_POINT('Ctrl Pts',(6.62854810712325,1.37296012253397,150.762000605629));
#45908=CARTESIAN_POINT('Ctrl Pts',(6.58881298834815,1.5426705431085,150.770212254219));
#45909=CARTESIAN_POINT('Ctrl Pts',(6.54901935243595,1.71263089292084,150.778435995945));
#45910=CARTESIAN_POINT('Ctrl Pts',(6.50268435133856,1.88088356948477,150.78665973767));
#45911=CARTESIAN_POINT('Ctrl Pts',(6.4499986631602,2.0469016207995,150.794883479395));
#45912=CARTESIAN_POINT('Ctrl Pts',(6.4013048591865,2.20034083221205,150.802484125441));
#45913=CARTESIAN_POINT('Ctrl Pts',(6.3471868848032,2.35187120945674,150.810084771486));
#45914=CARTESIAN_POINT('Ctrl Pts',(6.28783096916308,2.50109390132272,150.817685417532));
#45915=CARTESIAN_POINT('Ctrl Pts',(6.22358991167221,2.66259799781795,150.825911615954));
#45916=CARTESIAN_POINT('Ctrl Pts',(6.15303221576947,2.82185231328987,150.834137814376));
#45917=CARTESIAN_POINT('Ctrl Pts',(6.07633550844756,2.97832768324431,150.842364012798));
#45918=CARTESIAN_POINT('Ctrl Pts',(5.99737722358098,3.13941708677773,150.850832779464));
#45919=CARTESIAN_POINT('Ctrl Pts',(5.91191238708636,3.29756077071774,150.859301546131));
#45920=CARTESIAN_POINT('Ctrl Pts',(5.82018977794054,3.45219929157581,150.867770312797));
#45921=CARTESIAN_POINT('Ctrl Pts',(5.73130494264953,3.60205350510196,150.875977067241));
#45922=CARTESIAN_POINT('Ctrl Pts',(5.6365439549662,3.7486158563877,150.884183821685));
#45923=CARTESIAN_POINT('Ctrl Pts',(5.53618142010418,3.89139875670603,150.89239057613));
#45924=CARTESIAN_POINT('Ctrl Pts',(5.43588628825688,4.0340857646882,150.900591818955));
#45925=CARTESIAN_POINT('Ctrl Pts',(5.32999730572402,4.17299808375075,150.908793061781));
#45926=CARTESIAN_POINT('Ctrl Pts',(5.21883357252479,4.30767514354183,150.916994304607));
#45927=CARTESIAN_POINT('Ctrl Pts',(5.1077242642446,4.44228626646785,150.925191532167));
#45928=CARTESIAN_POINT('Ctrl Pts',(4.99134557668544,4.57266598397942,150.933388759727));
#45929=CARTESIAN_POINT('Ctrl Pts',(4.87005829085282,4.69838496120696,150.941585987286));
#45930=CARTESIAN_POINT('Ctrl Pts',(4.74880831326354,4.82406526699287,150.94978069336));
#45931=CARTESIAN_POINT('Ctrl Pts',(4.62265299463237,4.94508743108714,150.957975399434));
#45932=CARTESIAN_POINT('Ctrl Pts',(4.49199157550546,5.0610572695424,150.966170105508));
#45933=CARTESIAN_POINT('Ctrl Pts',(4.36132600684613,5.17703079095632,150.974365071829));
#45934=CARTESIAN_POINT('Ctrl Pts',(4.22615431604807,5.28795142348739,150.98256003815));
#45935=CARTESIAN_POINT('Ctrl Pts',(4.08691081441889,5.3934635434928,150.99075500447));
#45936=CARTESIAN_POINT('Ctrl Pts',(3.94766332851582,5.49897868259197,150.998950205279));
#45937=CARTESIAN_POINT('Ctrl Pts',(3.80434408879023,5.59908478839752,151.007145406088));
#45938=CARTESIAN_POINT('Ctrl Pts',(3.65741831470865,5.69346821113755,151.015340606898));
#45939=CARTESIAN_POINT('Ctrl Pts',(3.51043154852579,5.7878908145,151.023539209714));
#45940=CARTESIAN_POINT('Ctrl Pts',(3.35983556333475,5.87658580209414,151.03173781253));
#45941=CARTESIAN_POINT('Ctrl Pts',(3.2061225495812,5.95928411783387,151.039936415346));
#45942=CARTESIAN_POINT('Ctrl Pts',(3.17063755624633,5.97837520915509,151.04182908116));
#45943=CARTESIAN_POINT('Ctrl Pts',(3.13498654744956,5.9971469166337,151.043721746974));
#45944=CARTESIAN_POINT('Ctrl Pts',(3.09917575053262,6.01559628526637,151.045614412788));
#45945=CARTESIAN_POINT('Ctrl Pts',(3.09917575053273,6.01559628526631,149.045786479356));
#45946=CARTESIAN_POINT('Ctrl Pts',(2.94512620286167,6.09496108966518,149.053908071751));
#45947=CARTESIAN_POINT('Ctrl Pts',(2.78799803146464,6.16841903677227,149.062029664145));
#45948=CARTESIAN_POINT('Ctrl Pts',(2.6282914520702,6.23573356093529,149.070151256539));
#45949=CARTESIAN_POINT('Ctrl Pts',(2.4685751060542,6.30305220161929,149.078273345598));
#45950=CARTESIAN_POINT('Ctrl Pts',(2.30628037506223,6.36422652839151,149.086395434656));
#45951=CARTESIAN_POINT('Ctrl Pts',(2.14192748660438,6.41906812879632,149.094517523714));
#45952=CARTESIAN_POINT('Ctrl Pts',(1.97753325073724,6.47392352608732,149.102641656104));
#45953=CARTESIAN_POINT('Ctrl Pts',(1.81108017339957,6.52244290859249,149.110765788493));
#45954=CARTESIAN_POINT('Ctrl Pts',(1.64310362371349,6.56448775471016,149.118889920882));
#45955=CARTESIAN_POINT('Ctrl Pts',(1.47505282556408,6.60655118535775,149.127017644275));
#45956=CARTESIAN_POINT('Ctrl Pts',(1.30547756869858,6.64213429208963,149.135145367667));
#45957=CARTESIAN_POINT('Ctrl Pts',(1.13492334272837,6.67114967648982,149.14327309106));
#45958=CARTESIAN_POINT('Ctrl Pts',(0.964166382420434,6.700199550887,149.151410475712));
#45959=CARTESIAN_POINT('Ctrl Pts',(0.792428489986612,6.72266605231141,149.159547860364));
#45960=CARTESIAN_POINT('Ctrl Pts',(0.620261075322537,6.73851357485015,149.167685245016));
#45961=CARTESIAN_POINT('Ctrl Pts',(0.447975890638217,6.75437193778545,149.175828195994));
#45962=CARTESIAN_POINT('Ctrl Pts',(0.275260962282223,6.76360228215639,149.183971146972));
#45963=CARTESIAN_POINT('Ctrl Pts',(0.102667306064882,6.76622113326674,149.19211409795));
#45964=CARTESIAN_POINT('Ctrl Pts',(-0.070176194071899,6.76884377538563,
149.200268836538));
#45965=CARTESIAN_POINT('Ctrl Pts',(-0.24289770757871,6.76483582292493,149.208423575127));
#45966=CARTESIAN_POINT('Ctrl Pts',(-0.414950837277496,6.75426567456764,
149.216578313715));
#45967=CARTESIAN_POINT('Ctrl Pts',(-0.484926364438568,6.7499667018912,149.21989491791));
#45968=CARTESIAN_POINT('Ctrl Pts',(-0.554791444068832,6.74458285327622,
149.223211522104));
#45969=CARTESIAN_POINT('Ctrl Pts',(-0.624509858585915,6.7381211354894,149.226528126298));
#45970=CARTESIAN_POINT('Ctrl Pts',(-0.797549664132813,6.72208327236423,
149.234759876099));
#45971=CARTESIAN_POINT('Ctrl Pts',(-0.97022531043997,6.69935190517954,149.2429916259));
#45972=CARTESIAN_POINT('Ctrl Pts',(-1.14197910143897,6.66994548192687,149.251223375702));
#45973=CARTESIAN_POINT('Ctrl Pts',(-1.31352780205097,6.6405741727447,149.25944529601));
#45974=CARTESIAN_POINT('Ctrl Pts',(-1.48415648957198,6.60454373877506,149.267667216317));
#45975=CARTESIAN_POINT('Ctrl Pts',(-1.65331051605781,6.56192451476643,149.275889136625));
#45976=CARTESIAN_POINT('Ctrl Pts',(-1.8222964485577,6.51934764289916,149.284102886537));
#45977=CARTESIAN_POINT('Ctrl Pts',(-1.98981029334086,6.47019510725002,149.292316636449));
#45978=CARTESIAN_POINT('Ctrl Pts',(-2.1553054588549,6.41458863677401,149.300530386361));
#45979=CARTESIAN_POINT('Ctrl Pts',(-2.32066931320966,6.35902628692279,149.308737619122));
#45980=CARTESIAN_POINT('Ctrl Pts',(-2.48401734042951,6.29702031544894,149.316944851883));
#45981=CARTESIAN_POINT('Ctrl Pts',(-2.6448159412813,6.22874286166513,149.325152084644));
#45982=CARTESIAN_POINT('Ctrl Pts',(-2.8055191552641,6.16050591055053,149.333354448816));
#45983=CARTESIAN_POINT('Ctrl Pts',(-2.96367562670376,6.08600502804842,149.341556812988));
#45984=CARTESIAN_POINT('Ctrl Pts',(-3.11876956394421,6.00546129843622,149.34975917716));
#45985=CARTESIAN_POINT('Ctrl Pts',(-3.27381721439687,5.92494160658195,149.357959093389));
#45986=CARTESIAN_POINT('Ctrl Pts',(-3.4258038319085,5.83838282150255,149.366159009619));
#45987=CARTESIAN_POINT('Ctrl Pts',(-3.57423594106801,5.74605311823496,149.374358925848));
#45988=CARTESIAN_POINT('Ctrl Pts',(-3.72264729859076,5.65373632317486,149.382557695683));
#45989=CARTESIAN_POINT('Ctrl Pts',(-3.86750483280932,5.55565040534534,149.390756465519));
#45990=CARTESIAN_POINT('Ctrl Pts',(-4.00834189494613,5.45210823931621,149.398955235354));
#45991=CARTESIAN_POINT('Ctrl Pts',(-4.14918481625368,5.34856176567642,149.407154346278));
#45992=CARTESIAN_POINT('Ctrl Pts',(-4.28600664340828,5.23955880387085,149.415353457203));
#45993=CARTESIAN_POINT('Ctrl Pts',(-4.41837177039249,5.12545411632948,149.423552568127));
#45994=CARTESIAN_POINT('Ctrl Pts',(-4.55076641610839,5.01132398231489,149.431753507535));
#45995=CARTESIAN_POINT('Ctrl Pts',(-4.67870211068835,4.89209009050625,149.439954446942));
#45996=CARTESIAN_POINT('Ctrl Pts',(-4.80177820549031,4.76814587290262,149.448155386349));
#45997=CARTESIAN_POINT('Ctrl Pts',(-4.9249696591013,4.64408548280138,149.456364012469));
#45998=CARTESIAN_POINT('Ctrl Pts',(-5.04329215966144,4.51530620073256,149.464572638589));
#45999=CARTESIAN_POINT('Ctrl Pts',(-5.15638302138738,4.38223722962917,149.472781264709));
#46000=CARTESIAN_POINT('Ctrl Pts',(-5.26952787890707,4.24910472408447,149.480993810079));
#46001=CARTESIAN_POINT('Ctrl Pts',(-5.37743589602003,4.11167872763715,149.489206355448));
#46002=CARTESIAN_POINT('Ctrl Pts',(-5.4797863068807,3.97041950314104,149.497418900818));
#46003=CARTESIAN_POINT('Ctrl Pts',(-5.58227716442797,3.82896644073198,149.505642715558));
#46004=CARTESIAN_POINT('Ctrl Pts',(-5.67919497535735,3.68366993616677,149.513866530299));
#46005=CARTESIAN_POINT('Ctrl Pts',(-5.77026307927509,3.53501810404909,149.52209034504));
#46006=CARTESIAN_POINT('Ctrl Pts',(-5.8539405746149,3.39843007317805,149.529646758208));
#46007=CARTESIAN_POINT('Ctrl Pts',(-5.9326797234281,3.25900969930774,149.537203171376));
#46008=CARTESIAN_POINT('Ctrl Pts',(-6.0063013658658,3.11715140832116,149.544759584544));
#46009=CARTESIAN_POINT('Ctrl Pts',(-6.09117194522075,2.95361803764797,149.553470571453));
#46010=CARTESIAN_POINT('Ctrl Pts',(-6.16943201730198,2.78647759071529,149.562181558361));
#46011=CARTESIAN_POINT('Ctrl Pts',(-6.24078436680482,2.61627588129475,149.570892545269));
#46012=CARTESIAN_POINT('Ctrl Pts',(-6.31203988881782,2.44630514120322,149.579591711081));
#46013=CARTESIAN_POINT('Ctrl Pts',(-6.37640626983225,2.27328169467997,149.588290876892));
#46014=CARTESIAN_POINT('Ctrl Pts',(-6.43363275134785,2.09777468303541,149.596990042704));
#46015=CARTESIAN_POINT('Ctrl Pts',(-6.49075166015386,1.92259758447119,149.605672856072));
#46016=CARTESIAN_POINT('Ctrl Pts',(-6.54075736032535,1.74494651626455,149.61435566944));
#46017=CARTESIAN_POINT('Ctrl Pts',(-6.5834477071965,1.56540898381516,149.623038482807));
#46018=CARTESIAN_POINT('Ctrl Pts',(-6.62608942416789,1.38607596814402,149.631711405313));
#46019=CARTESIAN_POINT('Ctrl Pts',(-6.66143233574533,1.20486105875168,149.640384327818));
#46020=CARTESIAN_POINT('Ctrl Pts',(-6.68932389964516,1.02236723619061,149.649057250324));
#46021=CARTESIAN_POINT('Ctrl Pts',(-6.71717092613002,0.840164820849831,
149.657716323855));
#46022=CARTESIAN_POINT('Ctrl Pts',(-6.73759030209038,0.656687857839354,
149.666375397386));
#46023=CARTESIAN_POINT('Ctrl Pts',(-6.75048041214476,0.472549685482899,
149.675034470918));
#46024=CARTESIAN_POINT('Ctrl Pts',(-6.7614690981279,0.315573791173186,149.682416241867));
#46025=CARTESIAN_POINT('Ctrl Pts',(-6.76698678421464,0.158117688653368,
149.689798012817));
#46026=CARTESIAN_POINT('Ctrl Pts',(-6.76699997627813,0.000566614310398829,
149.697179783767));
#46027=CARTESIAN_POINT('',(-6.767,9.01944948036252E-12,149.30282021619));
#46028=CARTESIAN_POINT('Ctrl Pts',(3.09917575053258,6.01559628526639,148.651204821489));
#46029=CARTESIAN_POINT('Ctrl Pts',(2.94388516761211,6.09560045875987,148.659416327252));
#46030=CARTESIAN_POINT('Ctrl Pts',(2.78560087384593,6.16953292422705,148.667627833014));
#46031=CARTESIAN_POINT('Ctrl Pts',(2.62484376789698,6.23718559882039,148.675839338777));
#46032=CARTESIAN_POINT('Ctrl Pts',(2.46398377506222,6.30488157210938,148.684056100022));
#46033=CARTESIAN_POINT('Ctrl Pts',(2.30064815032346,6.36628961790689,148.692272861268));
#46034=CARTESIAN_POINT('Ctrl Pts',(2.13537375161274,6.4212512753297,148.700489622514));
#46035=CARTESIAN_POINT('Ctrl Pts',(1.96988497674041,6.47628422309903,148.708717041658));
#46036=CARTESIAN_POINT('Ctrl Pts',(1.80245274945248,6.52485398647728,148.716944460801));
#46037=CARTESIAN_POINT('Ctrl Pts',(1.6336257460409,6.56685281713184,148.725171879945));
#46038=CARTESIAN_POINT('Ctrl Pts',(1.5878156857973,6.57824891445967,148.727404334227));
#46039=CARTESIAN_POINT('Ctrl Pts',(1.54190297044554,6.58916150686769,148.729636788509));
#46040=CARTESIAN_POINT('Ctrl Pts',(1.49589863188773,6.59958909956646,148.731869242791));
#46041=CARTESIAN_POINT('Ctrl Pts',(1.32638072773533,6.63801294642667,148.740095444554));
#46042=CARTESIAN_POINT('Ctrl Pts',(1.1551444957387,6.66995491392575,148.748321646317));
#46043=CARTESIAN_POINT('Ctrl Pts',(0.982726700329653,6.69526229751002,148.75654784808));
#46044=CARTESIAN_POINT('Ctrl Pts',(0.810502580265703,6.72054125353996,148.764764809425));
#46045=CARTESIAN_POINT('Ctrl Pts',(0.637099891296366,6.73920041413438,148.77298177077));
#46046=CARTESIAN_POINT('Ctrl Pts',(0.463068282913116,6.75113744233962,148.781198732115));
#46047=CARTESIAN_POINT('Ctrl Pts',(0.289197233144874,6.76306345764476,148.789408112631));
#46048=CARTESIAN_POINT('Ctrl Pts',(0.114698775060923,6.76827966714148,148.797617493147));
#46049=CARTESIAN_POINT('Ctrl Pts',(-0.0598694812759922,6.7667351540615,
148.805826873663));
#46050=CARTESIAN_POINT('Ctrl Pts',(-0.234311709875384,6.76519175602669,
148.814030327502));
#46051=CARTESIAN_POINT('Ctrl Pts',(-0.40882327918961,6.75689736035804,148.822233781341));
#46052=CARTESIAN_POINT('Ctrl Pts',(-0.582843623452481,6.74185303240888,
148.83043723518));
#46053=CARTESIAN_POINT('Ctrl Pts',(-0.75677324356916,6.72681654770249,148.838636412212));
#46054=CARTESIAN_POINT('Ctrl Pts',(-0.930211792370118,6.70503717205541,
148.846835589244));
#46055=CARTESIAN_POINT('Ctrl Pts',(-1.10260078454534,6.67656801881925,148.855034766277));
#46056=CARTESIAN_POINT('Ctrl Pts',(-1.27495733857424,6.64810422257571,148.863232400484));
#46057=CARTESIAN_POINT('Ctrl Pts',(-1.44626437487053,6.61295320838439,148.871430034691));
#46058=CARTESIAN_POINT('Ctrl Pts',(-1.61597028789769,6.57121975196629,148.879627668898));
#46059=CARTESIAN_POINT('Ctrl Pts',(-1.78566397759705,6.52948930146418,148.887824712658));
#46060=CARTESIAN_POINT('Ctrl Pts',(-1.95375642518749,6.48117743774689,148.896021756418));
#46061=CARTESIAN_POINT('Ctrl Pts',(-2.11970800408929,6.42643968130098,148.904218800178));
#46062=CARTESIAN_POINT('Ctrl Pts',(-2.28567779148569,6.37169591893364,148.912416743332));
#46063=CARTESIAN_POINT('Ctrl Pts',(-2.44950590150521,6.31052497153085,148.920614686485));
#46064=CARTESIAN_POINT('Ctrl Pts',(-2.61066956059549,6.24313170174875,148.928812629639));
#46065=CARTESIAN_POINT('Ctrl Pts',(-2.77188019416391,6.17571878880579,148.937012962253));
#46066=CARTESIAN_POINT('Ctrl Pts',(-2.93042449906161,6.10208007930452,148.945213294867));
#46067=CARTESIAN_POINT('Ctrl Pts',(-3.08580126436238,6.0224678958762,148.95341362748));
#46068=CARTESIAN_POINT('Ctrl Pts',(-3.24133997366222,5.94277273533523,148.961622507026));
#46069=CARTESIAN_POINT('Ctrl Pts',(-3.39370422798857,5.85709182613359,148.969831386572));
#46070=CARTESIAN_POINT('Ctrl Pts',(-3.54241807360485,5.76572312826394,148.978040266118));
#46071=CARTESIAN_POINT('Ctrl Pts',(-3.69121175197275,5.67430538173623,148.986253552364));
#46072=CARTESIAN_POINT('Ctrl Pts',(-3.83635081725048,5.57719395889699,148.994466838611));
#46073=CARTESIAN_POINT('Ctrl Pts',(-3.97738984309682,5.47472912900997,149.002680124858));
#46074=CARTESIAN_POINT('Ctrl Pts',(-4.11863519109865,5.37211440610975,149.010905426097));
#46075=CARTESIAN_POINT('Ctrl Pts',(-4.25576823160249,5.26413084759802,149.019130727337));
#46076=CARTESIAN_POINT('Ctrl Pts',(-4.38837708282492,5.1511586637316,149.027356028577));
#46077=CARTESIAN_POINT('Ctrl Pts',(-4.50830565974434,5.04898906405793,149.034794813117));
#46078=CARTESIAN_POINT('Ctrl Pts',(-4.62453422653369,4.94273989356865,149.042233597658));
#46079=CARTESIAN_POINT('Ctrl Pts',(-4.73678561079548,4.83271673878792,149.049672382199));
#46080=CARTESIAN_POINT('Ctrl Pts',(-4.85803307738912,4.71387607707551,149.057707327923));
#46081=CARTESIAN_POINT('Ctrl Pts',(-4.97502002374452,4.59025882254214,149.065742273648));
#46082=CARTESIAN_POINT('Ctrl Pts',(-5.08733491019311,4.46220937558184,149.073777219373));
#46083=CARTESIAN_POINT('Ctrl Pts',(-5.19951770846345,4.33431052146556,149.081802715582));
#46084=CARTESIAN_POINT('Ctrl Pts',(-5.30703913411327,4.20199012627802,149.08982821179));
#46085=CARTESIAN_POINT('Ctrl Pts',(-5.4095220371579,4.06563160277749,149.097853707999));
#46086=CARTESIAN_POINT('Ctrl Pts',(-5.51190724024873,3.92940307385215,149.105871553267));
#46087=CARTESIAN_POINT('Ctrl Pts',(-5.60926325531765,3.7891443765773,149.113889398535));
#46088=CARTESIAN_POINT('Ctrl Pts',(-5.70125112887812,3.64527427849619,149.121907243803));
#46089=CARTESIAN_POINT('Ctrl Pts',(-5.79316596150943,3.50151841727303,149.129918722679));
#46090=CARTESIAN_POINT('Ctrl Pts',(-5.87972093833214,3.35415718109323,149.137930201555));
#46091=CARTESIAN_POINT('Ctrl Pts',(-5.9606187667796,3.20364057239804,149.14594168043));
#46092=CARTESIAN_POINT('Ctrl Pts',(-6.04148158251528,3.053189107536,149.153949691925));
#46093=CARTESIAN_POINT('Ctrl Pts',(-6.11669194310629,2.89958531797667,149.16195770342));
#46094=CARTESIAN_POINT('Ctrl Pts',(-6.1859970691669,2.74330626439312,149.169965714915));
#46095=CARTESIAN_POINT('Ctrl Pts',(-6.25528612372444,2.58706345112009,149.177971869393));
#46096=CARTESIAN_POINT('Ctrl Pts',(-6.31867251662192,2.42814695248479,149.185978023871));
#46097=CARTESIAN_POINT('Ctrl Pts',(-6.37595052568969,2.26705621764379,149.193984178349));
#46098=CARTESIAN_POINT('Ctrl Pts',(-6.43322675806054,2.10597047964916,149.201990084485));
#46099=CARTESIAN_POINT('Ctrl Pts',(-6.48439485906697,1.94271099495298,149.209995990622));
#46100=CARTESIAN_POINT('Ctrl Pts',(-6.52929820438422,1.77779468955923,149.218001896758));
#46101=CARTESIAN_POINT('Ctrl Pts',(-6.57422542585116,1.61279069434266,149.226012059821));
#46102=CARTESIAN_POINT('Ctrl Pts',(-6.61288113874827,1.44612848236859,149.234022222883));
#46103=CARTESIAN_POINT('Ctrl Pts',(-6.64515922493019,1.27833793471255,149.242032385946));
#46104=CARTESIAN_POINT('Ctrl Pts',(-6.67744680380719,1.11049804136435,149.250044904725));
#46105=CARTESIAN_POINT('Ctrl Pts',(-6.70335296096843,0.941529523093904,
149.258057423504));
#46106=CARTESIAN_POINT('Ctrl Pts',(-6.72282324652257,0.771969297327177,
149.266069942284));
#46107=CARTESIAN_POINT('Ctrl Pts',(-6.74231191257035,0.602249001969103,
149.274090025105));
#46108=CARTESIAN_POINT('Ctrl Pts',(-6.75535254533619,0.431936258650848,
149.282110107926));
#46109=CARTESIAN_POINT('Ctrl Pts',(-6.7619427611625,0.261570439388989,149.290130190747));
#46110=CARTESIAN_POINT('Ctrl Pts',(-6.76531612817425,0.174364428269627,
149.294235470988));
#46111=CARTESIAN_POINT('Ctrl Pts',(-6.76700022446772,0.0871444901626732,
149.29834075123));
#46112=CARTESIAN_POINT('Ctrl Pts',(-6.76699999997756,-1.74287689782069E-5,
149.302446031472));
#46113=CARTESIAN_POINT('Ctrl Pts',(-6.767,9.01944950864228E-12,149.30282021619));
#46114=CARTESIAN_POINT('Ctrl Pts',(-6.76700000000025,-0.18600724940665,
149.311569727996));
#46115=CARTESIAN_POINT('Ctrl Pts',(-6.75932637295488,-0.372014355518504,
149.320319239802));
#46116=CARTESIAN_POINT('Ctrl Pts',(-6.74400518267002,-0.557389537146031,
149.329068751608));
#46117=CARTESIAN_POINT('Ctrl Pts',(-6.72868405709744,-0.742763935802529,
149.337818226458));
#46118=CARTESIAN_POINT('Ctrl Pts',(-6.70571545653112,-0.92750612968633,
149.346567701309));
#46119=CARTESIAN_POINT('Ctrl Pts',(-6.67517739415792,-1.11098863924122,
149.35531717616));
#46120=CARTESIAN_POINT('Ctrl Pts',(-6.64463945823232,-1.29447038905826,
149.364066614782));
#46121=CARTESIAN_POINT('Ctrl Pts',(-6.60653217027305,-1.47669218227555,
149.372816053404));
#46122=CARTESIAN_POINT('Ctrl Pts',(-6.56098496116875,-1.65703510503474,
149.381565492025));
#46123=CARTESIAN_POINT('Ctrl Pts',(-6.51543793687688,-1.83737729603417,
149.390314895146));
#46124=CARTESIAN_POINT('Ctrl Pts',(-6.46245112202815,-2.01584035396493,
149.399064298266));
#46125=CARTESIAN_POINT('Ctrl Pts',(-6.4022044841642,-2.19181813637625,149.407813701386));
#46126=CARTESIAN_POINT('Ctrl Pts',(-6.3419580857538,-2.36779521935426,149.416563069732));
#46127=CARTESIAN_POINT('Ctrl Pts',(-6.27445201489444,-2.5412867754431,149.425312438077));
#46128=CARTESIAN_POINT('Ctrl Pts',(-6.19991555136409,-2.71170355237325,
149.434061806422));
#46129=CARTESIAN_POINT('Ctrl Pts',(-6.12537937789278,-2.88211966612562,
149.442811140719));
#46130=CARTESIAN_POINT('Ctrl Pts',(-6.04381298133871,-3.04946076209941,
149.451560475016));
#46131=CARTESIAN_POINT('Ctrl Pts',(-5.95549339426575,-3.21315848206357,
149.460309809313));
#46132=CARTESIAN_POINT('Ctrl Pts',(-5.86717414355448,-3.37685557859135,
149.469059110289));
#46133=CARTESIAN_POINT('Ctrl Pts',(-5.77210188986546,-3.53690907466809,
149.477808411264));
#46134=CARTESIAN_POINT('Ctrl Pts',(-5.67059953467396,-3.69277536784401,
149.48655771224));
#46135=CARTESIAN_POINT('Ctrl Pts',(-5.56909755762115,-3.84864108035286,
149.495306980621));
#46136=CARTESIAN_POINT('Ctrl Pts',(-5.46116568338442,-4.00031938103771,
149.504056249001));
#46137=CARTESIAN_POINT('Ctrl Pts',(-5.34717048686509,-4.14729511662709,
149.512805517382));
#46138=CARTESIAN_POINT('Ctrl Pts',(-5.23317570555944,-4.2942703168752,149.521554753895));
#46139=CARTESIAN_POINT('Ctrl Pts',(-5.11311782179264,-4.436542759866,149.530303990407));
#46140=CARTESIAN_POINT('Ctrl Pts',(-4.98740459172507,-4.57362924147112,
149.53905322692));
#46141=CARTESIAN_POINT('Ctrl Pts',(-4.86169180911318,-4.71071523513934,
149.547802432291));
#46142=CARTESIAN_POINT('Ctrl Pts',(-4.73032391415912,-4.84261509316055,
149.556551637662));
#46143=CARTESIAN_POINT('Ctrl Pts',(-4.59374707237765,-4.96888084331087,
149.565300843033));
#46144=CARTESIAN_POINT('Ctrl Pts',(-4.45717070537876,-5.09514615452311,
149.57405001799));
#46145=CARTESIAN_POINT('Ctrl Pts',(-4.31538563819983,-5.21577720253241,
149.582799192946));
#46146=CARTESIAN_POINT('Ctrl Pts',(-4.16887341291121,-5.3303642902828,149.591548367902));
#46147=CARTESIAN_POINT('Ctrl Pts',(-4.02236168477824,-5.44495098920818,
149.60029751317));
#46148=CARTESIAN_POINT('Ctrl Pts',(-3.87112305634937,-5.55349359238412,
149.609046658438));
#46149=CARTESIAN_POINT('Ctrl Pts',(-3.71567117317242,-5.65562346102138,
149.617795803706));
#46150=CARTESIAN_POINT('Ctrl Pts',(-3.56021980457814,-5.75775299158452,
149.626544920012));
#46151=CARTESIAN_POINT('Ctrl Pts',(-3.40055544862904,-5.85346967275053,
149.635294036318));
#46152=CARTESIAN_POINT('Ctrl Pts',(-3.23722036323922,-5.94244842803279,
149.644043152624));
#46153=CARTESIAN_POINT('Ctrl Pts',(-3.07388580496577,-6.03142689616205,
149.652792240695));
#46154=CARTESIAN_POINT('Ctrl Pts',(-2.90688079258249,-6.11366734484565,
149.661541328766));
#46155=CARTESIAN_POINT('Ctrl Pts',(-2.73677251095168,-6.18889046787057,
149.670290416837));
#46156=CARTESIAN_POINT('Ctrl Pts',(-2.56666476417227,-6.26411335438031,
149.679039477399));
#46157=CARTESIAN_POINT('Ctrl Pts',(-2.39345402972704,-6.33231884350059,
149.687788537962));
#46158=CARTESIAN_POINT('Ctrl Pts',(-2.21772856474678,-6.39327529620821,
149.696537598524));
#46159=CARTESIAN_POINT('Ctrl Pts',(-2.04200363768948,-6.45423156231866,
149.705286632304));
#46160=CARTESIAN_POINT('Ctrl Pts',(-1.86376426620811,-6.50793874251849,
149.714035666084));
#46161=CARTESIAN_POINT('Ctrl Pts',(-1.68361578195445,-6.55421443795928,
149.722784699864));
#46162=CARTESIAN_POINT('Ctrl Pts',(-1.50346783420668,-6.60048999558496,
149.731533707588));
#46163=CARTESIAN_POINT('Ctrl Pts',(-1.32141106258089,-6.63933404145327,
149.740282715312));
#46164=CARTESIAN_POINT('Ctrl Pts',(-1.13806375959929,-6.67061465526879,
149.749031723036));
#46165=CARTESIAN_POINT('Ctrl Pts',(-0.954716987427849,-6.70189517852357,
149.757780705431));
#46166=CARTESIAN_POINT('Ctrl Pts',(-0.770079973818414,-6.72561226535731,
149.766529687826));
#46167=CARTESIAN_POINT('Ctrl Pts',(-0.584779770560826,-6.7416853693971,
149.775278670221));
#46168=CARTESIAN_POINT('Ctrl Pts',(-0.391490647562162,-6.75845143942346,
149.784404850897));
#46169=CARTESIAN_POINT('Ctrl Pts',(-0.197480213112457,-6.76689975924003,
149.793531031573));
#46170=CARTESIAN_POINT('Ctrl Pts',(-0.00346532630577843,-6.76699911271707,
149.802657212249));
#46171=CARTESIAN_POINT('Ctrl Pts',(0.184486595288163,-6.76709536139795,
149.811498199779));
#46172=CARTESIAN_POINT('Ctrl Pts',(0.372442378177437,-6.75935659726813,
149.820339187309));
#46173=CARTESIAN_POINT('Ctrl Pts',(0.5597502177144,-6.7438096572908,149.829180174839));
#46174=CARTESIAN_POINT('Ctrl Pts',(0.745129914450085,-6.72842275717338,
149.837930153437));
#46175=CARTESIAN_POINT('Ctrl Pts',(0.929874656306541,-6.70538772273579,
149.846680132035));
#46176=CARTESIAN_POINT('Ctrl Pts',(1.11335688289016,-6.67478280180869,149.855430110632));
#46177=CARTESIAN_POINT('Ctrl Pts',(1.29683723118086,-6.64417819418173,149.864179999657));
#46178=CARTESIAN_POINT('Ctrl Pts',(1.47905480729456,-6.60600390230249,149.872929888682));
#46179=CARTESIAN_POINT('Ctrl Pts',(1.65939064804022,-6.56038959797333,149.881679777707));
#46180=CARTESIAN_POINT('Ctrl Pts',(1.8397247026349,-6.51477574543475,149.890429580068));
#46181=CARTESIAN_POINT('Ctrl Pts',(2.01817678125084,-6.46172209820339,149.899179382429));
#46182=CARTESIAN_POINT('Ctrl Pts',(2.19414072346928,-6.40140886724272,149.90792918479));
#46183=CARTESIAN_POINT('Ctrl Pts',(2.37010298131359,-6.3410962136165,149.916678903395));
#46184=CARTESIAN_POINT('Ctrl Pts',(2.5435768792619,-6.27352420826264,149.925428622001));
#46185=CARTESIAN_POINT('Ctrl Pts',(2.71397317789264,-6.19892237325806,149.934178340606));
#46186=CARTESIAN_POINT('Ctrl Pts',(2.88436790206507,-6.1243212275729,149.942927978365));
#46187=CARTESIAN_POINT('Ctrl Pts',(3.05168482125576,-6.04269049717761,149.951677616123));
#46188=CARTESIAN_POINT('Ctrl Pts',(3.21535561996723,-5.95430745235289,149.960427253881));
#46189=CARTESIAN_POINT('Ctrl Pts',(3.37902496074624,-5.86592519481895,149.9691768137));
#46190=CARTESIAN_POINT('Ctrl Pts',(3.53904799384228,-5.77079087940629,149.977926373519));
#46191=CARTESIAN_POINT('Ctrl Pts',(3.69488118814347,-5.66922763747439,149.986675933338));
#46192=CARTESIAN_POINT('Ctrl Pts',(3.85071304610209,-5.56766526649483,149.995425418126));
#46193=CARTESIAN_POINT('Ctrl Pts',(4.00235489705358,-5.45967423581161,150.004174902913));
#46194=CARTESIAN_POINT('Ctrl Pts',(4.14929168607059,-5.3456213393679,150.012924387701));
#46195=CARTESIAN_POINT('Ctrl Pts',(4.29622726385165,-5.23156938309016,150.021673800364));
#46196=CARTESIAN_POINT('Ctrl Pts',(4.43845763091479,-5.11145583677712,150.030423213027));
#46197=CARTESIAN_POINT('Ctrl Pts',(4.5754997066038,-4.98568866204746,150.039172625691));
#46198=CARTESIAN_POINT('Ctrl Pts',(4.7125406981473,-4.85992248226709,150.047921969137));
#46199=CARTESIAN_POINT('Ctrl Pts',(4.84439326930767,-4.72850295734563,150.056671312583));
#46200=CARTESIAN_POINT('Ctrl Pts',(4.97060959434169,-4.59187644222254,150.06542065603));
#46201=CARTESIAN_POINT('Ctrl Pts',(5.09682496279998,-4.45525096257255,150.074169933166));
#46202=CARTESIAN_POINT('Ctrl Pts',(5.21740397615335,-4.31341878218936,150.082919210302));
#46203=CARTESIAN_POINT('Ctrl Pts',(5.33193710451443,-4.16686161439305,150.091668487438));
#46204=CARTESIAN_POINT('Ctrl Pts',(5.44646940288906,-4.0203055086516,150.100417701171));
#46205=CARTESIAN_POINT('Ctrl Pts',(5.55495572749203,-3.86902470980796,150.109166914904));
#46206=CARTESIAN_POINT('Ctrl Pts',(5.65702762491009,-3.71353301466462,150.117916128637));
#46207=CARTESIAN_POINT('Ctrl Pts',(5.75909881654742,-3.55804239467561,150.126665281873));
#46208=CARTESIAN_POINT('Ctrl Pts',(5.85475551250403,-3.39834117620207,150.13541443511));
#46209=CARTESIAN_POINT('Ctrl Pts',(5.94367283727747,-3.23497174692608,150.144163588346));
#46210=CARTESIAN_POINT('Ctrl Pts',(6.03258957675983,-3.07160339301611,150.152912683991));
#46211=CARTESIAN_POINT('Ctrl Pts',(6.11476689684975,-2.90456712830154,150.161661779637));
#46212=CARTESIAN_POINT('Ctrl Pts',(6.18992570524972,-2.73443024476559,150.170410875282));
#46213=CARTESIAN_POINT('Ctrl Pts',(6.26508404388419,-2.56429442463709,150.179159916243));
#46214=CARTESIAN_POINT('Ctrl Pts',(6.33322384283048,-2.39105828656697,150.187908957204));
#46215=CARTESIAN_POINT('Ctrl Pts',(6.3941136871978,-2.21531017132811,150.196657998165));
#46216=CARTESIAN_POINT('Ctrl Pts',(6.45500317120656,-2.03956309620255,150.205406987348));
#46217=CARTESIAN_POINT('Ctrl Pts',(6.50864269269859,-1.86130434439383,150.21415597653));
#46218=CARTESIAN_POINT('Ctrl Pts',(6.55485008446139,-1.68113930720703,150.222904965713));
#46219=CARTESIAN_POINT('Ctrl Pts',(6.60199664749235,-1.49731239212586,150.231831779242));
#46220=CARTESIAN_POINT('Ctrl Pts',(6.64140563640763,-1.31150116500403,150.240758592771));
#46221=CARTESIAN_POINT('Ctrl Pts',(6.67293772282051,-1.12436255156377,150.249685406301));
#46222=CARTESIAN_POINT('Ctrl Pts',(6.70384494949771,-0.940932395058484,
150.258435320456));
#46223=CARTESIAN_POINT('Ctrl Pts',(6.72718449348851,-0.756227260513811,
150.267185234612));
#46224=CARTESIAN_POINT('Ctrl Pts',(6.74287707373872,-0.570874564548736,
150.275935148767));
#46225=CARTESIAN_POINT('Ctrl Pts',(6.7585693453863,-0.385525513639488,150.284684890851));
#46226=CARTESIAN_POINT('Ctrl Pts',(6.76661493004083,-0.199529212425204,
150.293434632935));
#46227=CARTESIAN_POINT('Ctrl Pts',(6.76698649908905,-0.0135174386073543,
150.302184375019));
#46228=CARTESIAN_POINT('Ctrl Pts',(6.76735806132407,0.172490924438802,150.310933956665));
#46229=CARTESIAN_POINT('Ctrl Pts',(6.76005588896326,0.358514472894389,150.319683538311));
#46230=CARTESIAN_POINT('Ctrl Pts',(6.74510478454641,0.54392135965516,150.328433119957));
#46231=CARTESIAN_POINT('Ctrl Pts',(6.73015393440765,0.729325093143337,150.337182552796));
#46232=CARTESIAN_POINT('Ctrl Pts',(6.70755443556994,0.914111900249198,150.345931985635));
#46233=CARTESIAN_POINT('Ctrl Pts',(6.67738304682437,1.09765415590819,150.354681418474));
#46234=CARTESIAN_POINT('Ctrl Pts',(6.64721213111997,1.28119353390565,150.363430714135));
#46235=CARTESIAN_POINT('Ctrl Pts',(6.60946960955649,1.46348811671957,150.372180009797));
#46236=CARTESIAN_POINT('Ctrl Pts',(6.56428366991354,1.64391876347538,150.380929305458));
#46237=CARTESIAN_POINT('Ctrl Pts',(6.51909837867908,1.82434682109034,150.389678475569));
#46238=CARTESIAN_POINT('Ctrl Pts',(6.46646995272131,2.00291071819767,150.39842764568));
#46239=CARTESIAN_POINT('Ctrl Pts',(6.40657713281779,2.17900400212029,150.40717681579));
#46240=CARTESIAN_POINT('Ctrl Pts',(6.34668509279304,2.35509499309002,150.415925871976));
#46241=CARTESIAN_POINT('Ctrl Pts',(6.27952894037783,2.52871516397484,150.424674928162));
#46242=CARTESIAN_POINT('Ctrl Pts',(6.20533675061716,2.699274867708,150.433423984348));
#46243=CARTESIAN_POINT('Ctrl Pts',(6.12832117908193,2.87632521635336,150.44250598563));
#46244=CARTESIAN_POINT('Ctrl Pts',(6.0437236662636,3.05007728919442,150.451587986912));
#46245=CARTESIAN_POINT('Ctrl Pts',(5.95185378008151,3.21989527477672,150.460669988195));
#46246=CARTESIAN_POINT('Ctrl Pts',(5.86334450817671,3.38350129286232,150.469419768502));
#46247=CARTESIAN_POINT('Ctrl Pts',(5.76808562057572,3.54345567124447,150.478169548809));
#46248=CARTESIAN_POINT('Ctrl Pts',(5.66640068804817,3.69921508464799,150.486919329116));
#46249=CARTESIAN_POINT('Ctrl Pts',(5.56471941108274,3.85496889851777,150.495668794869));
#46250=CARTESIAN_POINT('Ctrl Pts',(5.45661270815482,4.00652780919135,150.504418260623));
#46251=CARTESIAN_POINT('Ctrl Pts',(5.342447764495,4.15337704568733,150.513167726376));
#46252=CARTESIAN_POINT('Ctrl Pts',(5.22828631819995,4.30022178355763,150.521916924096));
#46253=CARTESIAN_POINT('Ctrl Pts',(5.10806717844484,4.44235690972202,150.530666121816));
#46254=CARTESIAN_POINT('Ctrl Pts',(4.98219864545147,4.57929969070179,150.539415319535));
#46255=CARTESIAN_POINT('Ctrl Pts',(4.85633329944467,4.71623900429546,150.548164295725));
#46256=CARTESIAN_POINT('Ctrl Pts',(4.72481904034104,4.84798602483173,150.556913271916));
#46257=CARTESIAN_POINT('Ctrl Pts',(4.58810250737667,4.97409332258693,150.565662248106));
#46258=CARTESIAN_POINT('Ctrl Pts',(4.45137708686117,5.10020881821721,150.574411793042));
#46259=CARTESIAN_POINT('Ctrl Pts',(4.30944892636532,5.22068366307537,150.583161337978));
#46260=CARTESIAN_POINT('Ctrl Pts',(4.16280009467146,5.33510865604472,150.591910882914));
#46261=CARTESIAN_POINT('Ctrl Pts',(4.01615988349291,5.44952692272521,150.600659913523));
#46262=CARTESIAN_POINT('Ctrl Pts',(3.8647997823275,5.55789587288265,150.609408944131));
#46263=CARTESIAN_POINT('Ctrl Pts',(3.70923383581604,5.65984746713526,150.618157974739));
#46264=CARTESIAN_POINT('Ctrl Pts',(3.55366577800089,5.76180044505044,150.626907124087));
#46265=CARTESIAN_POINT('Ctrl Pts',(3.39389200027401,5.85733573570734,150.635656273435));
#46266=CARTESIAN_POINT('Ctrl Pts',(3.23045513626613,5.94612887621617,150.644405422783));
#46267=CARTESIAN_POINT('Ctrl Pts',(3.18695122151961,5.96976399206486,150.646734286896));
#46268=CARTESIAN_POINT('Ctrl Pts',(3.14318791262855,5.99292165435235,150.649063151009));
#46269=CARTESIAN_POINT('Ctrl Pts',(3.09917575053255,6.01559628526641,150.651392015123));
#46270=CARTESIAN_POINT('Origin',(0.,0.,-3.69717978381041));
#46271=CARTESIAN_POINT('',(3.09917575053261,6.01559628526638,153.045781927116));
#46272=CARTESIAN_POINT('',(3.0991757505326,6.01559628526638,152.651615498439));
#46273=CARTESIAN_POINT('',(3.09917575053259,6.01559628526639,-3.69717978381041));
#46274=CARTESIAN_POINT('',(-6.76699781313954,-0.0054403092439294,151.697179783855));
#46275=CARTESIAN_POINT('Ctrl Pts',(-6.76699781313954,-0.00544030924374474,
151.697179783855));
#46276=CARTESIAN_POINT('Ctrl Pts',(-6.76682066285936,-0.225790937285296,
151.707538286931));
#46277=CARTESIAN_POINT('Ctrl Pts',(-6.75587712910279,-0.445703616568735,
151.717896790007));
#46278=CARTESIAN_POINT('Ctrl Pts',(-6.73431712015831,-0.664275488892024,
151.728255293083));
#46279=CARTESIAN_POINT('Ctrl Pts',(-6.71240037143604,-0.886463931197475,
151.738785191732));
#46280=CARTESIAN_POINT('Ctrl Pts',(-6.67951292140793,-1.10726700774589,
151.749315090381));
#46281=CARTESIAN_POINT('Ctrl Pts',(-6.63586112722697,-1.32575868850933,
151.75984498903));
#46282=CARTESIAN_POINT('Ctrl Pts',(-6.61854007886523,-1.41245626967753,
151.764023256777));
#46283=CARTESIAN_POINT('Ctrl Pts',(-6.599524712548,-1.49879014981483,151.768201524525));
#46284=CARTESIAN_POINT('Ctrl Pts',(-6.57883001468178,-1.58470332804665,
151.772379792272));
#46285=CARTESIAN_POINT('Ctrl Pts',(-6.53601859897826,-1.7624331413288,151.781023434166));
#46286=CARTESIAN_POINT('Ctrl Pts',(-6.48596221488716,-1.9385873517263,151.78966707606));
#46287=CARTESIAN_POINT('Ctrl Pts',(-6.42879045362175,-2.11256770386701,
151.798310717954));
#46288=CARTESIAN_POINT('Ctrl Pts',(-6.37169244615921,-2.28632361456472,
151.806943209212));
#46289=CARTESIAN_POINT('Ctrl Pts',(-6.30749745980911,-2.45791097036454,
151.815575700471));
#46290=CARTESIAN_POINT('Ctrl Pts',(-6.23638551469233,-2.62674412764847,
151.824208191729));
#46291=CARTESIAN_POINT('Ctrl Pts',(-6.16273537061777,-2.8016034475293,151.833148802535));
#46292=CARTESIAN_POINT('Ctrl Pts',(-6.08166543488737,-2.97350801273204,
151.84208941334));
#46293=CARTESIAN_POINT('Ctrl Pts',(-5.99343230693078,-3.1418240215261,151.851030024146));
#46294=CARTESIAN_POINT('Ctrl Pts',(-5.90847739352962,-3.30388641557568,
151.859638455405));
#46295=CARTESIAN_POINT('Ctrl Pts',(-5.81688210052459,-3.4626217765525,151.868246886663));
#46296=CARTESIAN_POINT('Ctrl Pts',(-5.71892465582685,-3.61748390196497,
151.876855317922));
#46297=CARTESIAN_POINT('Ctrl Pts',(-5.62106020070992,-3.77219901900898,
151.885455577321));
#46298=CARTESIAN_POINT('Ctrl Pts',(-5.5168457975921,-3.92304797382831,151.894055836721));
#46299=CARTESIAN_POINT('Ctrl Pts',(-5.40660531102839,-4.06950955408139,
151.90265609612));
#46300=CARTESIAN_POINT('Ctrl Pts',(-5.29648918255778,-4.21580591660546,
151.911246653895));
#46301=CARTESIAN_POINT('Ctrl Pts',(-5.18036071515962,-4.35772453466346,
151.91983721167));
#46302=CARTESIAN_POINT('Ctrl Pts',(-5.05858687090311,-4.4947733946804,151.928427769444));
#46303=CARTESIAN_POINT('Ctrl Pts',(-5.04409142298777,-4.51108711643535,
151.929450353428));
#46304=CARTESIAN_POINT('Ctrl Pts',(-5.02951603259424,-4.52733187070495,
151.930472937412));
#46305=CARTESIAN_POINT('Ctrl Pts',(-5.01486135872867,-4.54350685624332,
151.931495521396));
#46306=CARTESIAN_POINT('Ctrl Pts',(-4.89152421449246,-4.6796392971741,151.940101826078));
#46307=CARTESIAN_POINT('Ctrl Pts',(-4.76271597648191,-4.8106636564498,151.948708130761));
#46308=CARTESIAN_POINT('Ctrl Pts',(-4.62888841512035,-4.93616055658288,
151.957314435443));
#46309=CARTESIAN_POINT('Ctrl Pts',(-4.49493053380187,-5.06177966435729,
151.96592912086));
#46310=CARTESIAN_POINT('Ctrl Pts',(-4.35594379387702,-5.18186036088778,
151.974543806276));
#46311=CARTESIAN_POINT('Ctrl Pts',(-4.21241341248116,-5.29602324790487,
151.983158491693));
#46312=CARTESIAN_POINT('Ctrl Pts',(-4.06322305990135,-5.41468802953486,
151.992112888262));
#46313=CARTESIAN_POINT('Ctrl Pts',(-3.90912375108719,-5.52695858495553,
152.001067284831));
#46314=CARTESIAN_POINT('Ctrl Pts',(-3.75069272947807,-5.63245888125607,
152.0100216814));
#46315=CARTESIAN_POINT('Ctrl Pts',(-3.5978452869411,-5.73424103422492,152.018660498477));
#46316=CARTESIAN_POINT('Ctrl Pts',(-3.44096652223121,-5.82972188038494,
152.027299315554));
#46317=CARTESIAN_POINT('Ctrl Pts',(-3.28059960474056,-5.91861092093205,
152.035938132631));
#46318=CARTESIAN_POINT('Ctrl Pts',(-3.12007657215159,-6.00758649379843,
152.044585359483));
#46319=CARTESIAN_POINT('Ctrl Pts',(-2.95605887790096,-6.08995731281826,
152.053232586336));
#46320=CARTESIAN_POINT('Ctrl Pts',(-2.78911142845873,-6.16548022782013,
152.061879813188));
#46321=CARTESIAN_POINT('Ctrl Pts',(-2.62191369320887,-6.24111636595801,
152.070540003869));
#46322=CARTESIAN_POINT('Ctrl Pts',(-2.45177770476479,-6.30988396628493,
152.079200194551));
#46323=CARTESIAN_POINT('Ctrl Pts',(-2.27928676565387,-6.37158856486474,
152.087860385232));
#46324=CARTESIAN_POINT('Ctrl Pts',(-2.26102314405801,-6.37812194827024,
152.088777340328));
#46325=CARTESIAN_POINT('Ctrl Pts',(-2.24273313349377,-6.3845761955102,152.089694295423));
#46326=CARTESIAN_POINT('Ctrl Pts',(-2.22441743461814,-6.39095110891695,
152.090611250519));
#46327=CARTESIAN_POINT('Ctrl Pts',(-2.06044476477771,-6.44802299999824,
152.098820359882));
#46328=CARTESIAN_POINT('Ctrl Pts',(-1.89405170220875,-6.49885770803804,
152.107029469246));
#46329=CARTESIAN_POINT('Ctrl Pts',(-1.72575409940623,-6.54324550879627,
152.115238578609));
#46330=CARTESIAN_POINT('Ctrl Pts',(-1.55763559982528,-6.58758607181623,
152.123438951794));
#46331=CARTESIAN_POINT('Ctrl Pts',(-1.38761694091712,-6.62549329787349,
152.131639324979));
#46332=CARTESIAN_POINT('Ctrl Pts',(-1.21623222764221,-6.65680615373803,
152.139839698164));
#46333=CARTESIAN_POINT('Ctrl Pts',(-1.04499519193563,-6.68809202816225,
152.148033005309));
#46334=CARTESIAN_POINT('Ctrl Pts',(-0.872394798051353,-6.71279478400163,
152.156226312454));
#46335=CARTESIAN_POINT('Ctrl Pts',(-0.698978604547322,-6.73080366006802,
152.1644196196));
#46336=CARTESIAN_POINT('Ctrl Pts',(-0.525676726956045,-6.74880066468767,
152.172607525719));
#46337=CARTESIAN_POINT('Ctrl Pts',(-0.351560477592479,-6.76011254137418,
152.180795431838));
#46338=CARTESIAN_POINT('Ctrl Pts',(-0.177185936192593,-6.76467989959729,
152.188983337957));
#46339=CARTESIAN_POINT('Ctrl Pts',(-0.00289104353758479,-6.76924517159641,
152.197167504101));
#46340=CARTESIAN_POINT('Ctrl Pts',(0.171661547038031,-6.76707205286047,
152.205351670245));
#46341=CARTESIAN_POINT('Ctrl Pts',(0.345912251864701,-6.75815312892582,
152.213535836389));
#46342=CARTESIAN_POINT('Ctrl Pts',(0.52014864388683,-6.74923493758399,152.221719330293));
#46343=CARTESIAN_POINT('Ctrl Pts',(0.694082839869698,-6.73357205407506,
152.229902824196));
#46344=CARTESIAN_POINT('Ctrl Pts',(0.867156516699929,-6.71120917387805,
152.2380863181));
#46345=CARTESIAN_POINT('Ctrl Pts',(1.04022887084597,-6.68884646458529,152.246269749463));
#46346=CARTESIAN_POINT('Ctrl Pts',(1.21244036167865,-6.65978390559459,152.254453180825));
#46347=CARTESIAN_POINT('Ctrl Pts',(1.38323918504562,-6.6241179304836,152.262636612188));
#46348=CARTESIAN_POINT('Ctrl Pts',(1.55406802980395,-6.58844568634701,152.270821481956));
#46349=CARTESIAN_POINT('Ctrl Pts',(1.72348335993138,-6.54616778734753,152.279006351725));
#46350=CARTESIAN_POINT('Ctrl Pts',(1.89094490308364,-6.497431521263,152.287191221493));
#46351=CARTESIAN_POINT('Ctrl Pts',(2.05846659610467,-6.44867774978616,152.295379031154));
#46352=CARTESIAN_POINT('Ctrl Pts',(2.22403275876064,-6.39346109100412,152.303566840814));
#46353=CARTESIAN_POINT('Ctrl Pts',(2.38711954936351,-6.33197830516234,152.311754650474));
#46354=CARTESIAN_POINT('Ctrl Pts',(2.55039578527835,-6.27042409952316,152.31995197128));
#46355=CARTESIAN_POINT('Ctrl Pts',(2.71118655795087,-6.20258935209995,152.328149292086));
#46356=CARTESIAN_POINT('Ctrl Pts',(2.86898826530126,-6.12871889823344,152.336346612891));
#46357=CARTESIAN_POINT('Ctrl Pts',(3.02688424282071,-6.05480431442504,152.344548830747));
#46358=CARTESIAN_POINT('Ctrl Pts',(3.18178727646132,-5.97484700216473,152.352751048602));
#46359=CARTESIAN_POINT('Ctrl Pts',(3.33321970147719,-5.88913706935782,152.360953266457));
#46360=CARTESIAN_POINT('Ctrl Pts',(3.48489273404859,-5.80329095397696,152.369168516631));
#46361=CARTESIAN_POINT('Ctrl Pts',(3.63308383197254,-5.71167414139782,152.377383766805));
#46362=CARTESIAN_POINT('Ctrl Pts',(3.77734444563583,-5.61462001733191,152.385599016979));
#46363=CARTESIAN_POINT('Ctrl Pts',(3.91339829548935,-5.52308715269189,152.393346914241));
#46364=CARTESIAN_POINT('Ctrl Pts',(4.04595622289335,-5.42671854493955,152.401094811504));
#46365=CARTESIAN_POINT('Ctrl Pts',(4.17467077253493,-5.32582509485081,152.408842708766));
#46366=CARTESIAN_POINT('Ctrl Pts',(4.31045240636619,-5.21939208060285,152.41701600504));
#46367=CARTESIAN_POINT('Ctrl Pts',(4.44237888345318,-5.10759238998213,152.425189301315));
#46368=CARTESIAN_POINT('Ctrl Pts',(4.56999418349115,-4.99073563343693,152.433362597589));
#46369=CARTESIAN_POINT('Ctrl Pts',(4.6974537140481,-4.87402151430523,152.441525917394));
#46370=CARTESIAN_POINT('Ctrl Pts',(4.82061227768349,-4.75226286039346,152.449689237199));
#46371=CARTESIAN_POINT('Ctrl Pts',(4.93904408494467,-4.6258115533356,152.457852557004));
#46372=CARTESIAN_POINT('Ctrl Pts',(5.05735599433471,-4.49948826292183,152.466007612436));
#46373=CARTESIAN_POINT('Ctrl Pts',(5.1709504277376,-4.36848204158194,152.474162667868));
#46374=CARTESIAN_POINT('Ctrl Pts',(5.27943585967152,-4.23318390855092,152.482317723299));
#46375=CARTESIAN_POINT('Ctrl Pts',(5.38783404239173,-4.09799458880029,152.490466220042));
#46376=CARTESIAN_POINT('Ctrl Pts',(5.49113117897016,-3.95852051332946,152.498614716785));
#46377=CARTESIAN_POINT('Ctrl Pts',(5.58897370801332,-3.81518831660193,152.506763213529));
#46378=CARTESIAN_POINT('Ctrl Pts',(5.68675790427688,-3.6719415731586,152.514906852216));
#46379=CARTESIAN_POINT('Ctrl Pts',(5.77909376505791,-3.52484158931778,152.523050490903));
#46380=CARTESIAN_POINT('Ctrl Pts',(5.86566902263997,-3.37434673927293,152.53119412959));
#46381=CARTESIAN_POINT('Ctrl Pts',(5.95243595276715,-3.22351870245232,152.539355797816));
#46382=CARTESIAN_POINT('Ctrl Pts',(6.03341652519195,-3.06928104646432,152.547517466042));
#46383=CARTESIAN_POINT('Ctrl Pts',(6.10834065229936,-2.91212353368931,152.555679134268));
#46384=CARTESIAN_POINT('Ctrl Pts',(6.18306921713104,-2.75537622363578,152.563819499418));
#46385=CARTESIAN_POINT('Ctrl Pts',(6.25177276618944,-2.59572461526402,152.571959864567));
#46386=CARTESIAN_POINT('Ctrl Pts',(6.31422997937869,-2.43367803283742,152.580100229717));
#46387=CARTESIAN_POINT('Ctrl Pts',(6.37669114641939,-2.27162119205822,152.588241110191));
#46388=CARTESIAN_POINT('Ctrl Pts',(6.43290505884602,-2.1071694150306,152.596381990666));
#46389=CARTESIAN_POINT('Ctrl Pts',(6.48269916034021,-1.94085048278437,152.604522871141));
#46390=CARTESIAN_POINT('Ctrl Pts',(6.53250579729907,-1.77448968041626,152.61266580105));
#46391=CARTESIAN_POINT('Ctrl Pts',(6.57588930064009,-1.60626113560997,152.620808730959));
#46392=CARTESIAN_POINT('Ctrl Pts',(6.61272745042785,-1.43670618651064,152.628951660868));
#46393=CARTESIAN_POINT('Ctrl Pts',(6.64971916818584,-1.26644441012698,152.63712853638));
#46394=CARTESIAN_POINT('Ctrl Pts',(6.68011076325744,-1.0948455081302,152.645305411892));
#46395=CARTESIAN_POINT('Ctrl Pts',(6.703830722841,-0.922465522116235,152.653482287404));
#46396=CARTESIAN_POINT('Ctrl Pts',(6.72748854798329,-0.750537085527412,
152.661637743588));
#46397=CARTESIAN_POINT('Ctrl Pts',(6.74450966163421,-0.577832019655981,
152.669793199773));
#46398=CARTESIAN_POINT('Ctrl Pts',(6.75487538359512,-0.404904374020209,
152.677948655957));
#46399=CARTESIAN_POINT('Ctrl Pts',(6.76528194204491,-0.231295467792647,
152.686136241133));
#46400=CARTESIAN_POINT('Ctrl Pts',(6.7689805684702,-0.0574625941143888,
152.694323826309));
#46401=CARTESIAN_POINT('Ctrl Pts',(6.76600505955837,0.116036778784197,152.702511411485));
#46402=CARTESIAN_POINT('Ctrl Pts',(6.76302955064653,0.289536151682656,152.710698996661));
#46403=CARTESIAN_POINT('Ctrl Pts',(6.75337998421799,0.462701662475575,152.718886581837));
#46404=CARTESIAN_POINT('Ctrl Pts',(6.73714210211013,0.634984484830179,152.727074167013));
#46405=CARTESIAN_POINT('Ctrl Pts',(6.72080726251413,0.80829601952519,152.735310640812));
#46406=CARTESIAN_POINT('Ctrl Pts',(6.69775835998404,0.981212097610075,152.74354711461));
#46407=CARTESIAN_POINT('Ctrl Pts',(6.66801914461703,1.15317374537436,152.751783588409));
#46408=CARTESIAN_POINT('Ctrl Pts',(6.63831273267355,1.32494571326005,152.760010977081));
#46409=CARTESIAN_POINT('Ctrl Pts',(6.60193076403463,1.49576499809945,152.768238365753));
#46410=CARTESIAN_POINT('Ctrl Pts',(6.55894885626404,1.66507624477458,152.776465754426));
#46411=CARTESIAN_POINT('Ctrl Pts',(6.51600580488551,1.83423443113852,152.784685705395));
#46412=CARTESIAN_POINT('Ctrl Pts',(6.46647478491051,2.00188695012239,152.792905656365));
#46413=CARTESIAN_POINT('Ctrl Pts',(6.41048273242969,2.16748705583697,152.801125607335));
#46414=CARTESIAN_POINT('Ctrl Pts',(6.35453015777041,2.33297040334873,152.809339762736));
#46415=CARTESIAN_POINT('Ctrl Pts',(6.29212573879177,2.49640388273475,152.817553918138));
#46416=CARTESIAN_POINT('Ctrl Pts',(6.22344669317352,2.65725427033763,152.825768073539));
#46417=CARTESIAN_POINT('Ctrl Pts',(6.15480240948141,2.81802324345311,152.833978071343));
#46418=CARTESIAN_POINT('Ctrl Pts',(6.07988996652485,2.97621140154097,152.842188069146));
#46419=CARTESIAN_POINT('Ctrl Pts',(5.99893534885182,3.13130383072229,152.85039806695));
#46420=CARTESIAN_POINT('Ctrl Pts',(5.91799446527066,3.28636994820293,152.858606671913));
#46421=CARTESIAN_POINT('Ctrl Pts',(5.83101360838452,3.438341063342,152.866815276876));
#46422=CARTESIAN_POINT('Ctrl Pts',(5.73826566776904,3.58672498612636,152.875023881839));
#46423=CARTESIAN_POINT('Ctrl Pts',(5.64552342457804,3.73509979381675,152.883231982555));
#46424=CARTESIAN_POINT('Ctrl Pts',(5.54701499199426,3.87988754437472,152.89144008327));
#46425=CARTESIAN_POINT('Ctrl Pts',(5.44305769737916,4.02062332269531,152.899648183986));
#46426=CARTESIAN_POINT('Ctrl Pts',(5.33908805214441,4.16137582109384,152.907857259863));
#46427=CARTESIAN_POINT('Ctrl Pts',(5.22966846758373,4.29807510049649,152.91606633574));
#46428=CARTESIAN_POINT('Ctrl Pts',(5.11515785859708,4.43028769738857,152.924275411617));
#46429=CARTESIAN_POINT('Ctrl Pts',(5.00061300646012,4.56253983101763,152.932486942329));
#46430=CARTESIAN_POINT('Ctrl Pts',(4.88097433125103,4.69030233929231,152.94069847304));
#46431=CARTESIAN_POINT('Ctrl Pts',(4.75663908369482,4.81317708249623,152.948910003752));
#46432=CARTESIAN_POINT('Ctrl Pts',(4.6321733316871,4.93618079718074,152.95713015343));
#46433=CARTESIAN_POINT('Ctrl Pts',(4.5030014132024,5.05428624544385,152.965350303108));
#46434=CARTESIAN_POINT('Ctrl Pts',(4.36955604258135,5.16713353715006,152.973570452786));
#46435=CARTESIAN_POINT('Ctrl Pts',(4.2360385128263,5.28004184980293,152.981795047421));
#46436=CARTESIAN_POINT('Ctrl Pts',(4.09824320547279,5.38768611750558,152.990019642055));
#46437=CARTESIAN_POINT('Ctrl Pts',(3.95663349822709,5.48974866097778,152.99824423669));
#46438=CARTESIAN_POINT('Ctrl Pts',(3.81481632539584,5.59196073138394,153.006480880783));
#46439=CARTESIAN_POINT('Ctrl Pts',(3.66917388251207,5.68857453730499,153.014717524877));
#46440=CARTESIAN_POINT('Ctrl Pts',(3.5201970339267,5.77931672798209,153.02295416897));
#46441=CARTESIAN_POINT('Ctrl Pts',(3.38543950074021,5.86139789621528,153.0304046544));
#46442=CARTESIAN_POINT('Ctrl Pts',(3.24795419331786,5.93867531269824,153.03785513983));
#46443=CARTESIAN_POINT('Ctrl Pts',(3.10811898405032,6.01098040098169,153.04530562526));
#46444=CARTESIAN_POINT('Ctrl Pts',(3.10513914377014,6.01252119757833,153.045464392545));
#46445=CARTESIAN_POINT('Ctrl Pts',(3.10215806480747,6.01405982642792,153.045623159831));
#46446=CARTESIAN_POINT('Ctrl Pts',(3.09917575053261,6.01559628526638,153.045781927116));
#46447=CARTESIAN_POINT('Ctrl Pts',(3.09917575053262,6.01559628526637,151.045614412788));
#46448=CARTESIAN_POINT('Ctrl Pts',(2.94387213756178,6.09560717171302,151.053822491478));
#46449=CARTESIAN_POINT('Ctrl Pts',(2.78556183173075,6.16955175392866,151.062030570168));
#46450=CARTESIAN_POINT('Ctrl Pts',(2.62476468355848,6.23721887991308,151.070238648858));
#46451=CARTESIAN_POINT('Ctrl Pts',(2.46387447321858,6.30492516859095,151.078451478015));
#46452=CARTESIAN_POINT('Ctrl Pts',(2.30049488689371,6.36634663295596,151.086664307172));
#46453=CARTESIAN_POINT('Ctrl Pts',(2.13516212173171,6.42132164853328,151.09487713633));
#46454=CARTESIAN_POINT('Ctrl Pts',(1.96959745390637,6.47637377437072,151.103101485145));
#46455=CARTESIAN_POINT('Ctrl Pts',(1.80207447805811,6.52496128703662,151.111325833961));
#46456=CARTESIAN_POINT('Ctrl Pts',(1.633141877495,6.56697316942685,151.119550182777));
#46457=CARTESIAN_POINT('Ctrl Pts',(1.52108161702273,6.5948414581283,151.125005747111));
#46458=CARTESIAN_POINT('Ctrl Pts',(1.40840128980731,6.61981737147946,151.130461311445));
#46459=CARTESIAN_POINT('Ctrl Pts',(1.295262361097,6.64188109016756,151.135916875779));
#46460=CARTESIAN_POINT('Ctrl Pts',(1.12619762638398,6.67485114556148,151.144069185045));
#46461=CARTESIAN_POINT('Ctrl Pts',(0.955608083129771,6.70141354431739,151.152221494311));
#46462=CARTESIAN_POINT('Ctrl Pts',(0.78402508820873,6.72142794806723,151.160373803576));
#46463=CARTESIAN_POINT('Ctrl Pts',(0.61264136654608,6.74141910746555,151.168516644904));
#46464=CARTESIAN_POINT('Ctrl Pts',(0.440266849311369,6.75487736779777,151.176659486231));
#46465=CARTESIAN_POINT('Ctrl Pts',(0.267444897019827,6.76171296544434,151.184802327558));
#46466=CARTESIAN_POINT('Ctrl Pts',(0.0947873154990069,6.76854206176143,
151.192937424238));
#46467=CARTESIAN_POINT('Ctrl Pts',(-0.0783164910748943,6.76876102111578,
151.201072520918));
#46468=CARTESIAN_POINT('Ctrl Pts',(-0.251316192730467,6.76233163718488,
151.209207617598));
#46469=CARTESIAN_POINT('Ctrl Pts',(-0.424187713524088,6.75590701698458,
151.217336686732));
#46470=CARTESIAN_POINT('Ctrl Pts',(-0.596954919196228,6.74284387543872,
151.225465755865));
#46471=CARTESIAN_POINT('Ctrl Pts',(-0.769065619154389,6.72315603518427,
151.233594824999));
#46472=CARTESIAN_POINT('Ctrl Pts',(-0.941084955812843,6.70347864602932,
151.241719578895));
#46473=CARTESIAN_POINT('Ctrl Pts',(-1.11244811839762,6.67718360315843,151.249844332791));
#46474=CARTESIAN_POINT('Ctrl Pts',(-1.28260618693369,6.64433671401739,151.257969086686));
#46475=CARTESIAN_POINT('Ctrl Pts',(-1.45379845852855,6.6112901848974,151.266143221992));
#46476=CARTESIAN_POINT('Ctrl Pts',(-1.6237705644435,6.5716119233359,151.274317357298));
#46477=CARTESIAN_POINT('Ctrl Pts',(-1.79197154642861,6.52542159379685,151.282491492604));
#46478=CARTESIAN_POINT('Ctrl Pts',(-1.95911821829167,6.4795207924841,151.290614391148));
#46479=CARTESIAN_POINT('Ctrl Pts',(-2.12451555646846,6.42718945040662,151.298737289692));
#46480=CARTESIAN_POINT('Ctrl Pts',(-2.28763618556708,6.36859558163997,151.306860188237));
#46481=CARTESIAN_POINT('Ctrl Pts',(-2.45077822839969,6.30999402093683,151.314984153118));
#46482=CARTESIAN_POINT('Ctrl Pts',(-2.61164262248649,6.24512841972122,151.323108118));
#46483=CARTESIAN_POINT('Ctrl Pts',(-2.76972026942334,6.17421562865645,151.331232082881));
#46484=CARTESIAN_POINT('Ctrl Pts',(-2.92784874914383,6.10328003427549,151.339358660174));
#46485=CARTESIAN_POINT('Ctrl Pts',(-3.08318836359391,6.02629352742905,151.347485237466));
#46486=CARTESIAN_POINT('Ctrl Pts',(-3.23525303135444,5.94351973355115,151.355611814758));
#46487=CARTESIAN_POINT('Ctrl Pts',(-3.38890446546756,5.8598822106234,151.363823191364));
#46488=CARTESIAN_POINT('Ctrl Pts',(-3.53921188552433,5.77033612681724,151.372034567969));
#46489=CARTESIAN_POINT('Ctrl Pts',(-3.68570311014295,5.67519881448066,151.380245944575));
#46490=CARTESIAN_POINT('Ctrl Pts',(-3.83093187624985,5.58088139364305,151.388386555697));
#46491=CARTESIAN_POINT('Ctrl Pts',(-3.97240970507219,5.48106900138085,151.39652716682));
#46492=CARTESIAN_POINT('Ctrl Pts',(-4.10970947800898,5.3761116995802,151.404667777942));
#46493=CARTESIAN_POINT('Ctrl Pts',(-4.24879954984783,5.26978582346835,151.41291453729));
#46494=CARTESIAN_POINT('Ctrl Pts',(-4.38360155522664,5.15818018942659,151.421161296637));
#46495=CARTESIAN_POINT('Ctrl Pts',(-4.51370994905373,5.0416972832384,151.429408055984));
#46496=CARTESIAN_POINT('Ctrl Pts',(-4.64381834288091,4.92521437705012,151.437654815331));
#46497=CARTESIAN_POINT('Ctrl Pts',(-4.76923289663995,4.80385451259961,151.445901574678));
#46498=CARTESIAN_POINT('Ctrl Pts',(-4.88959050076544,4.67805448181447,151.454148334026));
#46499=CARTESIAN_POINT('Ctrl Pts',(-5.0088099671827,4.55344405396111,151.462317109536));
#46500=CARTESIAN_POINT('Ctrl Pts',(-5.12345180751663,4.424075684855,151.470485885046));
#46501=CARTESIAN_POINT('Ctrl Pts',(-5.2331094156714,4.29032106532965,151.478654660556));
#46502=CARTESIAN_POINT('Ctrl Pts',(-5.34263232504818,4.1567307443341,151.486813401887));
#46503=CARTESIAN_POINT('Ctrl Pts',(-5.44718296239913,4.0187651788118,151.494972143218));
#46504=CARTESIAN_POINT('Ctrl Pts',(-5.54639079289593,3.87683352395732,151.503130884549));
#46505=CARTESIAN_POINT('Ctrl Pts',(-5.64547523653223,3.73507839248016,151.511279478683));
#46506=CARTESIAN_POINT('Ctrl Pts',(-5.7392299068261,3.58936729755277,151.519428072816));
#46507=CARTESIAN_POINT('Ctrl Pts',(-5.82732409670485,3.44014285633068,151.527576666949));
#46508=CARTESIAN_POINT('Ctrl Pts',(-5.91535540066671,3.29102493877173,151.53571944422));
#46509=CARTESIAN_POINT('Ctrl Pts',(-5.9977340828456,3.13839897948418,151.54386222149));
#46510=CARTESIAN_POINT('Ctrl Pts',(-6.07417207465694,2.98273743521916,151.552004998761));
#46511=CARTESIAN_POINT('Ctrl Pts',(-6.15056996188726,2.82715756161119,151.560143503776));
#46512=CARTESIAN_POINT('Ctrl Pts',(-6.22103320390696,2.66854560029287,151.56828200879));
#46513=CARTESIAN_POINT('Ctrl Pts',(-6.28531914140873,2.50739950758572,151.576420513805));
#46514=CARTESIAN_POINT('Ctrl Pts',(-6.34958351078944,2.34630747986649,151.584556288327));
#46515=CARTESIAN_POINT('Ctrl Pts',(-6.40767456819633,2.18268335226831,151.592692062849));
#46516=CARTESIAN_POINT('Ctrl Pts',(-6.45939737997885,2.01704598051764,151.600827837371));
#46517=CARTESIAN_POINT('Ctrl Pts',(-6.51112495630825,1.85139335076001,151.608964361336));
#46518=CARTESIAN_POINT('Ctrl Pts',(-6.55648299694826,1.68372745157347,151.617100885301));
#46519=CARTESIAN_POINT('Ctrl Pts',(-6.59532603339712,1.51458361049967,151.625237409265));
#46520=CARTESIAN_POINT('Ctrl Pts',(-6.63416951338339,1.34543783802121,151.633374026139));
#46521=CARTESIAN_POINT('Ctrl Pts',(-6.66649776433342,1.17481444681058,151.641510643012));
#46522=CARTESIAN_POINT('Ctrl Pts',(-6.69221627720592,1.00325983628379,151.649647259886));
#46523=CARTESIAN_POINT('Ctrl Pts',(-6.71795126802431,0.831595310086349,
151.65778908992));
#46524=CARTESIAN_POINT('Ctrl Pts',(-6.73706800780001,0.658998734044302,
151.665930919953));
#46525=CARTESIAN_POINT('Ctrl Pts',(-6.7495237187244,0.486023219997578,151.674072749987));
#46526=CARTESIAN_POINT('Ctrl Pts',(-6.76130708652667,0.322384699870326,
151.681775094595));
#46527=CARTESIAN_POINT('Ctrl Pts',(-6.76712953799064,0.158407349923215,
151.689477439202));
#46528=CARTESIAN_POINT('Ctrl Pts',(-6.7669978131403,-0.0054403082953369,
151.69717978381));
#46529=CARTESIAN_POINT('',(-6.767,9.16835936326781E-12,151.30282021619));
#46530=CARTESIAN_POINT('Ctrl Pts',(3.09917575053255,6.01559628526641,150.651392015123));
#46531=CARTESIAN_POINT('Ctrl Pts',(2.93382384459255,6.10078395293764,150.660141463035));
#46532=CARTESIAN_POINT('Ctrl Pts',(2.76495772122967,6.17915010267057,150.668890910947));
#46533=CARTESIAN_POINT('Ctrl Pts',(2.59315093316688,6.25042856433187,150.67764035886));
#46534=CARTESIAN_POINT('Ctrl Pts',(2.42134553245598,6.32170645041458,150.68638973612));
#46535=CARTESIAN_POINT('Ctrl Pts',(2.24659977927575,6.38589665313463,150.69513911338));
#46536=CARTESIAN_POINT('Ctrl Pts',(2.06950718689908,6.44278115439079,150.70388849064));
#46537=CARTESIAN_POINT('Ctrl Pts',(1.89241596572854,6.49966521519726,150.712637800154));
#46538=CARTESIAN_POINT('Ctrl Pts',(1.71297821457195,6.54924360009547,150.721387109669));
#46539=CARTESIAN_POINT('Ctrl Pts',(1.53180337335846,6.59134792173556,150.730136419184));
#46540=CARTESIAN_POINT('Ctrl Pts',(1.35062987477783,6.63345193135305,150.73888566386));
#46541=CARTESIAN_POINT('Ctrl Pts',(1.16771959102951,6.66808192368238,150.747634908536));
#46542=CARTESIAN_POINT('Ctrl Pts',(0.983693746906821,6.69512028363169,150.756384153212));
#46543=CARTESIAN_POINT('Ctrl Pts',(0.799669205419827,6.72215845218868,150.765133335956));
#46544=CARTESIAN_POINT('Ctrl Pts',(0.614529402873411,6.7416050542458,150.773882518701));
#46545=CARTESIAN_POINT('Ctrl Pts',(0.428903127363162,6.75339404354123,150.782631701445));
#46546=CARTESIAN_POINT('Ctrl Pts',(0.243278104163796,6.7651829533033,150.791380825163));
#46547=CARTESIAN_POINT('Ctrl Pts',(0.0571669005390366,6.76931433552276,
150.800129948882));
#46548=CARTESIAN_POINT('Ctrl Pts',(-0.128798404777591,6.76577415902473,
150.808879072601));
#46549=CARTESIAN_POINT('Ctrl Pts',(-0.314762517259159,6.76223400523441,
150.8176281402));
#46550=CARTESIAN_POINT('Ctrl Pts',(-0.500580446819552,6.75102239665089,
150.826377207799));
#46551=CARTESIAN_POINT('Ctrl Pts',(-0.685621118842636,6.73217741012497,
150.835126275398));
#46552=CARTESIAN_POINT('Ctrl Pts',(-0.870660665414486,6.71333253821772,
150.843875289784));
#46553=CARTESIAN_POINT('Ctrl Pts',(-1.05492267885483,6.68685441030613,150.85262430417));
#46554=CARTESIAN_POINT('Ctrl Pts',(-1.23778137635246,6.65283295028178,150.861373318555));
#46555=CARTESIAN_POINT('Ctrl Pts',(-1.42999922978828,6.61707018861869,150.870570128923));
#46556=CARTESIAN_POINT('Ctrl Pts',(-1.62066601233663,6.5729717293442,150.87976693929));
#46557=CARTESIAN_POINT('Ctrl Pts',(-1.8090662850034,6.52070304311307,150.888963749658));
#46558=CARTESIAN_POINT('Ctrl Pts',(-1.98831342545485,6.47097374915044,150.897713747395));
#46559=CARTESIAN_POINT('Ctrl Pts',(-2.16550875896661,6.41384933989542,150.906463745133));
#46560=CARTESIAN_POINT('Ctrl Pts',(-2.34005036713973,6.3495238624049,150.915213742871));
#46561=CARTESIAN_POINT('Ctrl Pts',(-2.51458843547051,6.28519968948611,150.923963563152));
#46562=CARTESIAN_POINT('Ctrl Pts',(-2.68647261718019,6.21367483971115,150.932713383433));
#46563=CARTESIAN_POINT('Ctrl Pts',(-2.85511905908695,6.1351922674386,150.941463203714));
#46564=CARTESIAN_POINT('Ctrl Pts',(-3.02376230488844,6.05671118252957,150.950212858172));
#46565=CARTESIAN_POINT('Ctrl Pts',(-3.1891676737986,5.97127275992657,150.958962512631));
#46566=CARTESIAN_POINT('Ctrl Pts',(-3.35077334102739,5.87916720438024,150.967712167089));
#46567=CARTESIAN_POINT('Ctrl Pts',(-3.51237616037319,5.78706327195673,150.976461667358));
#46568=CARTESIAN_POINT('Ctrl Pts',(-3.6701791630225,5.68829258362331,150.985211167626));
#46569=CARTESIAN_POINT('Ctrl Pts',(-3.82364636566412,5.58319061741077,150.993960667894));
#46570=CARTESIAN_POINT('Ctrl Pts',(-3.97711106778755,5.47809036367733,151.002710025603));
#46571=CARTESIAN_POINT('Ctrl Pts',(-4.12623987481892,5.36665920043252,151.011459383311));
#46572=CARTESIAN_POINT('Ctrl Pts',(-4.27052628213902,5.24927559512357,151.02020874102));
#46573=CARTESIAN_POINT('Ctrl Pts',(-4.41481053024948,5.13189374643062,151.028957967796));
#46574=CARTESIAN_POINT('Ctrl Pts',(-4.55425230136499,5.00855981477382,151.037707194573));
#46575=CARTESIAN_POINT('Ctrl Pts',(-4.68837800630515,4.87969268192109,151.046456421349));
#46576=CARTESIAN_POINT('Ctrl Pts',(-4.82250188228878,4.75082730631827,151.05520552882));
#46577=CARTESIAN_POINT('Ctrl Pts',(-4.95130963052965,4.61642907903527,151.063954636291));
#46578=CARTESIAN_POINT('Ctrl Pts',(-5.07436379033381,4.47695444731674,151.072703743762));
#46579=CARTESIAN_POINT('Ctrl Pts',(-5.19741643562819,4.3374815322057,151.081452743552));
#46580=CARTESIAN_POINT('Ctrl Pts',(-5.31471544462785,4.19293255254574,151.090201743341));
#46581=CARTESIAN_POINT('Ctrl Pts',(-5.42586245275639,4.04379841779588,151.098950743131));
#46582=CARTESIAN_POINT('Ctrl Pts',(-5.53702160019166,3.89464799484325,151.107700698473));
#46583=CARTESIAN_POINT('Ctrl Pts',(-5.64202723081266,3.74091164443829,151.116450653815));
#46584=CARTESIAN_POINT('Ctrl Pts',(-5.74052265232982,3.58311159163208,151.125200609158));
#46585=CARTESIAN_POINT('Ctrl Pts',(-5.83901427066933,3.42531763191758,151.13395022664));
#46586=CARTESIAN_POINT('Ctrl Pts',(-5.93099603115754,3.26346052695587,151.142699844122));
#46587=CARTESIAN_POINT('Ctrl Pts',(-6.01615550622767,3.0980900446705,151.151449461605));
#46588=CARTESIAN_POINT('Ctrl Pts',(-6.10131214578814,2.93272506863797,151.160198787756));
#46589=CARTESIAN_POINT('Ctrl Pts',(-6.17964682328764,2.76384720416858,151.168948113907));
#46590=CARTESIAN_POINT('Ctrl Pts',(-6.25089348288581,2.59203002791552,151.177697440058));
#46591=CARTESIAN_POINT('Ctrl Pts',(-6.32213814889342,2.42021765936998,151.18644652139));
#46592=CARTESIAN_POINT('Ctrl Pts',(-6.38629508412592,2.24546640831898,151.195195602721));
#46593=CARTESIAN_POINT('Ctrl Pts',(-6.44314639819815,2.06836976660032,151.203944684053));
#46594=CARTESIAN_POINT('Ctrl Pts',(-6.50000285283702,1.89125711158269,151.212694556487));
#46595=CARTESIAN_POINT('Ctrl Pts',(-6.5495522767325,1.7117989144025,151.221444428922));
#46596=CARTESIAN_POINT('Ctrl Pts',(-6.59162635926386,1.53060476278429,151.230194301356));
#46597=CARTESIAN_POINT('Ctrl Pts',(-6.63369752055195,1.34942319164703,151.238943566279));
#46598=CARTESIAN_POINT('Ctrl Pts',(-6.66829431424251,1.16650618642721,151.247692831201));
#46599=CARTESIAN_POINT('Ctrl Pts',(-6.69529923745413,0.982474997618827,
151.256442096124));
#46600=CARTESIAN_POINT('Ctrl Pts',(-6.7223055473144,0.798434359178024,151.265191810303));
#46601=CARTESIAN_POINT('Ctrl Pts',(-6.741719164967,0.61327970624063,151.273941524483));
#46602=CARTESIAN_POINT('Ctrl Pts',(-6.75347414817273,0.427639953655683,
151.282691238663));
#46603=CARTESIAN_POINT('Ctrl Pts',(-6.76248837758728,0.285283364201305,
151.289400897838));
#46604=CARTESIAN_POINT('Ctrl Pts',(-6.76699999999981,0.142641701110285,
151.296110557014));
#46605=CARTESIAN_POINT('Ctrl Pts',(-6.767,9.16835937808996E-12,151.30282021619));
#46606=CARTESIAN_POINT('Ctrl Pts',(-6.76699999999368,9.25253348153785E-6,
151.303021482695));
#46607=CARTESIAN_POINT('Ctrl Pts',(-6.76700023307113,-0.170455966723974,
151.311077178856));
#46608=CARTESIAN_POINT('Ctrl Pts',(-6.7605549706658,-0.341193029931809,
151.319132875017));
#46609=CARTESIAN_POINT('Ctrl Pts',(-6.74762845049654,-0.511663262360731,
151.327188571179));
#46610=CARTESIAN_POINT('Ctrl Pts',(-6.73471557880108,-0.681953503696206,
151.335235761728));
#46611=CARTESIAN_POINT('Ctrl Pts',(-6.7153350949022,-0.851977105275738,
151.343282952278));
#46612=CARTESIAN_POINT('Ctrl Pts',(-6.68950320557243,-1.02119335222872,
151.351330142828));
#46613=CARTESIAN_POINT('Ctrl Pts',(-6.66369290553083,-1.19026817482549,
151.359370607848));
#46614=CARTESIAN_POINT('Ctrl Pts',(-6.63144198725326,-1.35853661800618,
151.367411072869));
#46615=CARTESIAN_POINT('Ctrl Pts',(-6.59281860865363,-1.52546117400293,
151.37545153789));
#46616=CARTESIAN_POINT('Ctrl Pts',(-6.55421901968788,-1.69228291470446,
151.383487050477));
#46617=CARTESIAN_POINT('Ctrl Pts',(-6.50925486776001,-1.85776205259014,
151.391522563065));
#46618=CARTESIAN_POINT('Ctrl Pts',(-6.45804570416447,-2.02136950677575,
151.399558075652));
#46619=CARTESIAN_POINT('Ctrl Pts',(-6.40685048307061,-2.18493241625405,
151.407591400444));
#46620=CARTESIAN_POINT('Ctrl Pts',(-6.34941374018606,-2.34662429780411,
151.415624725237));
#46621=CARTESIAN_POINT('Ctrl Pts',(-6.28590539453114,-2.5059294425431,151.423658050029));
#46622=CARTESIAN_POINT('Ctrl Pts',(-6.22240468799061,-2.66521542523004,
151.431690408531));
#46623=CARTESIAN_POINT('Ctrl Pts',(-6.15283396955282,-2.82211489426953,
151.439722767033));
#46624=CARTESIAN_POINT('Ctrl Pts',(-6.07741190738215,-2.97613062683909,
151.447755125536));
#46625=CARTESIAN_POINT('Ctrl Pts',(-6.00198391720787,-3.13015846469711,
151.455788115363));
#46626=CARTESIAN_POINT('Ctrl Pts',(-5.92070383231666,-3.28130177849347,
151.46382110519));
#46627=CARTESIAN_POINT('Ctrl Pts',(-5.83383695003169,-3.42908667730126,
151.471854095018));
#46628=CARTESIAN_POINT('Ctrl Pts',(-5.74694596005494,-3.57691259004551,
151.479889314197));
#46629=CARTESIAN_POINT('Ctrl Pts',(-5.65446527656626,-3.72137791018506,
151.487924533376));
#46630=CARTESIAN_POINT('Ctrl Pts',(-5.55670421255499,-3.86203667695863,
151.495959752556));
#46631=CARTESIAN_POINT('Ctrl Pts',(-5.4588363892755,-4.0028490491288,151.504003746538));
#46632=CARTESIAN_POINT('Ctrl Pts',(-5.35567688177833,-4.13984625728533,
151.512047740521));
#46633=CARTESIAN_POINT('Ctrl Pts',(-5.24757659962024,-4.2726138172222,151.520091734503));
#46634=CARTESIAN_POINT('Ctrl Pts',(-5.13941661942993,-4.40545469761589,
151.528140170756));
#46635=CARTESIAN_POINT('Ctrl Pts',(-5.02631067726316,-4.53406099736127,
151.536188607008));
#46636=CARTESIAN_POINT('Ctrl Pts',(-4.90864705673056,-4.6580546446398,151.544237043261));
#46637=CARTESIAN_POINT('Ctrl Pts',(-4.79079680301249,-4.78224496553134,
151.552298245611));
#46638=CARTESIAN_POINT('Ctrl Pts',(-4.66837469570844,-4.90180775598046,
151.560359447961));
#46639=CARTESIAN_POINT('Ctrl Pts',(-4.54180352305622,-5.01640406645578,
151.568420650312));
#46640=CARTESIAN_POINT('Ctrl Pts',(-4.41788460963826,-5.12859904717882,
151.576312932694));
#46641=CARTESIAN_POINT('Ctrl Pts',(-4.28998908925523,-5.23603348263788,
151.584205215077));
#46642=CARTESIAN_POINT('Ctrl Pts',(-4.15853970958954,-5.33843015162388,
151.59209749746));
#46643=CARTESIAN_POINT('Ctrl Pts',(-4.02143734872161,-5.44523038985015,
151.600329187484));
#46644=CARTESIAN_POINT('Ctrl Pts',(-3.88001749945412,-5.5469018433012,151.608560877509));
#46645=CARTESIAN_POINT('Ctrl Pts',(-3.73469941990389,-5.64307622161615,
151.616792567533));
#46646=CARTESIAN_POINT('Ctrl Pts',(-3.58955421119695,-5.73913619058896,
151.625014465113));
#46647=CARTESIAN_POINT('Ctrl Pts',(-3.44052030213288,-5.82971190998977,
151.633236362693));
#46648=CARTESIAN_POINT('Ctrl Pts',(-3.28805023937711,-5.91447500826,151.641458260274));
#46649=CARTESIAN_POINT('Ctrl Pts',(-3.1357310102289,-5.99915425319096,151.649672024201));
#46650=CARTESIAN_POINT('Ctrl Pts',(-2.97998270806837,-6.07803215569456,
151.657885788129));
#46651=CARTESIAN_POINT('Ctrl Pts',(-2.82128717941016,-6.15082333117249,
151.666099552057));
#46652=CARTESIAN_POINT('Ctrl Pts',(-2.66271686202538,-6.22355707418303,
151.674306835299));
#46653=CARTESIAN_POINT('Ctrl Pts',(-2.5012042740145,-6.29021350692185,151.682514118542));
#46654=CARTESIAN_POINT('Ctrl Pts',(-2.33725628959949,-6.3505528922077,151.690721401784));
#46655=CARTESIAN_POINT('Ctrl Pts',(-2.17340483629631,-6.41085675020136,
151.698923852651));
#46656=CARTESIAN_POINT('Ctrl Pts',(-2.00712117853895,-6.46485084687705,
151.707126303518));
#46657=CARTESIAN_POINT('Ctrl Pts',(-1.8389327045801,-6.51234331926886,151.715328754385));
#46658=CARTESIAN_POINT('Ctrl Pts',(-1.67079343048949,-6.55982189877414,
151.723528805804));
#46659=CARTESIAN_POINT('Ctrl Pts',(-1.50075079345592,-6.60080254146056,
151.731728857223));
#46660=CARTESIAN_POINT('Ctrl Pts',(-1.32934814206397,-6.6351429914653,151.739928908642));
#46661=CARTESIAN_POINT('Ctrl Pts',(-1.15796877252919,-6.66947877695963,
151.748127846236));
#46662=CARTESIAN_POINT('Ctrl Pts',(-0.985230107706917,-6.69717609494801,
151.756326783831));
#46663=CARTESIAN_POINT('Ctrl Pts',(-0.811686528474478,-6.71814364087975,
151.764525721426));
#46664=CARTESIAN_POINT('Ctrl Pts',(-0.638135043440735,-6.7391121419909,
151.772725032524));
#46665=CARTESIAN_POINT('Ctrl Pts',(-0.463778926784342,-6.75335021722072,
151.780924343623));
#46666=CARTESIAN_POINT('Ctrl Pts',(-0.289178593508561,-6.76081834847354,
151.789123654721));
#46667=CARTESIAN_POINT('Ctrl Pts',(-0.114538636257731,-6.76828817455156,
151.797324826579));
#46668=CARTESIAN_POINT('Ctrl Pts',(0.06034528998886,-6.76898498131176,151.805525998438));
#46669=CARTESIAN_POINT('Ctrl Pts',(0.234911792673331,-6.76292136947215,
151.813727170296));
#46670=CARTESIAN_POINT('Ctrl Pts',(0.409642357685587,-6.75685205888588,
151.821936049838));
#46671=CARTESIAN_POINT('Ctrl Pts',(0.584054544452102,-6.74400964817368,
151.83014492938));
#46672=CARTESIAN_POINT('Ctrl Pts',(0.757590160048227,-6.72445879973981,
151.838353808921));
#46673=CARTESIAN_POINT('Ctrl Pts',(0.93120923168094,-6.70489854899208,151.846566636244));
#46674=CARTESIAN_POINT('Ctrl Pts',(1.10395053750502,-6.67862348196518,151.854779463566));
#46675=CARTESIAN_POINT('Ctrl Pts',(1.27526519165629,-6.64574959586576,151.862992290889));
#46676=CARTESIAN_POINT('Ctrl Pts',(1.44681431562433,-6.61283071691918,151.871216358698));
#46677=CARTESIAN_POINT('Ctrl Pts',(1.61693253645797,-6.57329505057456,151.879440426508));
#46678=CARTESIAN_POINT('Ctrl Pts',(1.78508407526776,-6.52730908140755,151.887664494317));
#46679=CARTESIAN_POINT('Ctrl Pts',(1.93663282517774,-6.48586363172575,151.895076541834));
#46680=CARTESIAN_POINT('Ctrl Pts',(2.08658411908769,-6.43917948131312,151.902488589351));
#46681=CARTESIAN_POINT('Ctrl Pts',(2.23455979943223,-6.38741195655654,151.909900636867));
#46682=CARTESIAN_POINT('Ctrl Pts',(2.40712446113371,-6.32704227029496,151.918544337435));
#46683=CARTESIAN_POINT('Ctrl Pts',(2.57739622972982,-6.25962118194966,151.927188038003));
#46684=CARTESIAN_POINT('Ctrl Pts',(2.74479281837802,-6.18533761278885,151.935831738571));
#46685=CARTESIAN_POINT('Ctrl Pts',(2.91197428131449,-6.11114950737562,151.944464330895));
#46686=CARTESIAN_POINT('Ctrl Pts',(3.07628765451557,-6.03011663009837,151.953096923219));
#46687=CARTESIAN_POINT('Ctrl Pts',(3.23716825738057,-5.94247681303071,151.961729515542));
#46688=CARTESIAN_POINT('Ctrl Pts',(3.40345588027828,-5.85189151814839,151.970652239794));
#46689=CARTESIAN_POINT('Ctrl Pts',(3.56607566392043,-5.75424753404614,151.979574964047));
#46690=CARTESIAN_POINT('Ctrl Pts',(3.72442631529256,-5.64986173476452,151.988497688299));
#46691=CARTESIAN_POINT('Ctrl Pts',(3.87720327285403,-5.5491501513976,151.997106346695));
#46692=CARTESIAN_POINT('Ctrl Pts',(4.02600619613065,-5.4421634199807,152.005715005091));
#46693=CARTESIAN_POINT('Ctrl Pts',(4.17031943446256,-5.32923304186858,152.014323663487));
#46694=CARTESIAN_POINT('Ctrl Pts',(4.31449624953625,-5.21640941993707,152.022924183882));
#46695=CARTESIAN_POINT('Ctrl Pts',(4.45419160182225,-5.09765354092595,152.031524704278));
#46696=CARTESIAN_POINT('Ctrl Pts',(4.58891927497414,-4.97333981221581,152.040125224673));
#46697=CARTESIAN_POINT('Ctrl Pts',(4.72349583075759,-4.84916552006763,152.04871609829));
#46698=CARTESIAN_POINT('Ctrl Pts',(4.8531155994263,-4.71944602131146,152.057306971907));
#46699=CARTESIAN_POINT('Ctrl Pts',(4.97732572854776,-4.58459568467456,152.065897845524));
#46700=CARTESIAN_POINT('Ctrl Pts',(4.99132318199891,-4.56939916790657,152.066865965873));
#46701=CARTESIAN_POINT('Ctrl Pts',(5.00525197158645,-4.55413753382398,152.067834086222));
#46702=CARTESIAN_POINT('Ctrl Pts',(5.01911147663452,-4.53881140664774,152.068802206571));
#46703=CARTESIAN_POINT('Ctrl Pts',(5.14232916496506,-4.40255473982118,152.077409263679));
#46704=CARTESIAN_POINT('Ctrl Pts',(5.25992018472983,-4.26136041845833,152.086016320786));
#46705=CARTESIAN_POINT('Ctrl Pts',(5.37151197477263,-4.11571963390052,152.094623377894));
#46706=CARTESIAN_POINT('Ctrl Pts',(5.48321209879413,-3.96993746039604,152.103238790784));
#46707=CARTESIAN_POINT('Ctrl Pts',(5.58890118275948,-3.81970044793657,152.111854203674));
#46708=CARTESIAN_POINT('Ctrl Pts',(5.68824976275295,-3.66552910731057,152.120469616565));
#46709=CARTESIAN_POINT('Ctrl Pts',(5.79129726639236,-3.5056176945325,152.129405796541));
#46710=CARTESIAN_POINT('Ctrl Pts',(5.8875228850268,-3.34147368997647,152.138341976516));
#46711=CARTESIAN_POINT('Ctrl Pts',(5.97661157035904,-3.17370495431609,152.147278156492));
#46712=CARTESIAN_POINT('Ctrl Pts',(6.06274189604705,-3.01150729937476,152.155917593575));
#46713=CARTESIAN_POINT('Ctrl Pts',(6.14220158827863,-2.84592206877392,152.164557030658));
#46714=CARTESIAN_POINT('Ctrl Pts',(6.21475528363058,-2.67751858342492,152.173196467741));
#46715=CARTESIAN_POINT('Ctrl Pts',(6.2910470338892,-2.50043874504311,152.182281019163));
#46716=CARTESIAN_POINT('Ctrl Pts',(6.35970227598654,-2.32024297721477,152.191365570586));
#46717=CARTESIAN_POINT('Ctrl Pts',(6.42050674934671,-2.13761130273804,152.200450122008));
#46718=CARTESIAN_POINT('Ctrl Pts',(6.48131122270687,-1.95497962826131,152.20953467343));
#46719=CARTESIAN_POINT('Ctrl Pts',(6.5342648734388,-1.76991243252498,152.218619224853));
#46720=CARTESIAN_POINT('Ctrl Pts',(6.57921538620068,-1.58310261890388,152.227703776275));
#46721=CARTESIAN_POINT('Ctrl Pts',(6.61984056596085,-1.41426845455237,152.235914172818));
#46722=CARTESIAN_POINT('Ctrl Pts',(6.6540176064454,-1.24364128244219,152.24412456936));
#46723=CARTESIAN_POINT('Ctrl Pts',(6.68158884294507,-1.07175535166938,152.252334965903));
#46724=CARTESIAN_POINT('Ctrl Pts',(6.70913081273306,-0.900051876840416,
152.260536647156));
#46725=CARTESIAN_POINT('Ctrl Pts',(6.7300808845267,-0.727092656219492,152.268738328409));
#46726=CARTESIAN_POINT('Ctrl Pts',(6.74433165425905,-0.553425277123611,
152.276940009663));
#46727=CARTESIAN_POINT('Ctrl Pts',(6.75857018037254,-0.379907105210154,
152.285134644401));
#46728=CARTESIAN_POINT('Ctrl Pts',(6.76612083765613,-0.205682343029822,
152.293329279139));
#46729=CARTESIAN_POINT('Ctrl Pts',(6.76692757997545,-0.0313069859245526,
152.301523913878));
#46730=CARTESIAN_POINT('Ctrl Pts',(6.76773379236648,0.142953828495147,152.309713165771));
#46731=CARTESIAN_POINT('Ctrl Pts',(6.76180491155083,0.317364682295511,152.317902417665));
#46732=CARTESIAN_POINT('Ctrl Pts',(6.74913685369885,0.491366187322597,152.326091669559));
#46733=CARTESIAN_POINT('Ctrl Pts',(6.73647455518912,0.665288585178814,152.334277198332));
#46734=CARTESIAN_POINT('Ctrl Pts',(6.71707920940525,0.838801646880461,152.342462727106));
#46735=CARTESIAN_POINT('Ctrl Pts',(6.69099880037581,1.01134764219304,152.350648255879));
#46736=CARTESIAN_POINT('Ctrl Pts',(6.66492049002162,1.18387975283048,152.358833125967));
#46737=CARTESIAN_POINT('Ctrl Pts',(6.63215823275973,1.35544459521934,152.367017996056));
#46738=CARTESIAN_POINT('Ctrl Pts',(6.59281174209825,1.52549084994028,152.375202866145));
#46739=CARTESIAN_POINT('Ctrl Pts',(6.55346549401829,1.69553605628104,152.383387685771));
#46740=CARTESIAN_POINT('Ctrl Pts',(6.50753517343739,1.86406234266953,152.391572505398));
#46741=CARTESIAN_POINT('Ctrl Pts',(6.45517133322181,2.03052999454611,152.399757325025));
#46742=CARTESIAN_POINT('Ctrl Pts',(6.40279822069086,2.19702712364512,152.407943593977));
#46743=CARTESIAN_POINT('Ctrl Pts',(6.34398942696614,2.36146454864155,152.416129862929));
#46744=CARTESIAN_POINT('Ctrl Pts',(6.27894496928143,2.52331905884599,152.42431613188));
#46745=CARTESIAN_POINT('Ctrl Pts',(6.21387707493509,2.68523188807598,152.432505350489));
#46746=CARTESIAN_POINT('Ctrl Pts',(6.1425691752523,2.84455961492315,152.440694569097));
#46747=CARTESIAN_POINT('Ctrl Pts',(6.0652688930922,3.00080026900961,152.448883787706));
#46748=CARTESIAN_POINT('Ctrl Pts',(5.98787905783168,3.15722192935625,152.457082493601));
#46749=CARTESIAN_POINT('Ctrl Pts',(5.90448313068335,3.31054904906628,152.465281199496));
#46750=CARTESIAN_POINT('Ctrl Pts',(5.81537457033345,3.46030455404131,152.47347990539));
#46751=CARTESIAN_POINT('Ctrl Pts',(5.72621270366357,3.61014964541337,152.481683515897));
#46752=CARTESIAN_POINT('Ctrl Pts',(5.63133158775056,3.75641856193982,152.489887126403));
#46753=CARTESIAN_POINT('Ctrl Pts',(5.53106716917532,3.89866451109492,152.498090736909));
#46754=CARTESIAN_POINT('Ctrl Pts',(5.43064447048977,4.04113501353463,152.506307297855));
#46755=CARTESIAN_POINT('Ctrl Pts',(5.32482170495855,4.17956957168957,152.514523858802));
#46756=CARTESIAN_POINT('Ctrl Pts',(5.21397499711123,4.31355465127068,152.522740419748));
#46757=CARTESIAN_POINT('Ctrl Pts',(5.11159675800477,4.43730353637919,152.530329251726));
#46758=CARTESIAN_POINT('Ctrl Pts',(5.00493346792305,4.55725707086845,152.537918083705));
#46759=CARTESIAN_POINT('Ctrl Pts',(4.89430773789984,4.67311895490942,152.545506915683));
#46760=CARTESIAN_POINT('Ctrl Pts',(4.77510884212814,4.79795979109479,152.553683859617));
#46761=CARTESIAN_POINT('Ctrl Pts',(4.65093988341982,4.9184364187114,152.56186080355));
#46762=CARTESIAN_POINT('Ctrl Pts',(4.52215398777142,5.03412478102034,152.570037747484));
#46763=CARTESIAN_POINT('Ctrl Pts',(4.39356713560064,5.14963434258532,152.578202053641));
#46764=CARTESIAN_POINT('Ctrl Pts',(4.26037783138535,5.26037014250751,152.586366359798));
#46765=CARTESIAN_POINT('Ctrl Pts',(4.12297796141772,5.36594276242897,152.594530665956));
#46766=CARTESIAN_POINT('Ctrl Pts',(3.98570080863105,5.47142109132739,152.602687680253));
#46767=CARTESIAN_POINT('Ctrl Pts',(3.84422085959967,5.57174519650159,152.61084469455));
#46768=CARTESIAN_POINT('Ctrl Pts',(3.69896574212059,5.66656345933038,152.619001708847));
#46769=CARTESIAN_POINT('Ctrl Pts',(3.55383767118573,5.76129878991671,152.627151588658));
#46770=CARTESIAN_POINT('Ctrl Pts',(3.40494131244847,5.85053767288747,152.63530146847));
#46771=CARTESIAN_POINT('Ctrl Pts',(3.25273593142272,5.93396983143929,152.643451348282));
#46772=CARTESIAN_POINT('Ctrl Pts',(3.20191196779873,5.96182924720193,152.646172731668));
#46773=CARTESIAN_POINT('Ctrl Pts',(3.15071929826171,5.9890415589112,152.648894115053));
#46774=CARTESIAN_POINT('Ctrl Pts',(3.0991757505326,6.01559628526638,152.651615498439));
#46775=CARTESIAN_POINT('Origin',(0.,0.,-3.69717978381041));
#46776=CARTESIAN_POINT('',(-6.76724014394675,0.000669971015295954,153.303235821163));
#46777=CARTESIAN_POINT('Ctrl Pts',(3.0991757505326,6.01559628526638,152.651615498439));
#46778=CARTESIAN_POINT('Ctrl Pts',(2.94492830563623,6.09506304435979,152.659759416587));
#46779=CARTESIAN_POINT('Ctrl Pts',(2.78753676423252,6.16863743062611,152.667903334736));
#46780=CARTESIAN_POINT('Ctrl Pts',(2.62749618569209,6.2360686970377,152.676047252884));
#46781=CARTESIAN_POINT('Ctrl Pts',(2.46748507374941,6.30348754803553,152.684189671578));
#46782=CARTESIAN_POINT('Ctrl Pts',(2.30482622857547,6.36476538464918,152.692332090272));
#46783=CARTESIAN_POINT('Ctrl Pts',(2.14003647277271,6.41969881654915,152.700474508966));
#46784=CARTESIAN_POINT('Ctrl Pts',(1.9752567367852,6.47462890829708,152.708616432572));
#46785=CARTESIAN_POINT('Ctrl Pts',(1.80834669322798,6.52321524757542,152.716758356177));
#46786=CARTESIAN_POINT('Ctrl Pts',(1.63984005988312,6.56530376890533,152.724900279783));
#46787=CARTESIAN_POINT('Ctrl Pts',(1.47131194816819,6.6073976549667,152.733043241182));
#46788=CARTESIAN_POINT('Ctrl Pts',(1.30118719458042,6.64299198541091,152.741186202582));
#46789=CARTESIAN_POINT('Ctrl Pts',(1.13001146939226,6.67198344415227,152.749329163982));
#46790=CARTESIAN_POINT('Ctrl Pts',(0.958781697811568,6.70098405654995,152.757474696411));
#46791=CARTESIAN_POINT('Ctrl Pts',(0.786500652576645,6.72337758510041,152.765620228839));
#46792=CARTESIAN_POINT('Ctrl Pts',(0.61372089513729,6.73911237945116,152.773765761268));
#46793=CARTESIAN_POINT('Ctrl Pts',(0.440760318609443,6.75486364072613,152.781919818235));
#46794=CARTESIAN_POINT('Ctrl Pts',(0.267300350225355,6.76394221637646,152.790073875202));
#46795=CARTESIAN_POINT('Ctrl Pts',(0.0938962172301893,6.76634853524335,
152.79822793217));
#46796=CARTESIAN_POINT('Ctrl Pts',(-0.0796068153495014,6.76875622653391,
152.806386639735));
#46797=CARTESIAN_POINT('Ctrl Pts',(-0.253053585947054,6.76448408648889,
152.814545347299));
#46798=CARTESIAN_POINT('Ctrl Pts',(-0.425892454205106,6.75358457542742,
152.822704054864));
#46799=CARTESIAN_POINT('Ctrl Pts',(-0.598973669275219,6.74266978156651,
152.830874202199));
#46800=CARTESIAN_POINT('Ctrl Pts',(-0.771444917987083,6.72510909096235,
152.839044349533));
#46801=CARTESIAN_POINT('Ctrl Pts',(-0.942762205668032,6.70100652316978,
152.847214496867));
#46802=CARTESIAN_POINT('Ctrl Pts',(-1.05526312990229,6.68517880846691,152.852579682942));
#46803=CARTESIAN_POINT('Ctrl Pts',(-1.16726664649183,6.66653108608735,152.857944869016));
#46804=CARTESIAN_POINT('Ctrl Pts',(-1.27862215391275,6.64510454300935,152.863310055091));
#46805=CARTESIAN_POINT('Ctrl Pts',(-1.44960357757298,6.61220504010695,152.87154805943));
#46806=CARTESIAN_POINT('Ctrl Pts',(-1.61954544372369,6.57265771547668,152.879786063768));
#46807=CARTESIAN_POINT('Ctrl Pts',(-1.78789346599803,6.5265401212466,152.888024068107));
#46808=CARTESIAN_POINT('Ctrl Pts',(-1.95605633052642,6.4804732495001,152.896253011868));
#46809=CARTESIAN_POINT('Ctrl Pts',(-2.12262850043843,6.42785059227623,152.904481955629));
#46810=CARTESIAN_POINT('Ctrl Pts',(-2.28706429538294,6.36880097889583,152.91271089939));
#46811=CARTESIAN_POINT('Ctrl Pts',(-2.45135192060478,6.3098045739111,152.920932428218));
#46812=CARTESIAN_POINT('Ctrl Pts',(-2.61350667061379,6.24439286696381,152.929153957047));
#46813=CARTESIAN_POINT('Ctrl Pts',(-2.77299638335608,6.17274493705143,152.937375485875));
#46814=CARTESIAN_POINT('Ctrl Pts',(-2.93237407528811,6.10114733050489,152.945591240147));
#46815=CARTESIAN_POINT('Ctrl Pts',(-3.08909013388998,6.02332237190325,152.95380699442));
#46816=CARTESIAN_POINT('Ctrl Pts',(-3.24263070343066,5.93949788460008,152.962022748692));
#46817=CARTESIAN_POINT('Ctrl Pts',(-3.39609393362528,5.85571562021592,152.970234364637));
#46818=CARTESIAN_POINT('Ctrl Pts',(-3.54638454856016,5.76594001872067,152.978445980583));
#46819=CARTESIAN_POINT('Ctrl Pts',(-3.69301161604868,5.67044567946202,152.986657596528));
#46820=CARTESIAN_POINT('Ctrl Pts',(-3.83961411264868,5.5749673425746,152.99486783642));
#46821=CARTESIAN_POINT('Ctrl Pts',(-3.98255398204806,5.47377236626722,153.003078076312));
#46822=CARTESIAN_POINT('Ctrl Pts',(-4.12136742791459,5.36717984831184,153.011288316203));
#46823=CARTESIAN_POINT('Ctrl Pts',(-4.26017257550486,5.26059370246369,153.019498065287));
#46824=CARTESIAN_POINT('Ctrl Pts',(-4.39485150688813,5.14861087458011,153.02770781437));
#46825=CARTESIAN_POINT('Ctrl Pts',(-4.52497185228122,5.03159206773191,153.035917563453));
#46826=CARTESIAN_POINT('Ctrl Pts',(-4.65510784230526,4.9145591914771,153.044128299611));
#46827=CARTESIAN_POINT('Ctrl Pts',(-4.78068388857562,4.79248936891971,153.052339035768));
#46828=CARTESIAN_POINT('Ctrl Pts',(-4.90130292896311,4.66578167068902,153.060549771926));
#46829=CARTESIAN_POINT('Ctrl Pts',(-5.02195818455962,4.53903592916301,153.068762973313));
#46830=CARTESIAN_POINT('Ctrl Pts',(-5.13765322320199,4.40764979685971,153.076976174699));
#46831=CARTESIAN_POINT('Ctrl Pts',(-5.24802983011563,4.27205710427852,153.085189376086));
#46832=CARTESIAN_POINT('Ctrl Pts',(-5.35852196341923,4.1363224927281,153.093411173873));
#46833=CARTESIAN_POINT('Ctrl Pts',(-5.4636843178522,3.99637280217192,153.10163297166));
#46834=CARTESIAN_POINT('Ctrl Pts',(-5.56320016391786,3.85267347905118,153.109854769447));
#46835=CARTESIAN_POINT('Ctrl Pts',(-5.66276990172245,3.70889633710346,153.11808101966));
#46836=CARTESIAN_POINT('Ctrl Pts',(-5.75668684323546,3.56136581550566,153.126307269874));
#46837=CARTESIAN_POINT('Ctrl Pts',(-5.84467922020521,3.41057382457871,153.134533520087));
#46838=CARTESIAN_POINT('Ctrl Pts',(-5.93279963002372,3.25956242455254,153.142771739863));
#46839=CARTESIAN_POINT('Ctrl Pts',(-6.01497807970119,3.10528038679674,153.151009959638));
#46840=CARTESIAN_POINT('Ctrl Pts',(-6.09098957038893,2.94824270598831,153.159248179414));
#46841=CARTESIAN_POINT('Ctrl Pts',(-6.15823680080461,2.80931174950108,153.166536517775));
#46842=CARTESIAN_POINT('Ctrl Pts',(-6.22065785029642,2.66822442975674,153.173824856137));
#46843=CARTESIAN_POINT('Ctrl Pts',(-6.2781292976951,2.52534780207054,153.181113194498));
#46844=CARTESIAN_POINT('Ctrl Pts',(-6.3504164459868,2.34563866926717,153.190280410912));
#46845=CARTESIAN_POINT('Ctrl Pts',(-6.41505133711675,2.16265535962499,153.199447627326));
#46846=CARTESIAN_POINT('Ctrl Pts',(-6.47175761011487,1.9770286886943,153.20861484374));
#46847=CARTESIAN_POINT('Ctrl Pts',(-6.52820740822629,1.79224158236338,153.21774059806));
#46848=CARTESIAN_POINT('Ctrl Pts',(-6.57680004080532,1.60483515921502,153.22686635238));
#46849=CARTESIAN_POINT('Ctrl Pts',(-6.61730875284526,1.41545535765617,153.235992106701));
#46850=CARTESIAN_POINT('Ctrl Pts',(-6.65769786423432,1.22663469378369,153.245090917529));
#46851=CARTESIAN_POINT('Ctrl Pts',(-6.69005060763174,1.03585247477288,153.254189728358));
#46852=CARTESIAN_POINT('Ctrl Pts',(-6.71418957826771,0.843769700262641,
153.263288539186));
#46853=CARTESIAN_POINT('Ctrl Pts',(-6.73821397325754,0.652598646816766,
153.272344162501));
#46854=CARTESIAN_POINT('Ctrl Pts',(-6.75410229271552,0.460139554458451,
153.281399785815));
#46855=CARTESIAN_POINT('Ctrl Pts',(-6.76172810895751,0.267061754158045,
153.29045540913));
#46856=CARTESIAN_POINT('Ctrl Pts',(-6.76519894482116,0.179183770675106,
153.294577011483));
#46857=CARTESIAN_POINT('Ctrl Pts',(-6.76695883519318,0.0911778433954226,
153.298698613836));
#46858=CARTESIAN_POINT('Ctrl Pts',(-6.76699928620785,0.00310812845892864,
153.302820216189));
#46859=CARTESIAN_POINT('',(3.92888236737299,-5.50964357679747,154.));
#46860=CARTESIAN_POINT('Ctrl Pts',(-6.767,9.31121846292626E-12,153.30282021619));
#46861=CARTESIAN_POINT('Ctrl Pts',(-6.76700000000026,-0.186008656853188,
153.3115697942));
#46862=CARTESIAN_POINT('Ctrl Pts',(-6.75932625676188,-0.37201717040645,
153.32031937221));
#46863=CARTESIAN_POINT('Ctrl Pts',(-6.7440048348797,-0.557393745138262,
153.329068950221));
#46864=CARTESIAN_POINT('Ctrl Pts',(-6.72868354559113,-0.742768715596703,
153.337818452511));
#46865=CARTESIAN_POINT('Ctrl Pts',(-6.70571473370896,-0.927511472541724,
153.346567954801));
#46866=CARTESIAN_POINT('Ctrl Pts',(-6.67517641362661,-1.11099453057292,
153.355317457091));
#46867=CARTESIAN_POINT('Ctrl Pts',(-6.64463834768126,-1.29447606167556,
153.364066886569));
#46868=CARTESIAN_POINT('Ctrl Pts',(-6.60653094664505,-1.47669763213353,
153.372816316047));
#46869=CARTESIAN_POINT('Ctrl Pts',(-6.56098364152038,-1.65704033013745,
153.381565745524));
#46870=CARTESIAN_POINT('Ctrl Pts',(-6.51543670030484,-1.83738158725801,
153.390315105097));
#46871=CARTESIAN_POINT('Ctrl Pts',(-6.46245004412932,-2.01584372410336,
153.399064464669));
#46872=CARTESIAN_POINT('Ctrl Pts',(-6.40220363820689,-2.19182060737882,
153.407813824241));
#46873=CARTESIAN_POINT('Ctrl Pts',(-6.34195769362181,-2.36779614310984,
153.416563116816));
#46874=CARTESIAN_POINT('Ctrl Pts',(-6.27445220335668,-2.54128619222773,
153.42531240939));
#46875=CARTESIAN_POINT('Ctrl Pts',(-6.19991644125039,-2.71170151777682,
153.434061701964));
#46876=CARTESIAN_POINT('Ctrl Pts',(-6.12538122514392,-2.88211559497567,
153.442810930446));
#46877=CARTESIAN_POINT('Ctrl Pts',(-6.04381595508577,-3.04945473112789,
153.451560158929));
#46878=CARTESIAN_POINT('Ctrl Pts',(-5.95549765311986,-3.213150588392,153.460309387411));
#46879=CARTESIAN_POINT('Ctrl Pts',(-5.86717996878046,-3.37684530090017,
153.469058554709));
#46880=CARTESIAN_POINT('Ctrl Pts',(-5.77210948310036,-3.53689653331464,
153.477807722007));
#46881=CARTESIAN_POINT('Ctrl Pts',(-5.67060908169332,-3.69276070746769,
153.486556889304));
#46882=CARTESIAN_POINT('Ctrl Pts',(-5.5691093563862,-3.84862384340065,153.495305998323));
#46883=CARTESIAN_POINT('Ctrl Pts',(-5.46117995742809,-4.00029973676548,
153.504055107342));
#46884=CARTESIAN_POINT('Ctrl Pts',(-5.34718743797362,-4.14727326121358,
153.512804216361));
#46885=CARTESIAN_POINT('Ctrl Pts',(-5.23319563997062,-4.2942458554755,153.521553270007));
#46886=CARTESIAN_POINT('Ctrl Pts',(-5.11314097386879,-4.43651591395998,
153.530302323653));
#46887=CARTESIAN_POINT('Ctrl Pts',(-4.98743116787335,-4.57360026081483,
153.5390513773));
#46888=CARTESIAN_POINT('Ctrl Pts',(-4.86172211573906,-4.71068378559727,
153.547800378479));
#46889=CARTESIAN_POINT('Ctrl Pts',(-4.73035818522944,-4.84258144980424,
153.556549379659));
#46890=CARTESIAN_POINT('Ctrl Pts',(-4.5937855075914,-4.96884530955063,153.565298380838));
#46891=CARTESIAN_POINT('Ctrl Pts',(-4.45241612228613,-5.09954381050499,
153.574354664571));
#46892=CARTESIAN_POINT('Ctrl Pts',(-4.30546569332165,-5.22420535248028,
153.583410948304));
#46893=CARTESIAN_POINT('Ctrl Pts',(-4.15346891903191,-5.34237633816974,
153.592467232036));
#46894=CARTESIAN_POINT('Ctrl Pts',(-4.00661345260036,-5.45655017707648,
153.60121718596));
#46895=CARTESIAN_POINT('Ctrl Pts',(-3.85504768195733,-5.56466517980614,
153.609967139885));
#46896=CARTESIAN_POINT('Ctrl Pts',(-3.69928645877247,-5.66635409200155,
153.618717093809));
#46897=CARTESIAN_POINT('Ctrl Pts',(-3.54352834466741,-5.76804097443025,
153.627466873079));
#46898=CARTESIAN_POINT('Ctrl Pts',(-3.38357518563572,-5.86330186629665,
153.63621665235));
#46899=CARTESIAN_POINT('Ctrl Pts',(-3.21997030268213,-5.95181319009974,
153.64496643162));
#46900=CARTESIAN_POINT('Ctrl Pts',(-3.05636846790294,-6.0403228648203,153.653716047871));
#46901=CARTESIAN_POINT('Ctrl Pts',(-2.88911529745392,-6.12208308673445,
153.662465664121));
#46902=CARTESIAN_POINT('Ctrl Pts',(-2.71877888751091,-6.19681614708916,
153.671215280372));
#46903=CARTESIAN_POINT('Ctrl Pts',(-2.548445424774,-6.27154791439248,153.679964745234));
#46904=CARTESIAN_POINT('Ctrl Pts',(-2.37502909175458,-6.33925264829314,
153.688714210096));
#46905=CARTESIAN_POINT('Ctrl Pts',(-2.1991188982138,-6.3997003891994,153.697463674959));
#46906=CARTESIAN_POINT('Ctrl Pts',(-2.02321151455511,-6.46014716455032,
153.706213000062));
#46907=CARTESIAN_POINT('Ctrl Pts',(-1.84481062111901,-6.5133370857405,153.714962325166));
#46908=CARTESIAN_POINT('Ctrl Pts',(-1.66452213842223,-6.55908949860438,
153.72371165027));
#46909=CARTESIAN_POINT('Ctrl Pts',(-1.48423629599081,-6.60484124143928,
153.732460847242));
#46910=CARTESIAN_POINT('Ctrl Pts',(-1.30206319737382,-6.64315562342162,
153.741210044215));
#46911=CARTESIAN_POINT('Ctrl Pts',(-1.11862155689613,-6.67390251745164,
153.749959241188));
#46912=CARTESIAN_POINT('Ctrl Pts',(-0.935182359145258,-6.704649002053,153.758708321655));
#46913=CARTESIAN_POINT('Ctrl Pts',(-0.750474935937235,-6.72782815298643,
153.767457402123));
#46914=CARTESIAN_POINT('Ctrl Pts',(-0.565126592231362,-6.74336124901766,
153.77620648259));
#46915=CARTESIAN_POINT('Ctrl Pts',(-0.379780470417673,-6.75889415884347,
153.784955458177));
#46916=CARTESIAN_POINT('Ctrl Pts',(-0.193793729005098,-6.76678117325788,
153.793704433763));
#46917=CARTESIAN_POINT('Ctrl Pts',(-0.00779800265608266,-6.7669955069554,
153.80245340935));
#46918=CARTESIAN_POINT('Ctrl Pts',(0.17821673193395,-6.76720986255722,153.811203279057));
#46919=CARTESIAN_POINT('Ctrl Pts',(0.364240166675858,-6.75974996789178,
153.819953148765));
#46920=CARTESIAN_POINT('Ctrl Pts',(0.549640413288921,-6.74464116288477,
153.828703018472));
#46921=CARTESIAN_POINT('Ctrl Pts',(0.735033738525658,-6.72953292192083,
153.837452561528));
#46922=CARTESIAN_POINT('Ctrl Pts',(0.91980363650705,-6.70677636530813,153.846202104585));
#46923=CARTESIAN_POINT('Ctrl Pts',(1.10332252380503,-6.67644878722697,153.854951647641));
#46924=CARTESIAN_POINT('Ctrl Pts',(1.28683553553499,-6.64612218011807,153.863700910571));
#46925=CARTESIAN_POINT('Ctrl Pts',(1.46909733398482,-6.60822508332242,153.872450173501));
#46926=CARTESIAN_POINT('Ctrl Pts',(1.64948889425487,-6.56288620865316,153.881199436431));
#46927=CARTESIAN_POINT('Ctrl Pts',(1.82987563779965,-6.51754854459987,153.889948465742));
#46928=CARTESIAN_POINT('Ctrl Pts',(2.00839196519895,-6.46476957015119,153.898697495054));
#46929=CARTESIAN_POINT('Ctrl Pts',(2.18443160482961,-6.4047285316258,153.907446524365));
#46930=CARTESIAN_POINT('Ctrl Pts',(2.3604849227005,-6.34468282792527,153.916196233474));
#46931=CARTESIAN_POINT('Ctrl Pts',(2.53406089643084,-6.27737402346287,153.924945942583));
#46932=CARTESIAN_POINT('Ctrl Pts',(2.70456994115639,-6.20303074580429,153.933695651692));
#46933=CARTESIAN_POINT('Ctrl Pts',(2.87506802043528,-6.12869224916626,153.942444798107));
#46934=CARTESIAN_POINT('Ctrl Pts',(3.04249930269661,-6.04732029912513,153.951193944521));
#46935=CARTESIAN_POINT('Ctrl Pts',(3.20629514779787,-5.9591912559682,153.959943090936));
#46936=CARTESIAN_POINT('Ctrl Pts',(3.37009610080391,-5.871059464544,153.968692510189));
#46937=CARTESIAN_POINT('Ctrl Pts',(3.53026113741014,-5.77617029410984,153.977441929442));
#46938=CARTESIAN_POINT('Ctrl Pts',(3.68624626164006,-5.67484603302545,153.986191348695));
#46939=CARTESIAN_POINT('Ctrl Pts',(3.76830672481212,-5.62154148981211,153.990794232464));
#46940=CARTESIAN_POINT('Ctrl Pts',(3.84921079545831,-5.56645673171636,153.995397116232));
#46941=CARTESIAN_POINT('Ctrl Pts',(3.92888236737299,-5.50964357679747,154.));
#46942=CARTESIAN_POINT('',(-3.92888236737363,-5.50964357679701,154.));
#46943=CARTESIAN_POINT('Origin',(0.,0.,154.));
#46944=CARTESIAN_POINT('',(-6.76699995627346,0.000769282111940907,153.697179783839));
#46945=CARTESIAN_POINT('Ctrl Pts',(-6.76699995627346,0.000769282111748204,
153.697179783839));
#46946=CARTESIAN_POINT('Ctrl Pts',(-6.76701947092661,-0.170891614425859,
153.705273779468));
#46947=CARTESIAN_POINT('Ctrl Pts',(-6.76050280836558,-0.342746040058435,
153.713367775097));
#46948=CARTESIAN_POINT('Ctrl Pts',(-6.74743188915907,-0.514248870839024,
153.721461770727));
#46949=CARTESIAN_POINT('Ctrl Pts',(-6.73437014253476,-0.685631348659959,
153.729550086355));
#46950=CARTESIAN_POINT('Ctrl Pts',(-6.7147633219503,-0.856662354601882,
153.737638401983));
#46951=CARTESIAN_POINT('Ctrl Pts',(-6.68864541020004,-1.02679675525875,
153.745726717611));
#46952=CARTESIAN_POINT('Ctrl Pts',(-6.66253954073297,-1.19685271141162,
153.753811303929));
#46953=CARTESIAN_POINT('Ctrl Pts',(-6.62992861067414,-1.36601251921381,
153.761895890246));
#46954=CARTESIAN_POINT('Ctrl Pts',(-6.59089844295224,-1.53373619462076,
153.769980476564));
#46955=CARTESIAN_POINT('Ctrl Pts',(-6.55187966162554,-1.70141093946542,
153.77806270434));
#46956=CARTESIAN_POINT('Ctrl Pts',(-6.50644545638599,-1.86765002537015,
153.786144932116));
#46957=CARTESIAN_POINT('Ctrl Pts',(-6.45473272074018,-2.03192384301332,
153.794227159892));
#46958=CARTESIAN_POINT('Ctrl Pts',(-6.40301193775555,-2.19622322432188,
153.802310645393));
#46959=CARTESIAN_POINT('Ctrl Pts',(-6.3450107770592,-2.35855637023451,153.810394130895));
#46960=CARTESIAN_POINT('Ctrl Pts',(-6.28091605110546,-2.51840873548472,
153.818477616396));
#46961=CARTESIAN_POINT('Ctrl Pts',(-6.22169455239901,-2.66610726295361,
153.825946501223));
#46962=CARTESIAN_POINT('Ctrl Pts',(-6.15727148173902,-2.81168785811568,
153.83341538605));
#46963=CARTESIAN_POINT('Ctrl Pts',(-6.08783061025201,-2.95476013592959,
153.840884270877));
#46964=CARTESIAN_POINT('Ctrl Pts',(-5.99896118095524,-3.13786198078316,
153.850442842332));
#46965=CARTESIAN_POINT('Ctrl Pts',(-5.901916903247,-3.3167679087119,153.860001413788));
#46966=CARTESIAN_POINT('Ctrl Pts',(-5.79710256826938,-3.49082953077983,
153.869559985244));
#46967=CARTESIAN_POINT('Ctrl Pts',(-5.69197696941553,-3.66540805824244,
153.879146942492));
#46968=CARTESIAN_POINT('Ctrl Pts',(-5.57903518394445,-3.83511339336938,
153.888733899741));
#46969=CARTESIAN_POINT('Ctrl Pts',(-5.45872656148091,-3.99932410876923,
153.89832085699));
#46970=CARTESIAN_POINT('Ctrl Pts',(-5.33816688849719,-4.16387748610534,
153.907927819542));
#46971=CARTESIAN_POINT('Ctrl Pts',(-5.2102096778897,-4.32291321352696,153.917534782095));
#46972=CARTESIAN_POINT('Ctrl Pts',(-5.07534690357434,-4.47583989977058,
153.927141744648));
#46973=CARTESIAN_POINT('Ctrl Pts',(-4.94048239335081,-4.62876855443496,
153.936748830859));
#46974=CARTESIAN_POINT('Ctrl Pts',(-4.79871221545128,-4.77558793666736,
153.946355917069));
#46975=CARTESIAN_POINT('Ctrl Pts',(-4.65056698131552,-4.91574162790294,
153.955963003279));
#46976=CARTESIAN_POINT('Ctrl Pts',(-4.50269287672303,-5.05563881540073,
153.965552506981));
#46977=CARTESIAN_POINT('Ctrl Pts',(-4.34846710060624,-5.18889461150784,
153.975142010682));
#46978=CARTESIAN_POINT('Ctrl Pts',(-4.18845473229509,-5.31499162327796,
153.984731514384));
#46979=CARTESIAN_POINT('Ctrl Pts',(-4.1035304018323,-5.38191585176705,153.989821009589));
#46980=CARTESIAN_POINT('Ctrl Pts',(-4.01697672380024,-5.44682420222127,
153.994910504795));
#46981=CARTESIAN_POINT('Ctrl Pts',(-3.92888236737363,-5.50964357679701,
154.));
#46982=CARTESIAN_POINT('Ctrl Pts',(3.09917575053261,6.01559628526638,153.045781927116));
#46983=CARTESIAN_POINT('Ctrl Pts',(2.94639732302355,6.09430622112099,153.053915280607));
#46984=CARTESIAN_POINT('Ctrl Pts',(2.79037452573701,6.16731781408541,153.062048634097));
#46985=CARTESIAN_POINT('Ctrl Pts',(2.63157606100013,6.23434811629661,153.070181987587));
#46986=CARTESIAN_POINT('Ctrl Pts',(2.47296115830906,6.30130093526874,153.078305939381));
#46987=CARTESIAN_POINT('Ctrl Pts',(2.31157730937803,6.36228608395666,153.086429891174));
#46988=CARTESIAN_POINT('Ctrl Pts',(2.14791895551187,6.41706577499038,153.094553842968));
#46989=CARTESIAN_POINT('Ctrl Pts',(1.98441500867196,6.47179378293556,153.102670130043));
#46990=CARTESIAN_POINT('Ctrl Pts',(1.81864117473825,6.52032787233376,153.110786417118));
#46991=CARTESIAN_POINT('Ctrl Pts',(1.65111305741791,6.56247778446709,153.118902704193));
#46992=CARTESIAN_POINT('Ctrl Pts',(1.48370742648437,6.60459687914409,153.127013057131));
#46993=CARTESIAN_POINT('Ctrl Pts',(1.31455042063434,6.64034100076727,153.13512341007));
#46994=CARTESIAN_POINT('Ctrl Pts',(1.14417401210083,6.66956931368384,153.143233763009));
#46995=CARTESIAN_POINT('Ctrl Pts',(0.973886012015048,6.69878246000665,153.151339907479));
#46996=CARTESIAN_POINT('Ctrl Pts',(0.802380230570611,6.72148646861295,153.159446051949));
#46997=CARTESIAN_POINT('Ctrl Pts',(0.630200046847709,6.73759132783765,153.16755219642));
#46998=CARTESIAN_POINT('Ctrl Pts',(0.456747704672164,6.75381517829787,153.175718233382));
#46999=CARTESIAN_POINT('Ctrl Pts',(0.282611322577518,6.76334188447178,153.183884270344));
#47000=CARTESIAN_POINT('Ctrl Pts',(0.108353414412268,6.76613246527033,153.192050307306));
#47001=CARTESIAN_POINT('Ctrl Pts',(-0.0645940545419908,6.76890206058514,
153.200154934744));
#47002=CARTESIAN_POINT('Ctrl Pts',(-0.237660855314371,6.76503651809403,
153.208259562183));
#47003=CARTESIAN_POINT('Ctrl Pts',(-0.410295751295052,6.7545500513705,153.216364189622));
#47004=CARTESIAN_POINT('Ctrl Pts',(-0.582956388774257,6.74406202101543,
153.224470025538));
#47005=CARTESIAN_POINT('Ctrl Pts',(-0.755184626184368,6.72695112247535,
153.232575861453));
#47006=CARTESIAN_POINT('Ctrl Pts',(-0.926433189663243,6.70328356442501,
153.240681697369));
#47007=CARTESIAN_POINT('Ctrl Pts',(-1.0977402072223,6.67960792767719,153.248790300135));
#47008=CARTESIAN_POINT('Ctrl Pts',(-1.26806652102535,6.64937122536387,153.256898902901));
#47009=CARTESIAN_POINT('Ctrl Pts',(-1.43687397087053,6.6126909947339,153.265007505667));
#47010=CARTESIAN_POINT('Ctrl Pts',(-1.60780895651683,6.57554847109535,153.273218303821));
#47011=CARTESIAN_POINT('Ctrl Pts',(-1.77718615438182,6.53179898737637,153.281429101974));
#47012=CARTESIAN_POINT('Ctrl Pts',(-1.94446249311462,6.48161666660953,153.289639900127));
#47013=CARTESIAN_POINT('Ctrl Pts',(-2.10995223596933,6.43197031840232,153.297763002804));
#47014=CARTESIAN_POINT('Ctrl Pts',(-2.27338545253408,6.37602805559977,153.305886105482));
#47015=CARTESIAN_POINT('Ctrl Pts',(-2.43425670380338,6.31400691320403,153.314009208159));
#47016=CARTESIAN_POINT('Ctrl Pts',(-2.59773305835091,6.25098141807217,153.32226385405));
#47017=CARTESIAN_POINT('Ctrl Pts',(-2.75856339751926,6.181678644642,153.330518499941));
#47018=CARTESIAN_POINT('Ctrl Pts',(-2.91624400533904,6.10637453005662,153.338773145833));
#47019=CARTESIAN_POINT('Ctrl Pts',(-3.07392461315882,6.03107041547123,153.347027791724));
#47020=CARTESIAN_POINT('Ctrl Pts',(-3.22845517768015,5.94976520392367,153.355282437615));
#47021=CARTESIAN_POINT('Ctrl Pts',(-3.37936374480091,5.86278003001351,153.363537083506));
#47022=CARTESIAN_POINT('Ctrl Pts',(-3.53143289885957,5.77512588244229,153.371855213098));
#47023=CARTESIAN_POINT('Ctrl Pts',(-3.68029464888091,5.68143320994216,153.380173342689));
#47024=CARTESIAN_POINT('Ctrl Pts',(-3.82544302852417,5.58195974864705,153.38849147228));
#47025=CARTESIAN_POINT('Ctrl Pts',(-3.97041383648347,5.48260798123564,153.396799425634));
#47026=CARTESIAN_POINT('Ctrl Pts',(-4.11168003741536,5.37748970785892,153.405107378989));
#47027=CARTESIAN_POINT('Ctrl Pts',(-4.24876047979325,5.26690833272681,153.413415332343));
#47028=CARTESIAN_POINT('Ctrl Pts',(-4.38569876832377,5.15644163163315,153.421714670263));
#47029=CARTESIAN_POINT('Ctrl Pts',(-4.51845967542282,5.04052333296863,153.430014008184));
#47030=CARTESIAN_POINT('Ctrl Pts',(-4.64659109393952,4.91949999549974,153.438313346104));
#47031=CARTESIAN_POINT('Ctrl Pts',(-4.77461350413703,4.79857961912153,153.446605623329));
#47032=CARTESIAN_POINT('Ctrl Pts',(-4.89801402012995,4.67256309620952,153.454897900554));
#47033=CARTESIAN_POINT('Ctrl Pts',(-5.01637354724699,4.54183723117425,153.463190177779));
#47034=CARTESIAN_POINT('Ctrl Pts',(-5.13465441379185,4.41119824525717,153.471476944039));
#47035=CARTESIAN_POINT('Ctrl Pts',(-5.24790073360115,4.27585641233802,153.479763710298));
#47036=CARTESIAN_POINT('Ctrl Pts',(-5.35573009431797,4.13623550548284,153.488050476558));
#47037=CARTESIAN_POINT('Ctrl Pts',(-5.46351089017542,3.99667748196166,153.496333510572));
#47038=CARTESIAN_POINT('Ctrl Pts',(-5.56587937520239,3.85284450095779,153.504616544586));
#47039=CARTESIAN_POINT('Ctrl Pts',(-5.66249312863783,3.7051937288257,153.512899578601));
#47040=CARTESIAN_POINT('Ctrl Pts',(-5.75908395288089,3.55757799842255,153.521180646815));
#47041=CARTESIAN_POINT('Ctrl Pts',(-5.84992257501593,3.40614657410768,153.52946171503));
#47042=CARTESIAN_POINT('Ctrl Pts',(-5.93470952527804,3.25138614295106,153.537742783244));
#47043=CARTESIAN_POINT('Ctrl Pts',(-6.01949065779634,3.0966363308406,153.546023283245));
#47044=CARTESIAN_POINT('Ctrl Pts',(-6.09822077806186,2.93855827358451,153.554303783245));
#47045=CARTESIAN_POINT('Ctrl Pts',(-6.17064598217405,2.77766397584,153.562584283246));
#47046=CARTESIAN_POINT('Ctrl Pts',(-6.24307843517748,2.61675357451276,153.570865612025));
#47047=CARTESIAN_POINT('Ctrl Pts',(-6.30920457180915,2.4530266900129,153.579146940804));
#47048=CARTESIAN_POINT('Ctrl Pts',(-6.36881824749775,2.28701620683801,153.587428269583));
#47049=CARTESIAN_POINT('Ctrl Pts',(-6.42847284618091,2.12089176246176,153.595715283245));
#47050=CARTESIAN_POINT('Ctrl Pts',(-6.48160593226592,1.95248091625491,153.604002296907));
#47051=CARTESIAN_POINT('Ctrl Pts',(-6.52806068577934,1.78233349370487,153.612289310569));
#47052=CARTESIAN_POINT('Ctrl Pts',(-6.57453174707025,1.61212634150182,153.620579233358));
#47053=CARTESIAN_POINT('Ctrl Pts',(-6.6143197184717,1.44018173706329,153.628869156146));
#47054=CARTESIAN_POINT('Ctrl Pts',(-6.64731869275697,1.26706084973208,153.637159078935));
#47055=CARTESIAN_POINT('Ctrl Pts',(-6.68035304300543,1.09375437123414,153.645457888788));
#47056=CARTESIAN_POINT('Ctrl Pts',(-6.70658379608069,0.919269435204907,
153.653756698641));
#47057=CARTESIAN_POINT('Ctrl Pts',(-6.72595667241432,0.74417460370888,153.662055508495));
#47058=CARTESIAN_POINT('Ctrl Pts',(-6.74129614728042,0.605534232466989,
153.668626519581));
#47059=CARTESIAN_POINT('Ctrl Pts',(-6.75233709758221,0.466511658131155,
153.675197530667));
#47060=CARTESIAN_POINT('Ctrl Pts',(-6.75907576279589,0.327389420698271,
153.681768541753));
#47061=CARTESIAN_POINT('Ctrl Pts',(-6.76434391201384,0.218626530260761,
153.686905622439));
#47062=CARTESIAN_POINT('Ctrl Pts',(-6.76698757074323,0.109718671431278,
153.692042703124));
#47063=CARTESIAN_POINT('Ctrl Pts',(-6.76699995627339,0.000769282719978384,
153.69717978381));
#47064=CARTESIAN_POINT('Origin',(0.,0.,0.));
#47065=CARTESIAN_POINT('',(-7.91099862725341,0.00453934634078324,0.642148860446907));
#47066=CARTESIAN_POINT('',(3.42067962509757,7.13322310757503,0.));
#47067=CARTESIAN_POINT('Ctrl Pts',(-7.91099862725342,0.00453934634078324,
0.642148860446907));
#47068=CARTESIAN_POINT('Ctrl Pts',(-7.90966797736711,2.20467810308481,0.553622307310889));
#47069=CARTESIAN_POINT('Ctrl Pts',(-6.94102417781289,4.38711985141806,0.465095754174871));
#47070=CARTESIAN_POINT('Ctrl Pts',(-3.67820201488296,7.34180684107626,0.287981765306128));
#47071=CARTESIAN_POINT('Ctrl Pts',(-1.40868175871758,8.08992666571333,0.199394329573404));
#47072=CARTESIAN_POINT('Ctrl Pts',(1.69567364519644,7.7814699249772,0.0738712625604527));
#47073=CARTESIAN_POINT('Ctrl Pts',(2.59296389908065,7.53014751000291,0.0369356312802263));
#47074=CARTESIAN_POINT('Ctrl Pts',(3.42067962509757,7.13322310757503,0.));
#47075=CARTESIAN_POINT('',(-3.42067962509618,7.1332231075757,0.));
#47076=CARTESIAN_POINT('Origin',(0.,0.,0.));
#47077=CARTESIAN_POINT('',(-7.9109995421887,0.00269137328987276,0.357668491799685));
#47078=CARTESIAN_POINT('Ctrl Pts',(-3.42067962509618,7.1332231075757,-6.22634595477876E-14));
#47079=CARTESIAN_POINT('Ctrl Pts',(-3.62731135360407,7.03413452826928,0.00922064556105209));
#47080=CARTESIAN_POINT('Ctrl Pts',(-3.82949148083065,6.926132808479,0.0184412911221664));
#47081=CARTESIAN_POINT('Ctrl Pts',(-4.02653219998454,6.80962256241031,0.0276619366832808));
#47082=CARTESIAN_POINT('Ctrl Pts',(-4.22390059962538,6.69291855875524,0.0368979162608378));
#47083=CARTESIAN_POINT('Ctrl Pts',(-4.41611240780442,6.5676777773061,0.0461338958383948));
#47084=CARTESIAN_POINT('Ctrl Pts',(-4.60250654856346,6.43434957633097,0.0553698754159518));
#47085=CARTESIAN_POINT('Ctrl Pts',(-4.78893874977624,6.30099415061687,0.0646077409196011));
#47086=CARTESIAN_POINT('Ctrl Pts',(-4.96955083114128,6.15954806785506,0.0738456064232504));
#47087=CARTESIAN_POINT('Ctrl Pts',(-5.14371259147606,6.01050262260076,0.0830834719268997));
#47088=CARTESIAN_POINT('Ctrl Pts',(-5.31770286349601,5.86160393489066,0.0923122413695945));
#47089=CARTESIAN_POINT('Ctrl Pts',(-5.48525542973374,5.70512090210243,0.101541010812289));
#47090=CARTESIAN_POINT('Ctrl Pts',(-5.64577433139744,5.54158399728216,0.110769780254984));
#47091=CARTESIAN_POINT('Ctrl Pts',(-5.80575143797907,5.37859907412792,0.119967400083236));
#47092=CARTESIAN_POINT('Ctrl Pts',(-5.95874220013166,5.20860787913774,0.129165019911488));
#47093=CARTESIAN_POINT('Ctrl Pts',(-6.10419004227923,5.03217496990507,0.13836263973974));
#47094=CARTESIAN_POINT('Ctrl Pts',(-6.21358399872687,4.89947658329754,0.145280336200942));
#47095=CARTESIAN_POINT('Ctrl Pts',(-6.31871173245749,4.76313504531534,0.152198032662144));
#47096=CARTESIAN_POINT('Ctrl Pts',(-6.41934941157972,4.62340503655597,0.159115729123346));
#47097=CARTESIAN_POINT('Ctrl Pts',(-6.53431466778682,4.4637819570399,0.167018283643299));
#47098=CARTESIAN_POINT('Ctrl Pts',(-6.64335809141854,4.29981903155955,0.174920838163251));
#47099=CARTESIAN_POINT('Ctrl Pts',(-6.74614773335647,4.13199851884404,0.182823392683204));
#47100=CARTESIAN_POINT('Ctrl Pts',(-6.84892595283971,3.96419665511074,0.19072506903519));
#47101=CARTESIAN_POINT('Ctrl Pts',(-6.94545159618463,3.79253835114268,0.198626745387175));
#47102=CARTESIAN_POINT('Ctrl Pts',(-7.03543686180464,3.61753357462795,0.20652842173916));
#47103=CARTESIAN_POINT('Ctrl Pts',(-7.12542708494852,3.44251915664191,0.214430533415183));
#47104=CARTESIAN_POINT('Ctrl Pts',(-7.20887605615657,3.26415820451004,0.222332645091205));
#47105=CARTESIAN_POINT('Ctrl Pts',(-7.28554250781484,3.08298416584046,0.230234756767228));
#47106=CARTESIAN_POINT('Ctrl Pts',(-7.36225435229779,2.90170285728692,0.238141547141196));
#47107=CARTESIAN_POINT('Ctrl Pts',(-7.43217551890899,2.71760545062612,0.246048337515164));
#47108=CARTESIAN_POINT('Ctrl Pts',(-7.49511303977695,2.53124505351923,0.253955127889132));
#47109=CARTESIAN_POINT('Ctrl Pts',(-7.55807012074251,2.34482673821814,0.261864375582507));
#47110=CARTESIAN_POINT('Ctrl Pts',(-7.61403912746857,2.15614435839489,0.269773623275881));
#47111=CARTESIAN_POINT('Ctrl Pts',(-7.66287724009551,1.9657653479564,0.277682870969256));
#47112=CARTESIAN_POINT('Ctrl Pts',(-7.71176225471301,1.77520350583035,0.28559971435871));
#47113=CARTESIAN_POINT('Ctrl Pts',(-7.75350261574405,1.58294211241716,0.293516557748164));
#47114=CARTESIAN_POINT('Ctrl Pts',(-7.78800659475649,1.38955902358606,0.301433401137619));
#47115=CARTESIAN_POINT('Ctrl Pts',(-7.81241025252054,1.25278480645919,0.30703275350733));
#47116=CARTESIAN_POINT('Ctrl Pts',(-7.83319511826985,1.11544967373295,0.312632105877042));
#47117=CARTESIAN_POINT('Ctrl Pts',(-7.85034443405357,0.977759309198411,
0.318231458246754));
#47118=CARTESIAN_POINT('Ctrl Pts',(-7.89060612247121,0.654501715431181,
0.331377136085626));
#47119=CARTESIAN_POINT('Ctrl Pts',(-7.91088858436064,0.328839751290012,
0.344522813924497));
#47120=CARTESIAN_POINT('Ctrl Pts',(-7.91099954218839,0.00269137419092156,
0.357668491763368));
#47121=CARTESIAN_POINT('',(-7.91099984610374,0.00110339172886062,2.35766849176338));
#47122=CARTESIAN_POINT('Ctrl Pts',(-7.9109995421887,0.00269137328987276,
0.357668491799686));
#47123=CARTESIAN_POINT('Ctrl Pts',(-7.91106612671522,-0.193026612311905,
0.365557065733029));
#47124=CARTESIAN_POINT('Ctrl Pts',(-7.90386535789137,-0.38893260034787,
0.373445639666373));
#47125=CARTESIAN_POINT('Ctrl Pts',(-7.88938173600258,-0.58444574053446,
0.381334213599717));
#47126=CARTESIAN_POINT('Ctrl Pts',(-7.8749084006657,-0.779820023460108,
0.38921718491337));
#47127=CARTESIAN_POINT('Ctrl Pts',(-7.85316254236865,-0.974801671083165,
0.397100156227022));
#47128=CARTESIAN_POINT('Ctrl Pts',(-7.82418072132649,-1.16881009579097,
0.404983127540675));
#47129=CARTESIAN_POINT('Ctrl Pts',(-7.79521407261338,-1.36271695477407,
0.412861972024807));
#47130=CARTESIAN_POINT('Ctrl Pts',(-7.7590190599732,-1.55565126495248,0.420740816508939));
#47131=CARTESIAN_POINT('Ctrl Pts',(-7.7156840782254,-1.74703755111877,0.428619660993071));
#47132=CARTESIAN_POINT('Ctrl Pts',(-7.67236369316935,-1.93835937189216,
0.436495851615135));
#47133=CARTESIAN_POINT('Ctrl Pts',(-7.62190820812512,-2.12813387105543,
0.444372042237198));
#47134=CARTESIAN_POINT('Ctrl Pts',(-7.56445716738786,-2.315795492429,0.452248232859261));
#47135=CARTESIAN_POINT('Ctrl Pts',(-7.50700354853349,-2.50346553512323,
0.460124776925605));
#47136=CARTESIAN_POINT('Ctrl Pts',(-7.44255383927082,-2.68902217738124,
0.46800132099195));
#47137=CARTESIAN_POINT('Ctrl Pts',(-7.37129771049221,-2.87191418104586,
0.475877865058294));
#47138=CARTESIAN_POINT('Ctrl Pts',(-7.30003652999233,-3.05481915088534,
0.483754967534222));
#47139=CARTESIAN_POINT('Ctrl Pts',(-7.22196809318516,-3.23505878302041,
0.491632070010151));
#47140=CARTESIAN_POINT('Ctrl Pts',(-7.13733056290994,-3.4121010295347,0.499509172486079));
#47141=CARTESIAN_POINT('Ctrl Pts',(-7.05267271493674,-3.58918577600005,
0.507388165903161));
#47142=CARTESIAN_POINT('Ctrl Pts',(-6.9614427801441,-3.76307129523202,0.515267159320242));
#47143=CARTESIAN_POINT('Ctrl Pts',(-6.86392539657377,-3.93324918486862,
0.523146152737324));
#47144=CARTESIAN_POINT('Ctrl Pts',(-6.76636810703079,-4.10349671454231,
0.531028370388735));
#47145=CARTESIAN_POINT('Ctrl Pts',(-6.66251841354984,-4.27003329147758,
0.538910588040146));
#47146=CARTESIAN_POINT('Ctrl Pts',(-6.55270499322013,-4.43237839898942,
0.546792805691557));
#47147=CARTESIAN_POINT('Ctrl Pts',(-6.44276429118574,-4.59491167623469,
0.554684159403901));
#47148=CARTESIAN_POINT('Ctrl Pts',(-6.32684624659744,-4.75324349162964,
0.562575513116245));
#47149=CARTESIAN_POINT('Ctrl Pts',(-6.20532139862745,-4.90692442775883,
0.570466866828589));
#47150=CARTESIAN_POINT('Ctrl Pts',(-6.08372134841189,-5.06070046502733,
0.578363103883966));
#47151=CARTESIAN_POINT('Ctrl Pts',(-5.95650780183018,-5.2098196229548,0.586259340939343));
#47152=CARTESIAN_POINT('Ctrl Pts',(-5.82408922820781,-5.35386828955231,
0.594155577994721));
#47153=CARTESIAN_POINT('Ctrl Pts',(-5.69147314761481,-5.49813180981411,
0.602063592566027));
#47154=CARTESIAN_POINT('Ctrl Pts',(-5.55363677011433,-5.63730948165375,
0.609971607137334));
#47155=CARTESIAN_POINT('Ctrl Pts',(-5.41102385846469,-5.77102606155317,
0.617879621708641));
#47156=CARTESIAN_POINT('Ctrl Pts',(-5.29931365386042,-5.87576767524552,
0.624074053303617));
#47157=CARTESIAN_POINT('Ctrl Pts',(-5.18467339594249,-5.97715926774425,
0.630268484898594));
#47158=CARTESIAN_POINT('Ctrl Pts',(-5.06732899452634,-6.07503891849531,
0.636462916493571));
#47159=CARTESIAN_POINT('Ctrl Pts',(-4.91907023871337,-6.19870493975095,
0.644289269605917));
#47160=CARTESIAN_POINT('Ctrl Pts',(-4.76603844546121,-6.31714329989183,
0.652115622718264));
#47161=CARTESIAN_POINT('Ctrl Pts',(-4.6086409765581,-6.42995718097637,0.65994197583061));
#47162=CARTESIAN_POINT('Ctrl Pts',(-4.45143333327123,-6.54263500546073,
0.667758890148847));
#47163=CARTESIAN_POINT('Ctrl Pts',(-4.28987078075816,-6.64970165296909,
0.675575804467085));
#47164=CARTESIAN_POINT('Ctrl Pts',(-4.12439613246084,-6.75079828927973,
0.683392718785321));
#47165=CARTESIAN_POINT('Ctrl Pts',(-3.95908852051114,-6.8517928748348,0.691201742415584));
#47166=CARTESIAN_POINT('Ctrl Pts',(-3.78987697509584,-6.94682926645249,
0.699010766045846));
#47167=CARTESIAN_POINT('Ctrl Pts',(-3.61723601415294,-7.03558985572034,
0.706819789676109));
#47168=CARTESIAN_POINT('Ctrl Pts',(-3.4447354099442,-7.12427828281785,0.714622464586765));
#47169=CARTESIAN_POINT('Ctrl Pts',(-3.26881125517591,-7.20670090797966,
0.72242513949742));
#47170=CARTESIAN_POINT('Ctrl Pts',(-3.08996572640634,-7.28258421232698,
0.730227814408076));
#47171=CARTESIAN_POINT('Ctrl Pts',(-2.9112304847738,-7.35842072236838,0.738025677710171));
#47172=CARTESIAN_POINT('Ctrl Pts',(-2.72957778154651,-7.42772580607952,
0.745823541012267));
#47173=CARTESIAN_POINT('Ctrl Pts',(-2.54553314591733,-7.49027249190817,
0.753621404314362));
#47174=CARTESIAN_POINT('Ctrl Pts',(-2.3615658817154,-7.55279288342873,0.76141598943445));
#47175=CARTESIAN_POINT('Ctrl Pts',(-2.17520902235627,-7.60856042377065,
0.769210574554537));
#47176=CARTESIAN_POINT('Ctrl Pts',(-1.98700692466844,-7.65739671698676,
0.777005159674624));
#47177=CARTESIAN_POINT('Ctrl Pts',(-1.79881702477839,-7.70622984501377,
0.784799239610262));
#47178=CARTESIAN_POINT('Ctrl Pts',(-1.60878246449003,-7.74813252360481,
0.792593319545901));
#47179=CARTESIAN_POINT('Ctrl Pts',(-1.41746199545339,-7.78297645450925,
0.800387399481539));
#47180=CARTESIAN_POINT('Ctrl Pts',(-1.22613925784472,-7.81782079857369,
0.808181571835054));
#47181=CARTESIAN_POINT('Ctrl Pts',(-1.033530928811,-7.84560616405464,0.81597574418857));
#47182=CARTESIAN_POINT('Ctrl Pts',(-0.840205128118094,-7.86625554776121,
0.823769916542086));
#47183=CARTESIAN_POINT('Ctrl Pts',(-0.646842666975414,-7.88690884721877,
0.831565566907657));
#47184=CARTESIAN_POINT('Ctrl Pts',(-0.452762814686121,-7.9004234319023,
0.839361217273228));
#47185=CARTESIAN_POINT('Ctrl Pts',(-0.258538107664255,-7.90677425040613,
0.8471568676388));
#47186=CARTESIAN_POINT('Ctrl Pts',(-0.0642420383565574,-7.91312740233567,
0.854955382292021));
#47187=CARTESIAN_POINT('Ctrl Pts',(0.130198638675183,-7.91231153399614,
0.862753896945242));
#47188=CARTESIAN_POINT('Ctrl Pts',(0.324211961902205,-7.90435371195897,
0.870552411598464));
#47189=CARTESIAN_POINT('Ctrl Pts',(0.518434713335572,-7.89638729982929,
0.878359344379414));
#47190=CARTESIAN_POINT('Ctrl Pts',(0.71222883633158,-7.88126355082138,0.886166277160364));
#47191=CARTESIAN_POINT('Ctrl Pts',(0.905027021324463,-7.85906146372915,
0.893973209941314));
#47192=CARTESIAN_POINT('Ctrl Pts',(1.09794061974251,-7.83684608595726,0.901784816131675));
#47193=CARTESIAN_POINT('Ctrl Pts',(1.28985674377954,-7.80754397955293,0.909596422322036));
#47194=CARTESIAN_POINT('Ctrl Pts',(1.48021879727392,-7.77128517763934,0.917408028512397));
#47195=CARTESIAN_POINT('Ctrl Pts',(1.67084401425626,-7.7349762502275,0.925230433753797));
#47196=CARTESIAN_POINT('Ctrl Pts',(1.85991052628593,-7.69169149718788,0.933052838995197));
#47197=CARTESIAN_POINT('Ctrl Pts',(2.04687628812262,-7.64161098598466,0.940875244236597));
#47198=CARTESIAN_POINT('Ctrl Pts',(2.15697474602777,-7.61212009417424,0.945481621071194));
#47199=CARTESIAN_POINT('Ctrl Pts',(2.26634507620393,-7.58027358173682,0.950087997905792));
#47200=CARTESIAN_POINT('Ctrl Pts',(2.37488002166888,-7.54611594680853,0.954694374740389));
#47201=CARTESIAN_POINT('Ctrl Pts',(2.56153944077685,-7.4873713252813,0.962616464906417));
#47202=CARTESIAN_POINT('Ctrl Pts',(2.74626565333976,-7.42161887265386,0.970538555072446));
#47203=CARTESIAN_POINT('Ctrl Pts',(2.92849514242134,-7.34900246297514,0.978460645238474));
#47204=CARTESIAN_POINT('Ctrl Pts',(3.11052681834732,-7.2764648796226,0.986374135843243));
#47205=CARTESIAN_POINT('Ctrl Pts',(3.29006685295937,-7.19707830715971,0.994287626448011));
#47206=CARTESIAN_POINT('Ctrl Pts',(3.46656583453685,-7.11103665542668,1.00220111705278));
#47207=CARTESIAN_POINT('Ctrl Pts',(3.6429057122888,-7.02507256536467,1.01010747409441));
#47208=CARTESIAN_POINT('Ctrl Pts',(3.81620969119175,-6.93246549712835,1.01801383113605));
#47209=CARTESIAN_POINT('Ctrl Pts',(3.98594705941756,-6.83345791232525,1.02592018817768));
#47210=CARTESIAN_POINT('Ctrl Pts',(4.15556265334386,-6.73452135831173,1.03382087297931));
#47211=CARTESIAN_POINT('Ctrl Pts',(4.32161643909138,-6.62919360925994,1.04172155778094));
#47212=CARTESIAN_POINT('Ctrl Pts',(4.48360083903562,-6.51776376652293,1.04962224258256));
#47213=CARTESIAN_POINT('Ctrl Pts',(4.64549882763955,-6.40639336655981,1.05751871272671));
#47214=CARTESIAN_POINT('Ctrl Pts',(4.80333147379025,-6.28892755392932,1.06541518287086));
#47215=CARTESIAN_POINT('Ctrl Pts',(4.95661856809418,-6.16569974702174,1.073311653015));
#47216=CARTESIAN_POINT('Ctrl Pts',(5.10985208654935,-6.04251500984797,1.08120536323933));
#47217=CARTESIAN_POINT('Ctrl Pts',(5.25854295211118,-5.91357250740162,1.08909907346365));
#47218=CARTESIAN_POINT('Ctrl Pts',(5.40224231930561,-5.77924726270676,1.09699278368797));
#47219=CARTESIAN_POINT('Ctrl Pts',(5.54594160696548,-5.64492209235808,1.1048864895433));
#47220=CARTESIAN_POINT('Ctrl Pts',(5.68464914485778,-5.50521441413616,1.11278019539862));
#47221=CARTESIAN_POINT('Ctrl Pts',(5.81795097104388,-5.36053798592358,1.12067390125394));
#47222=CARTESIAN_POINT('Ctrl Pts',(5.9512596551405,-5.21585411461716,1.12856801321269));
#47223=CARTESIAN_POINT('Ctrl Pts',(6.07916183988643,-5.0662012364696,1.13646212517144));
#47224=CARTESIAN_POINT('Ctrl Pts',(6.20128205197944,-4.91202828898589,1.14435623713019));
#47225=CARTESIAN_POINT('Ctrl Pts',(6.32342890329766,-4.75782171031371,1.15225207110549));
#47226=CARTESIAN_POINT('Ctrl Pts',(6.43979105508588,-4.59909336699831,1.16014790508079));
#47227=CARTESIAN_POINT('Ctrl Pts',(6.55003462754972,-4.43632363313359,1.16804373905609));
#47228=CARTESIAN_POINT('Ctrl Pts',(6.66032062550205,-4.27349125992113,1.17594261161773));
#47229=CARTESIAN_POINT('Ctrl Pts',(6.76448315945939,-4.10661468149927,1.18384148417937));
#47230=CARTESIAN_POINT('Ctrl Pts',(6.86223267518691,-3.93620168583841,1.19174035674102));
#47231=CARTESIAN_POINT('Ctrl Pts',(6.96008394357878,-3.76561129823632,1.19964745165877));
#47232=CARTESIAN_POINT('Ctrl Pts',(7.05150868835067,-3.59147743864202,1.20755454657653));
#47233=CARTESIAN_POINT('Ctrl Pts',(7.13626366989418,-3.41433182830089,1.21546164149429));
#47234=CARTESIAN_POINT('Ctrl Pts',(7.2210691804526,-3.23708060772867,1.2233734504443));
#47235=CARTESIAN_POINT('Ctrl Pts',(7.29919686339688,-3.05681437116568,1.23128525939432));
#47236=CARTESIAN_POINT('Ctrl Pts',(7.37045221679219,-2.87408335299851,1.23919706834434));
#47237=CARTESIAN_POINT('Ctrl Pts',(7.4417980846851,-2.69112021463941,1.24711892753448));
#47238=CARTESIAN_POINT('Ctrl Pts',(7.50625407293359,-2.50568636444544,1.25504078672463));
#47239=CARTESIAN_POINT('Ctrl Pts',(7.56367564732459,-2.31834676053195,1.26296264591478));
#47240=CARTESIAN_POINT('Ctrl Pts',(7.58774835862122,-2.23980881991876,1.26628370827225));
#47241=CARTESIAN_POINT('Ctrl Pts',(7.61058537722258,-2.16093606269547,1.26960477062973));
#47242=CARTESIAN_POINT('Ctrl Pts',(7.6321787424618,-2.08177055486773,1.27292583298721));
#47243=CARTESIAN_POINT('Ctrl Pts',(7.68325789520957,-1.89450437278393,1.28078181326463));
#47244=CARTESIAN_POINT('Ctrl Pts',(7.72751443554771,-1.70508658561529,1.28863779354205));
#47245=CARTESIAN_POINT('Ctrl Pts',(7.76476293192005,-1.51405997605129,1.29649377381948));
#47246=CARTESIAN_POINT('Ctrl Pts',(7.80197079559645,-1.32324174875495,1.30434118436419));
#47247=CARTESIAN_POINT('Ctrl Pts',(7.83218577261682,-1.13081853413889,1.3121885949089));
#47248=CARTESIAN_POINT('Ctrl Pts',(7.85527200877326,-0.937348744162689,
1.32003600545361));
#47249=CARTESIAN_POINT('Ctrl Pts',(7.87833750629953,-0.744052750313094,
1.32787636657962));
#47250=CARTESIAN_POINT('Ctrl Pts',(7.89428697580821,-0.54971239878627,1.33571672770562));
#47251=CARTESIAN_POINT('Ctrl Pts',(7.90303543735866,-0.354896993299682,
1.34355708883162));
#47252=CARTESIAN_POINT('Ctrl Pts',(7.91177772381033,-0.160219098204852,
1.35139191584123));
#47253=CARTESIAN_POINT('Ctrl Pts',(7.91332911110288,0.0349328347151123,
1.35922674285084));
#47254=CARTESIAN_POINT('Ctrl Pts',(7.90765632864982,0.229983451501376,1.36706156986045));
#47255=CARTESIAN_POINT('Ctrl Pts',(7.90198645884924,0.424933920843567,1.37489237413015));
#47256=CARTESIAN_POINT('Ctrl Pts',(7.88909981890886,0.619782828602985,1.38272317839985));
#47257=CARTESIAN_POINT('Ctrl Pts',(7.86901521296409,0.81395367075759,1.39055398266955));
#47258=CARTESIAN_POINT('Ctrl Pts',(7.84893705567685,1.00806216957978,1.39838227266662));
#47259=CARTESIAN_POINT('Ctrl Pts',(7.82166557348624,1.20149268878542,1.4062105626637));
#47260=CARTESIAN_POINT('Ctrl Pts',(7.7872715374635,1.39367248728343,1.41403885266077));
#47261=CARTESIAN_POINT('Ctrl Pts',(7.75287507181378,1.58586586154281,1.4218676956556));
#47262=CARTESIAN_POINT('Ctrl Pts',(7.71135510037303,1.77680799242736,1.42969653865042));
#47263=CARTESIAN_POINT('Ctrl Pts',(7.66283385940022,1.96593444530317,1.43752538164525));
#47264=CARTESIAN_POINT('Ctrl Pts',(7.61430794975743,2.15507909575548,1.44535497792428));
#47265=CARTESIAN_POINT('Ctrl Pts',(7.55877951482502,2.34240738059906,1.45318457420331));
#47266=CARTESIAN_POINT('Ctrl Pts',(7.49642118890176,2.52736826730588,1.46101417048234));
#47267=CARTESIAN_POINT('Ctrl Pts',(7.4340459945453,2.71237918743351,1.4688458847307));
#47268=CARTESIAN_POINT('Ctrl Pts',(7.36483734020135,2.89502110168799,1.47667759897906));
#47269=CARTESIAN_POINT('Ctrl Pts',(7.28901675181659,3.07476109506693,1.48450931322742));
#47270=CARTESIAN_POINT('Ctrl Pts',(7.21316243784266,3.254581038197,1.49234451108337));
#47271=CARTESIAN_POINT('Ctrl Pts',(7.13069046659174,3.43149616657611,1.50017970893932));
#47272=CARTESIAN_POINT('Ctrl Pts',(7.04186929690232,3.60499622820114,1.50801490679527));
#47273=CARTESIAN_POINT('Ctrl Pts',(6.952943867529,3.77869994692328,1.51585930172951));
#47274=CARTESIAN_POINT('Ctrl Pts',(6.85765451363545,3.94898028053856,1.52370369666375));
#47275=CARTESIAN_POINT('Ctrl Pts',(6.75631476749142,4.11535317592274,1.531548091598));
#47276=CARTESIAN_POINT('Ctrl Pts',(6.65490817317078,4.28183581822377,1.53939766104193));
#47277=CARTESIAN_POINT('Ctrl Pts',(6.54744342477946,4.44440559427355,1.54724723048585));
#47278=CARTESIAN_POINT('Ctrl Pts',(6.43427573884808,4.6026097723434,1.55509679992978));
#47279=CARTESIAN_POINT('Ctrl Pts',(6.32094554126904,4.76104113559808,1.56295764155316));
#47280=CARTESIAN_POINT('Ctrl Pts',(6.20189626204498,4.91509410335571,1.57081848317654));
#47281=CARTESIAN_POINT('Ctrl Pts',(6.0775222946626,5.06435027993513,1.57867932479992));
#47282=CARTESIAN_POINT('Ctrl Pts',(6.01171364190726,5.1433245870416,1.58283864694462));
#47283=CARTESIAN_POINT('Ctrl Pts',(5.94441486145594,5.22095658309199,1.58699796908932));
#47284=CARTESIAN_POINT('Ctrl Pts',(5.87568825599643,5.29718873727807,1.59115729123402));
#47285=CARTESIAN_POINT('Ctrl Pts',(5.74512415958285,5.4420115793553,1.5990590075182));
#47286=CARTESIAN_POINT('Ctrl Pts',(5.60901247919307,5.58221516921733,1.60696072380238));
#47287=CARTESIAN_POINT('Ctrl Pts',(5.46771201489397,5.71734609081733,1.61486244008655));
#47288=CARTESIAN_POINT('Ctrl Pts',(5.32657659542006,5.85231917387486,1.62275492683713));
#47289=CARTESIAN_POINT('Ctrl Pts',(5.18026471049383,5.98223115281326,1.63064741358771));
#47290=CARTESIAN_POINT('Ctrl Pts',(5.02917515824721,6.10666179083705,1.63853990033829));
#47291=CARTESIAN_POINT('Ctrl Pts',(4.87823377477048,6.23097040364931,1.64642464717545));
#47292=CARTESIAN_POINT('Ctrl Pts',(4.72252432185267,6.34980816445695,1.65430939401261));
#47293=CARTESIAN_POINT('Ctrl Pts',(4.56248235630436,6.46279163739722,1.66219414084976));
#47294=CARTESIAN_POINT('Ctrl Pts',(4.40256736252464,6.57568547315181,1.67007263220107));
#47295=CARTESIAN_POINT('Ctrl Pts',(4.23832698504589,6.68273407523877,1.67795112355238));
#47296=CARTESIAN_POINT('Ctrl Pts',(4.07022996932809,6.78359410613456,1.68582961490369));
#47297=CARTESIAN_POINT('Ctrl Pts',(3.90223483919664,6.88439300457452,1.69370333100835));
#47298=CARTESIAN_POINT('Ctrl Pts',(3.73038802416106,6.97901062793922,1.70157704711301));
#47299=CARTESIAN_POINT('Ctrl Pts',(3.55518759034413,7.06714668005859,1.70945076321767));
#47300=CARTESIAN_POINT('Ctrl Pts',(3.38006054681664,7.15524581257545,1.71732118107534));
#47301=CARTESIAN_POINT('Ctrl Pts',(3.20158299270792,7.23686862926661,1.72519159893301));
#47302=CARTESIAN_POINT('Ctrl Pts',(3.02027818423293,7.31176043712091,1.73306201679067));
#47303=CARTESIAN_POINT('Ctrl Pts',(2.83899039489044,7.38664521486051,1.74093169585004));
#47304=CARTESIAN_POINT('Ctrl Pts',(2.65487619711691,7.45480010438969,1.74880137490941));
#47305=CARTESIAN_POINT('Ctrl Pts',(2.46847990812357,7.51601809093021,1.75667105396878));
#47306=CARTESIAN_POINT('Ctrl Pts',(2.28208477794308,7.57723569688274,1.7645406841029));
#47307=CARTESIAN_POINT('Ctrl Pts',(2.09340791355454,7.63151637715714,1.77241031423701));
#47308=CARTESIAN_POINT('Ctrl Pts',(1.90300999933721,7.67870262104365,1.78027994437113));
#47309=CARTESIAN_POINT('Ctrl Pts',(1.71258097184564,7.72589657572128,1.78815086049602));
#47310=CARTESIAN_POINT('Ctrl Pts',(1.52043067021317,7.76599370087157,1.79602177662091));
#47311=CARTESIAN_POINT('Ctrl Pts',(1.32713143109919,7.79888730298038,1.80389269274579));
#47312=CARTESIAN_POINT('Ctrl Pts',(1.13376781522621,7.83179186003917,1.81176623021608));
#47313=CARTESIAN_POINT('Ctrl Pts',(0.939254840577545,7.85748805622527,1.81963976768636));
#47314=CARTESIAN_POINT('Ctrl Pts',(0.744171676952125,7.87592086776031,1.82751330515665));
#47315=CARTESIAN_POINT('Ctrl Pts',(0.548897500175621,7.89437172754384,1.83539455189909));
#47316=CARTESIAN_POINT('Ctrl Pts',(0.353052364075873,7.90554496486019,1.84327579864153));
#47317=CARTESIAN_POINT('Ctrl Pts',(0.157218223899022,7.90943761781292,1.85115704538398));
#47318=CARTESIAN_POINT('Ctrl Pts',(-0.0387248944192319,7.9133324369563,
1.85904267789706));
#47319=CARTESIAN_POINT('Ctrl Pts',(-0.23465665926724,7.90993860042775,1.86692831041015));
#47320=CARTESIAN_POINT('Ctrl Pts',(-0.429998259737013,7.89930519075084,
1.87481394292323));
#47321=CARTESIAN_POINT('Ctrl Pts',(-0.625581418376249,7.88865863186776,
1.88270932675887));
#47322=CARTESIAN_POINT('Ctrl Pts',(-0.820572611094728,7.87075464924748,
1.89060471059451));
#47323=CARTESIAN_POINT('Ctrl Pts',(-1.01440016151281,7.84569393440267,1.89850009443015));
#47324=CARTESIAN_POINT('Ctrl Pts',(-1.10350376009476,7.83417338497152,1.90212964611371));
#47325=CARTESIAN_POINT('Ctrl Pts',(-1.19236160753875,7.82114111686436,1.90575919779728));
#47326=CARTESIAN_POINT('Ctrl Pts',(-1.28091912361697,7.80661048078821,1.90938874948084));
#47327=CARTESIAN_POINT('Ctrl Pts',(-1.4840743942043,7.77327649136997,1.91771511845594));
#47328=CARTESIAN_POINT('Ctrl Pts',(-1.68610102522148,7.73197959767553,1.92604148743103));
#47329=CARTESIAN_POINT('Ctrl Pts',(-1.88636669581931,7.68280819029759,1.93436785640613));
#47330=CARTESIAN_POINT('Ctrl Pts',(-2.08638212157466,7.63369822575735,1.94268382104739));
#47331=CARTESIAN_POINT('Ctrl Pts',(-2.28464069384541,7.57673344200757,1.95099978568865));
#47332=CARTESIAN_POINT('Ctrl Pts',(-2.48051884884997,7.5120534636343,1.95931575032991));
#47333=CARTESIAN_POINT('Ctrl Pts',(-2.67616425723196,7.44745033939779,1.96762183376373));
#47334=CARTESIAN_POINT('Ctrl Pts',(-2.86943461406105,7.37515039661436,1.97592791719754));
#47335=CARTESIAN_POINT('Ctrl Pts',(-3.05971929268036,7.29534364166621,1.98423400063136));
#47336=CARTESIAN_POINT('Ctrl Pts',(-3.24971045937864,7.21565998771666,1.99252727202732));
#47337=CARTESIAN_POINT('Ctrl Pts',(-3.43672487057012,7.12849274219435,2.00082054342329));
#47338=CARTESIAN_POINT('Ctrl Pts',(-3.62016967077566,7.03408078961253,2.00911381481925));
#47339=CARTESIAN_POINT('Ctrl Pts',(-3.80344077058155,6.93975823391673,2.01739923347394));
#47340=CARTESIAN_POINT('Ctrl Pts',(-3.98314874143098,6.83820478400954,2.02568465212862));
#47341=CARTESIAN_POINT('Ctrl Pts',(-4.15872150952731,6.72970700745544,2.0339700707833));
#47342=CARTESIAN_POINT('Ctrl Pts',(-4.33408484153599,6.6213386550147,2.04224560598232));
#47343=CARTESIAN_POINT('Ctrl Pts',(-4.5053225664823,6.50604265857243,2.05052114118135));
#47344=CARTESIAN_POINT('Ctrl Pts',(-4.67188775381832,6.38415114292593,2.05879667638038));
#47345=CARTESIAN_POINT('Ctrl Pts',(-4.73701876376317,6.33648861725212,2.062032610455));
#47346=CARTESIAN_POINT('Ctrl Pts',(-4.80143561405838,6.28781813039693,2.06526854452963));
#47347=CARTESIAN_POINT('Ctrl Pts',(-4.86510669996793,6.23816141166026,2.06850447860425));
#47348=CARTESIAN_POINT('Ctrl Pts',(-5.0277096124292,6.11134832257107,2.07676839145496));
#47349=CARTESIAN_POINT('Ctrl Pts',(-5.18525920588905,5.97824633454064,2.08503230430567));
#47350=CARTESIAN_POINT('Ctrl Pts',(-5.33728610071854,5.83928917583953,2.09329621715638));
#47351=CARTESIAN_POINT('Ctrl Pts',(-5.48945000238128,5.70020678876818,2.10156757745598));
#47352=CARTESIAN_POINT('Ctrl Pts',(-5.63608105236553,5.555258895159,2.10983893775559));
#47353=CARTESIAN_POINT('Ctrl Pts',(-5.77674712300957,5.40491569562381,2.11811029805519));
#47354=CARTESIAN_POINT('Ctrl Pts',(-5.91754923325907,5.25442709763217,2.12638965767252));
#47355=CARTESIAN_POINT('Ctrl Pts',(-6.05237464655406,5.09853299112444,2.13466901728984));
#47356=CARTESIAN_POINT('Ctrl Pts',(-6.18083133164794,4.93773683479781,2.14294837690717));
#47357=CARTESIAN_POINT('Ctrl Pts',(-6.30950271264577,4.77667193203648,2.15124157422081));
#47358=CARTESIAN_POINT('Ctrl Pts',(-6.43178390076399,4.61068882953579,2.15953477153444));
#47359=CARTESIAN_POINT('Ctrl Pts',(-6.54732487325436,4.44032183564038,2.16782796884807));
#47360=CARTESIAN_POINT('Ctrl Pts',(-6.66297109400047,4.26979965152494,2.17612872057754));
#47361=CARTESIAN_POINT('Ctrl Pts',(-6.77186468438994,4.09488585158791,2.18442947230701));
#47362=CARTESIAN_POINT('Ctrl Pts',(-6.87370083924785,3.91614067322964,2.19273022403647));
#47363=CARTESIAN_POINT('Ctrl Pts',(-6.97569398705812,3.73711993720412,2.20104377239522));
#47364=CARTESIAN_POINT('Ctrl Pts',(-7.07060781210317,3.55425627498662,2.20935732075396));
#47365=CARTESIAN_POINT('Ctrl Pts',(-7.15818420681603,3.36813299340889,2.21767086911271));
#47366=CARTESIAN_POINT('Ctrl Pts',(-7.19312024006662,3.29388457092897,2.22098731531769));
#47367=CARTESIAN_POINT('Ctrl Pts',(-7.22688915641556,3.21911762542658,2.22430376152268));
#47368=CARTESIAN_POINT('Ctrl Pts',(-7.25947675683652,3.14386994275374,2.22762020772766));
#47369=CARTESIAN_POINT('Ctrl Pts',(-7.3438421092644,2.94906280181453,2.23620608546266));
#47370=CARTESIAN_POINT('Ctrl Pts',(-7.42043412903276,2.75069165235358,2.24479196319766));
#47371=CARTESIAN_POINT('Ctrl Pts',(-7.48896670490833,2.54937221542372,2.25337784093267));
#47372=CARTESIAN_POINT('Ctrl Pts',(-7.55833747050121,2.34559053510414,2.26206872850189));
#47373=CARTESIAN_POINT('Ctrl Pts',(-7.61945019851203,2.13878817759546,2.27075961607112));
#47374=CARTESIAN_POINT('Ctrl Pts',(-7.67205674126729,1.9296285546123,2.27945050364034));
#47375=CARTESIAN_POINT('Ctrl Pts',(-7.72377724630503,1.72399175037445,2.28799501294972));
#47376=CARTESIAN_POINT('Ctrl Pts',(-7.76727569579189,1.51607669808758,2.2965395222591));
#47377=CARTESIAN_POINT('Ctrl Pts',(-7.80236435240672,1.30653416040025,2.30508403156849));
#47378=CARTESIAN_POINT('Ctrl Pts',(-7.83835467867448,1.09160702935836,2.31384810826763));
#47379=CARTESIAN_POINT('Ctrl Pts',(-7.86549709841624,0.874967868526115,
2.32261218496678));
#47380=CARTESIAN_POINT('Ctrl Pts',(-7.88364311573386,0.65733722223991,2.33137626166593));
#47381=CARTESIAN_POINT('Ctrl Pts',(-7.90178913305148,0.439706575953708,
2.34014033836508));
#47382=CARTESIAN_POINT('Ctrl Pts',(-7.91093863592887,0.221084715389548,
2.34890441506423));
#47383=CARTESIAN_POINT('Ctrl Pts',(-7.91099969220747,0.00220678346617059,
2.35766849176338));
#47384=CARTESIAN_POINT('',(-7.91099895811926,-0.0034257496853649,4.35766849176336));
#47385=CARTESIAN_POINT('Ctrl Pts',(-7.911,-8.44935232890975E-12,2.35766849176337));
#47386=CARTESIAN_POINT('Ctrl Pts',(-7.91099999999765,-2.20167589667518,
2.4462559274961));
#47387=CARTESIAN_POINT('Ctrl Pts',(-6.94214576671906,-4.38610418339417,
2.53484336322882));
#47388=CARTESIAN_POINT('Ctrl Pts',(-3.67820201487515,-7.34180684108017,
2.71201823469427));
#47389=CARTESIAN_POINT('Ctrl Pts',(-1.40868175870898,-8.08992666571483,
2.800605670427));
#47390=CARTESIAN_POINT('Ctrl Pts',(2.97309270522067,-7.65454228024948,2.97778054189244));
#47391=CARTESIAN_POINT('Ctrl Pts',(5.05102072676269,-6.47444880833704,3.06636797762517));
#47392=CARTESIAN_POINT('Ctrl Pts',(7.66951518848171,-2.93425195366922,3.24354284909062));
#47393=CARTESIAN_POINT('Ctrl Pts',(8.18956872247132,-0.60188196009084,3.33213028482334));
#47394=CARTESIAN_POINT('Ctrl Pts',(7.32306689760967,3.71537198233187,3.50930515628879));
#47395=CARTESIAN_POINT('Ctrl Pts',(5.94329958849633,5.66643518937106,3.59789259202151));
#47396=CARTESIAN_POINT('Ctrl Pts',(2.1615450163706,7.92205913233211,3.77506746348696));
#47397=CARTESIAN_POINT('Ctrl Pts',(-0.21081652930848,8.20894963712981,3.86365489921969));
#47398=CARTESIAN_POINT('Ctrl Pts',(-4.42123908577114,6.91982244717397,4.04082977068514));
#47399=CARTESIAN_POINT('Ctrl Pts',(-6.22631625634709,5.35390358802913,4.12941720641786));
#47400=CARTESIAN_POINT('Ctrl Pts',(-7.65317280859724,2.31334857513753,4.26455925868818));
#47401=CARTESIAN_POINT('Ctrl Pts',(-7.91100000000124,1.157028378357,4.31111387522578));
#47402=CARTESIAN_POINT('Ctrl Pts',(-7.911,-8.4471318828605E-12,4.35766849176337));
#47403=CARTESIAN_POINT('',(-7.91099998419434,-0.000500077126143346,6.35761307316525));
#47404=CARTESIAN_POINT('Ctrl Pts',(-7.91099853652232,-0.00481197898119207,
4.35766849176336));
#47405=CARTESIAN_POINT('Ctrl Pts',(-7.91085957146424,-0.233273569392922,
4.36684708997177));
#47406=CARTESIAN_POINT('Ctrl Pts',(-7.90081999409514,-0.461398660723006,
4.37602568818018));
#47407=CARTESIAN_POINT('Ctrl Pts',(-7.88099117191259,-0.688403332528123,
4.38520428638859));
#47408=CARTESIAN_POINT('Ctrl Pts',(-7.86107949738137,-0.91635651605244,
4.3944212362657));
#47409=CARTESIAN_POINT('Ctrl Pts',(-7.8312966797031,-1.14317980272321,4.40363818614281));
#47410=CARTESIAN_POINT('Ctrl Pts',(-7.7918056249086,-1.36809579476098,4.41285513601991));
#47411=CARTESIAN_POINT('Ctrl Pts',(-7.75212623634786,-1.59408441643826,
4.42211604174709));
#47412=CARTESIAN_POINT('Ctrl Pts',(-7.70264584886791,-1.81814741536919,
4.43137694747427));
#47413=CARTESIAN_POINT('Ctrl Pts',(-7.64357920451689,-2.03951414417183,
4.44063785320145));
#47414=CARTESIAN_POINT('Ctrl Pts',(-7.61253384831106,-2.15586422674899,
4.44550537395275));
#47415=CARTESIAN_POINT('Ctrl Pts',(-7.57884106698765,-2.27146976033907,
4.45037289470406));
#47416=CARTESIAN_POINT('Ctrl Pts',(-7.54253741009926,-2.38622094895949,
4.45524041545537));
#47417=CARTESIAN_POINT('Ctrl Pts',(-7.48354424394224,-2.57269075716126,
4.4631500996323));
#47418=CARTESIAN_POINT('Ctrl Pts',(-7.41755723275975,-2.75720789205596,
4.47105978380923));
#47419=CARTESIAN_POINT('Ctrl Pts',(-7.34472350009437,-2.9392103883801,4.47896946798616));
#47420=CARTESIAN_POINT('Ctrl Pts',(-7.27196366407615,-3.12102822611597,
4.48687112704727));
#47421=CARTESIAN_POINT('Ctrl Pts',(-7.19237107077791,-3.30033619002059,
4.49477278610837));
#47422=CARTESIAN_POINT('Ctrl Pts',(-7.1061427904712,-3.47658678036867,4.50267444516947));
#47423=CARTESIAN_POINT('Ctrl Pts',(-7.01998602260213,-3.65269119930631,
4.51056955108004));
#47424=CARTESIAN_POINT('Ctrl Pts',(-6.92720468165589,-3.82574298818843,
4.51846465699062));
#47425=CARTESIAN_POINT('Ctrl Pts',(-6.82804426171055,-3.99521370643945,
4.52635976290119));
#47426=CARTESIAN_POINT('Ctrl Pts',(-6.72894771435978,-4.16457526284459,
4.53424978330588));
#47427=CARTESIAN_POINT('Ctrl Pts',(-6.62348044823339,-4.33036004812295,
4.54213980371057));
#47428=CARTESIAN_POINT('Ctrl Pts',(-6.51193442959602,-4.49206311004665,
4.55002982411526));
#47429=CARTESIAN_POINT('Ctrl Pts',(-6.40043960678927,-4.65369195576192,
4.5579162232688));
#47430=CARTESIAN_POINT('Ctrl Pts',(-6.28287178631894,-4.8112425281299,4.56580262242234));
#47431=CARTESIAN_POINT('Ctrl Pts',(-6.15956704404111,-4.96423758798495,
4.57368902157588));
#47432=CARTESIAN_POINT('Ctrl Pts',(-6.03629606567186,-5.11719075398323,
4.58157326123697));
#47433=CARTESIAN_POINT('Ctrl Pts',(-5.90729151261009,-5.26559062571781,
4.58945750089806));
#47434=CARTESIAN_POINT('Ctrl Pts',(-5.77293081815939,-5.4089916591492,4.59734174055915));
#47435=CARTESIAN_POINT('Ctrl Pts',(-5.63855444253181,-5.5524094288514,4.60522690038635));
#47436=CARTESIAN_POINT('Ctrl Pts',(-5.49882090709427,-5.69082693830027,
4.61311206021354));
#47437=CARTESIAN_POINT('Ctrl Pts',(-5.35414614578648,-5.82383379309195,
4.62099722004074));
#47438=CARTESIAN_POINT('Ctrl Pts',(-5.20945334281543,-5.95685723450084,
4.62888336318663));
#47439=CARTESIAN_POINT('Ctrl Pts',(-5.05981833949993,-6.08446844284659,
4.63676950633253));
#47440=CARTESIAN_POINT('Ctrl Pts',(-4.90569192378809,-6.20629581545066,
4.64465564947842));
#47441=CARTESIAN_POINT('Ctrl Pts',(-4.75152042760113,-6.32815882137438,
4.65254409924436));
#47442=CARTESIAN_POINT('Ctrl Pts',(-4.59285517151457,-6.4442344065822,4.6604325490103));
#47443=CARTESIAN_POINT('Ctrl Pts',(-4.43017801577483,-6.55419283730235,
4.66832099877624));
#47444=CARTESIAN_POINT('Ctrl Pts',(-4.26742598311092,-6.66420187960985,
4.67621307943216));
#47445=CARTESIAN_POINT('Ctrl Pts',(-4.10065865629295,-6.76808796386108,
4.68410516008808));
#47446=CARTESIAN_POINT('Ctrl Pts',(-3.93038490874541,-6.86556592489697,
4.691997240744));
#47447=CARTESIAN_POINT('Ctrl Pts',(-3.75991376502587,-6.96315689088305,
4.69989847058782));
#47448=CARTESIAN_POINT('Ctrl Pts',(-3.58592838021548,-7.05432472362902,
4.70779970043163));
#47449=CARTESIAN_POINT('Ctrl Pts',(-3.40896119455936,-7.13883075678282,
4.71570093027545));
#47450=CARTESIAN_POINT('Ctrl Pts',(-3.23187674743201,-7.22339278507346,
4.72360739560873));
#47451=CARTESIAN_POINT('Ctrl Pts',(-3.05180687590208,-7.30128407735721,
4.73151386094202));
#47452=CARTESIAN_POINT('Ctrl Pts',(-2.8693020520652,-7.37231488299397,4.7394203262753));
#47453=CARTESIAN_POINT('Ctrl Pts',(-2.68654579668107,-7.44344354569001,
4.74733768411416));
#47454=CARTESIAN_POINT('Ctrl Pts',(-2.50134821293216,-7.50769273055924,
4.75525504195302));
#47455=CARTESIAN_POINT('Ctrl Pts',(-2.31427405444284,-7.56492277560933,
4.76317239979188));
#47456=CARTESIAN_POINT('Ctrl Pts',(-2.23315417186469,-7.58973910819045,
4.76660555776199));
#47457=CARTESIAN_POINT('Ctrl Pts',(-2.15168155942537,-7.61323628552008,
4.77003871573209));
#47458=CARTESIAN_POINT('Ctrl Pts',(-2.06990271671669,-7.63540593179753,
4.77347187370219));
#47459=CARTESIAN_POINT('Ctrl Pts',(-1.88311267735236,-7.68604334562849,
4.78131350719979));
#47460=CARTESIAN_POINT('Ctrl Pts',(-1.69416914107881,-7.72990202532652,
4.78915514069739));
#47461=CARTESIAN_POINT('Ctrl Pts',(-1.50361088955,-7.76679311510398,4.79699677419498));
#47462=CARTESIAN_POINT('Ctrl Pts',(-1.31327700440735,-7.80364076871205,
4.8048291748257));
#47463=CARTESIAN_POINT('Ctrl Pts',(-1.12133253093889,-7.83353710127725,
4.81266157545642));
#47464=CARTESIAN_POINT('Ctrl Pts',(-0.928332353797759,-7.85634266315391,
4.82049397608713));
#47465=CARTESIAN_POINT('Ctrl Pts',(-0.735521847410999,-7.87912581288469,
4.82831867943302));
#47466=CARTESIAN_POINT('Ctrl Pts',(-0.541658049914513,-7.89483202798421,
4.8361433827789));
#47467=CARTESIAN_POINT('Ctrl Pts',(-0.347307203557107,-7.90337261593792,
4.84396808612479));
#47468=CARTESIAN_POINT('Ctrl Pts',(-0.153109544359171,-7.91190647220801,
4.85178662204664));
#47469=CARTESIAN_POINT('Ctrl Pts',(0.0415740495560627,-7.91328593479967,
4.8596051579685));
#47470=CARTESIAN_POINT('Ctrl Pts',(0.236170833643165,-7.90747395426228,
4.86742369389036));
#47471=CARTESIAN_POINT('Ctrl Pts',(0.430652079913269,-7.90166542446816,
4.87523758771817));
#47472=CARTESIAN_POINT('Ctrl Pts',(0.62504626851744,-7.88867396726732,4.88305148154599));
#47473=CARTESIAN_POINT('Ctrl Pts',(0.818779071836284,-7.86851458863253,
4.8908653753738));
#47474=CARTESIAN_POINT('Ctrl Pts',(1.01243451497338,-7.84836325991581,4.89867614900598));
#47475=CARTESIAN_POINT('Ctrl Pts',(1.20542874968516,-7.82104974875847,4.90648692263816));
#47476=CARTESIAN_POINT('Ctrl Pts',(1.39719080189449,-7.78664105138419,4.91429769627034));
#47477=CARTESIAN_POINT('Ctrl Pts',(1.588945233428,-7.75223372142084,4.92210815950027));
#47478=CARTESIAN_POINT('Ctrl Pts',(1.77946723227763,-7.71073182016129,4.92991862273019));
#47479=CARTESIAN_POINT('Ctrl Pts',(1.96819380720538,-7.66225385492274,4.93772908596012));
#47480=CARTESIAN_POINT('Ctrl Pts',(2.15692558742979,-7.61377455260598,4.94553976461163));
#47481=CARTESIAN_POINT('Ctrl Pts',(2.34386150397228,-7.55831888982698,4.95335044326314));
#47482=CARTESIAN_POINT('Ctrl Pts',(2.52845160510943,-7.49605586162614,4.96116112191465));
#47483=CARTESIAN_POINT('Ctrl Pts',(2.71307930626593,-7.43378015077844,4.96897339155976));
#47484=CARTESIAN_POINT('Ctrl Pts',(2.89535990668359,-7.36469442473456,4.97678566120486));
#47485=CARTESIAN_POINT('Ctrl Pts',(3.07476124264891,-7.28901668956137,4.98459793084996));
#47486=CARTESIAN_POINT('Ctrl Pts',(3.25423071902528,-7.21331021038828,4.99241316775984));
#47487=CARTESIAN_POINT('Ctrl Pts',(3.43081842859891,-7.13100687135934,5.00022840466972));
#47488=CARTESIAN_POINT('Ctrl Pts',(3.6040145761508,-7.04237175494822,5.0080436415796));
#47489=CARTESIAN_POINT('Ctrl Pts',(3.77739908255753,-6.95364024373122,5.01586737792262));
#47490=CARTESIAN_POINT('Ctrl Pts',(3.94738434664408,-6.85856336193265,5.02369111426563));
#47491=CARTESIAN_POINT('Ctrl Pts',(4.11348654706754,-6.75745140027617,5.03151485060864));
#47492=CARTESIAN_POINT('Ctrl Pts',(4.27968952566926,-6.6562780915739,5.03934333379963));
#47493=CARTESIAN_POINT('Ctrl Pts',(4.442004452746,-6.54906259908174,5.04717181699063));
#47494=CARTESIAN_POINT('Ctrl Pts',(4.59997859179379,-6.43615707973623,5.05500030018163));
#47495=CARTESIAN_POINT('Ctrl Pts',(4.75817014634896,-6.32309617159784,5.06283955750095));
#47496=CARTESIAN_POINT('Ctrl Pts',(4.91200870294541,-6.2043298095686,5.07067881482026));
#47497=CARTESIAN_POINT('Ctrl Pts',(5.0610756728966,-6.08024950419094,5.07851807213958));
#47498=CARTESIAN_POINT('Ctrl Pts',(5.14465020246199,-6.01068377038913,5.08291315874272));
#47499=CARTESIAN_POINT('Ctrl Pts',(5.22672555110569,-5.93944836820004,5.08730824534587));
#47500=CARTESIAN_POINT('Ctrl Pts',(5.30723332611136,-5.86661703388017,5.09170333194901));
#47501=CARTESIAN_POINT('Ctrl Pts',(5.45212403513974,-5.73554169776082,5.09961321660458));
#47502=CARTESIAN_POINT('Ctrl Pts',(5.59235160506865,-5.59891857292677,5.10752310126014));
#47503=CARTESIAN_POINT('Ctrl Pts',(5.72746461096192,-5.45711188543709,5.1154329859157));
#47504=CARTESIAN_POINT('Ctrl Pts',(5.86243072674516,-5.31545936519276,5.12333427122274));
#47505=CARTESIAN_POINT('Ctrl Pts',(5.99229311804405,-5.1686347545401,5.13123555652978));
#47506=CARTESIAN_POINT('Ctrl Pts',(6.11663398779495,-5.01704192322046,5.13913684183683));
#47507=CARTESIAN_POINT('Ctrl Pts',(6.24086278404226,-4.86558572871025,5.14703100539276));
#47508=CARTESIAN_POINT('Ctrl Pts',(6.35957975544661,-4.70937014007884,5.15492516894869));
#47509=CARTESIAN_POINT('Ctrl Pts',(6.47240430642796,-4.54883539976254,5.16281933250462));
#47510=CARTESIAN_POINT('Ctrl Pts',(6.58514812299098,-4.38841553407917,5.17070784719514));
#47511=CARTESIAN_POINT('Ctrl Pts',(6.69200772217223,-4.22368295542573,5.17859636188567));
#47512=CARTESIAN_POINT('Ctrl Pts',(6.7926429574596,-4.05511068313486,5.18648487657619));
#47513=CARTESIAN_POINT('Ctrl Pts',(6.89322487109512,-3.88662772898379,5.19436921153153));
#47514=CARTESIAN_POINT('Ctrl Pts',(6.98758881606287,-3.71430943059956,5.20225354648687));
#47515=CARTESIAN_POINT('Ctrl Pts',(7.07543798704275,-3.53865769629,5.21013788144221));
#47516=CARTESIAN_POINT('Ctrl Pts',(7.16325692412841,-3.36306641372852,5.21801950294965));
#47517=CARTESIAN_POINT('Ctrl Pts',(7.244565401664,-3.18414428984217,5.22590112445708));
#47518=CARTESIAN_POINT('Ctrl Pts',(7.31911246602694,-3.00241797717257,5.23378274596451));
#47519=CARTESIAN_POINT('Ctrl Pts',(7.39366050701541,-2.82068928374447,5.24166447072743));
#47520=CARTESIAN_POINT('Ctrl Pts',(7.46144681901013,-2.63615664400992,5.24954619549034));
#47521=CARTESIAN_POINT('Ctrl Pts',(7.52226830598668,-2.44936737398625,5.25742792025325));
#47522=CARTESIAN_POINT('Ctrl Pts',(7.58309345699017,-2.26256685134525,5.26531011982948));
#47523=CARTESIAN_POINT('Ctrl Pts',(7.636952839462,-2.07350975555625,5.27319231940571));
#47524=CARTESIAN_POINT('Ctrl Pts',(7.68369301820594,-1.88275930537426,5.28107451898194));
#47525=CARTESIAN_POINT('Ctrl Pts',(7.73044387766686,-1.69196526632228,5.28895851973962));
#47526=CARTESIAN_POINT('Ctrl Pts',(7.77007220956591,-1.49947743699353,5.2968425204973));
#47527=CARTESIAN_POINT('Ctrl Pts',(7.80247550177028,-1.30587022489777,5.30472652125498));
#47528=CARTESIAN_POINT('Ctrl Pts',(7.8348916511138,-1.11218619237123,5.31261365026562));
#47529=CARTESIAN_POINT('Ctrl Pts',(7.86007699153326,-0.91738223213148,5.32050077927626));
#47530=CARTESIAN_POINT('Ctrl Pts',(7.87798073737355,-0.722039127451784,
5.3283879082869));
#47531=CARTESIAN_POINT('Ctrl Pts',(7.89590358450976,-0.526487613510565,
5.33628345198274));
#47532=CARTESIAN_POINT('Ctrl Pts',(7.90652928827996,-0.330396149926966,
5.34417899567859));
#47533=CARTESIAN_POINT('Ctrl Pts',(7.90985914163195,-0.134347904864651,
5.35207453937443));
#47534=CARTESIAN_POINT('Ctrl Pts',(7.91319102275443,0.0618197270910941,
5.3599748911951));
#47535=CARTESIAN_POINT('Ctrl Pts',(7.90921820287093,0.257943743998826,5.36787524301577));
#47536=CARTESIAN_POINT('Ctrl Pts',(7.89799398724836,0.453444569257142,5.37577559483644));
#47537=CARTESIAN_POINT('Ctrl Pts',(7.88675515720779,0.649199945111568,5.38368623325954));
#47538=CARTESIAN_POINT('Ctrl Pts',(7.8682461047889,0.844330166108271,5.39159687168265));
#47539=CARTESIAN_POINT('Ctrl Pts',(7.8425716791579,1.03826319267825,5.39950751010575));
#47540=CARTESIAN_POINT('Ctrl Pts',(7.83129090286285,1.1234730867729,5.40298327013578));
#47541=CARTESIAN_POINT('Ctrl Pts',(7.81862748948768,1.20845201665567,5.4064590301658));
#47542=CARTESIAN_POINT('Ctrl Pts',(7.80459339720012,1.2931523129084,5.40993479019582));
#47543=CARTESIAN_POINT('Ctrl Pts',(7.77265570572528,1.48590663389456,5.41784465349193));
#47544=CARTESIAN_POINT('Ctrl Pts',(7.73352983042176,1.67773721077236,5.42575451678803));
#47545=CARTESIAN_POINT('Ctrl Pts',(7.68727814727843,1.8680673666588,5.43366438008413));
#47546=CARTESIAN_POINT('Ctrl Pts',(7.64107673028992,2.05819067244958,5.44156564697063));
#47547=CARTESIAN_POINT('Ctrl Pts',(7.58776501155819,2.2468164730727,5.44946691385713));
#47548=CARTESIAN_POINT('Ctrl Pts',(7.52745689775621,2.4333749510551,5.45736818074362));
#47549=CARTESIAN_POINT('Ctrl Pts',(7.46720311987403,2.61976534507904,5.46526232881017));
#47550=CARTESIAN_POINT('Ctrl Pts',(7.3999656095018,2.80409180073171,5.47315647687672));
#47551=CARTESIAN_POINT('Ctrl Pts',(7.32590898403179,2.98579613464856,5.48105062494327));
#47552=CARTESIAN_POINT('Ctrl Pts',(7.25190532428576,3.16737051258193,5.48893912706977));
#47553=CARTESIAN_POINT('Ctrl Pts',(7.17109239582628,3.34632618696021,5.49682762919627));
#47554=CARTESIAN_POINT('Ctrl Pts',(7.08368425729333,3.52212128453502,5.50471613132277));
#47555=CARTESIAN_POINT('Ctrl Pts',(6.99632239972878,3.69782330190595,5.51260045663548));
#47556=CARTESIAN_POINT('Ctrl Pts',(6.9023724436189,3.87036776890524,5.5204847819482));
#47557=CARTESIAN_POINT('Ctrl Pts',(6.80209618146223,4.03923365728414,5.52836910726092));
#47558=CARTESIAN_POINT('Ctrl Pts',(6.70185439298216,4.20804149176372,5.53625072204499));
#47559=CARTESIAN_POINT('Ctrl Pts',(6.5952908090014,4.3731729718368,5.54413233682906));
#47560=CARTESIAN_POINT('Ctrl Pts',(6.48271282612842,4.53413226692276,5.55201395161314));
#47561=CARTESIAN_POINT('Ctrl Pts',(6.37013330588394,4.69509376007823,5.559895674029));
#47562=CARTESIAN_POINT('Ctrl Pts',(6.25153941333028,4.85188266684265,5.56777739644486));
#47563=CARTESIAN_POINT('Ctrl Pts',(6.12728180067544,5.00403224760907,5.57565911886072));
#47564=CARTESIAN_POINT('Ctrl Pts',(6.00301665946148,5.15619104686191,5.58354131881685));
#47565=CARTESIAN_POINT('Ctrl Pts',(5.87308733223298,5.30370969227481,5.59142351877298));
#47566=CARTESIAN_POINT('Ctrl Pts',(5.73788469627472,5.4461546261795,5.5993057187291));
#47567=CARTESIAN_POINT('Ctrl Pts',(5.60265111798718,5.58863215987797,5.607189722597));
#47568=CARTESIAN_POINT('Ctrl Pts',(5.46214206372018,5.72603341797021,5.6150737264649));
#47569=CARTESIAN_POINT('Ctrl Pts',(5.31678535237621,5.85796163496807,5.6229577303328));
#47570=CARTESIAN_POINT('Ctrl Pts',(5.17137091527017,5.98994224484682,5.63084486518878));
#47571=CARTESIAN_POINT('Ctrl Pts',(5.02110524036368,6.11644525098225,5.63873200004477));
#47572=CARTESIAN_POINT('Ctrl Pts',(4.86644947338875,6.23711395782972,5.64661913490075));
#47573=CARTESIAN_POINT('Ctrl Pts',(4.71162862559173,6.3579114674352,5.65451468854855));
#47574=CARTESIAN_POINT('Ctrl Pts',(4.55240859789324,6.47286202630655,5.66241024219636));
#47575=CARTESIAN_POINT('Ctrl Pts',(4.38928069598927,6.58165146234712,5.67030579584416));
#47576=CARTESIAN_POINT('Ctrl Pts',(4.22605340599731,6.69050717996132,5.67820615997486));
#47577=CARTESIAN_POINT('Ctrl Pts',(4.05891378832009,6.79319411100993,5.68610652410555));
#47578=CARTESIAN_POINT('Ctrl Pts',(3.88837824456623,6.88944378213394,5.69400688823624));
#47579=CARTESIAN_POINT('Ctrl Pts',(3.71762058035253,6.98581881727732,5.70191754249458));
#47580=CARTESIAN_POINT('Ctrl Pts',(3.54345846071086,7.07573968723102,5.70982819675292));
#47581=CARTESIAN_POINT('Ctrl Pts',(3.36642981088409,7.15898535606764,5.71773885101126));
#47582=CARTESIAN_POINT('Ctrl Pts',(3.28864660744725,7.19556200510547,5.72121465015505));
#47583=CARTESIAN_POINT('Ctrl Pts',(3.21031022542822,7.23085060300295,5.72469044929885));
#47584=CARTESIAN_POINT('Ctrl Pts',(3.13146723383428,7.26483543952802,5.72816624844264));
#47585=CARTESIAN_POINT('Ctrl Pts',(2.95365582650221,7.34148006561724,5.73600507754929));
#47586=CARTESIAN_POINT('Ctrl Pts',(2.77276024579775,7.41170845372168,5.74384390665593));
#47587=CARTESIAN_POINT('Ctrl Pts',(2.58928861157229,7.47525955977329,5.75168273576258));
#47588=CARTESIAN_POINT('Ctrl Pts',(2.40602264600011,7.53873942609104,5.75951277767205));
#47589=CARTESIAN_POINT('Ctrl Pts',(2.22018670579099,7.59555680085031,5.76734281958153));
#47590=CARTESIAN_POINT('Ctrl Pts',(2.03231158941905,7.64549740720073,5.775172861491));
#47591=CARTESIAN_POINT('Ctrl Pts',(1.84461051228267,7.69539175077233,5.78299564999441));
#47592=CARTESIAN_POINT('Ctrl Pts',(1.65487435830366,7.7384219224363,5.79081843849782));
#47593=CARTESIAN_POINT('Ctrl Pts',(1.46365208603583,7.77442239468907,5.79864122700123));
#47594=CARTESIAN_POINT('Ctrl Pts',(1.27256975658462,7.8103965205993,5.80645829052792));
#47595=CARTESIAN_POINT('Ctrl Pts',(1.08000381908775,7.83935112883234,5.81427535405461));
#47596=CARTESIAN_POINT('Ctrl Pts',(0.88651670175689,7.86117097750113,5.8220924175813));
#47597=CARTESIAN_POINT('Ctrl Pts',(0.693133560898,7.8829791005785,5.82990528035965));
#47598=CARTESIAN_POINT('Ctrl Pts',(0.498830574925137,7.89766006236304,5.83771814313801));
#47599=CARTESIAN_POINT('Ctrl Pts',(0.304178823781853,7.90514998233194,5.84553100591636));
#47600=CARTESIAN_POINT('Ctrl Pts',(0.109593833991573,7.91263733341981,5.85334118905126));
#47601=CARTESIAN_POINT('Ctrl Pts',(-0.085339331573861,7.9129385432862,5.86115137218617));
#47602=CARTESIAN_POINT('Ctrl Pts',(-0.280045841120314,7.90604169776957,
5.86896155532107));
#47603=CARTESIAN_POINT('Ctrl Pts',(-0.47476113216939,7.89914454119675,5.87677209070482));
#47604=CARTESIAN_POINT('Ctrl Pts',(-0.669249394896092,7.8850486838601,5.88458262608857));
#47605=CARTESIAN_POINT('Ctrl Pts',(-0.862936648121897,7.86379433488238,
5.89239316147232));
#47606=CARTESIAN_POINT('Ctrl Pts',(-1.05663942563658,7.84253828234054,5.90020432288079));
#47607=CARTESIAN_POINT('Ctrl Pts',(-1.24954071573259,7.81412263277778,5.90801548428925));
#47608=CARTESIAN_POINT('Ctrl Pts',(-1.44107259283951,7.77863939144673,5.91582664569772));
#47609=CARTESIAN_POINT('Ctrl Pts',(-1.6326535540037,7.74314705679151,5.92363980887999));
#47610=CARTESIAN_POINT('Ctrl Pts',(-1.82286405703168,7.70058358625159,5.93145297206225));
#47611=CARTESIAN_POINT('Ctrl Pts',(-2.0111471371933,7.65109196079613,5.93926613524452));
